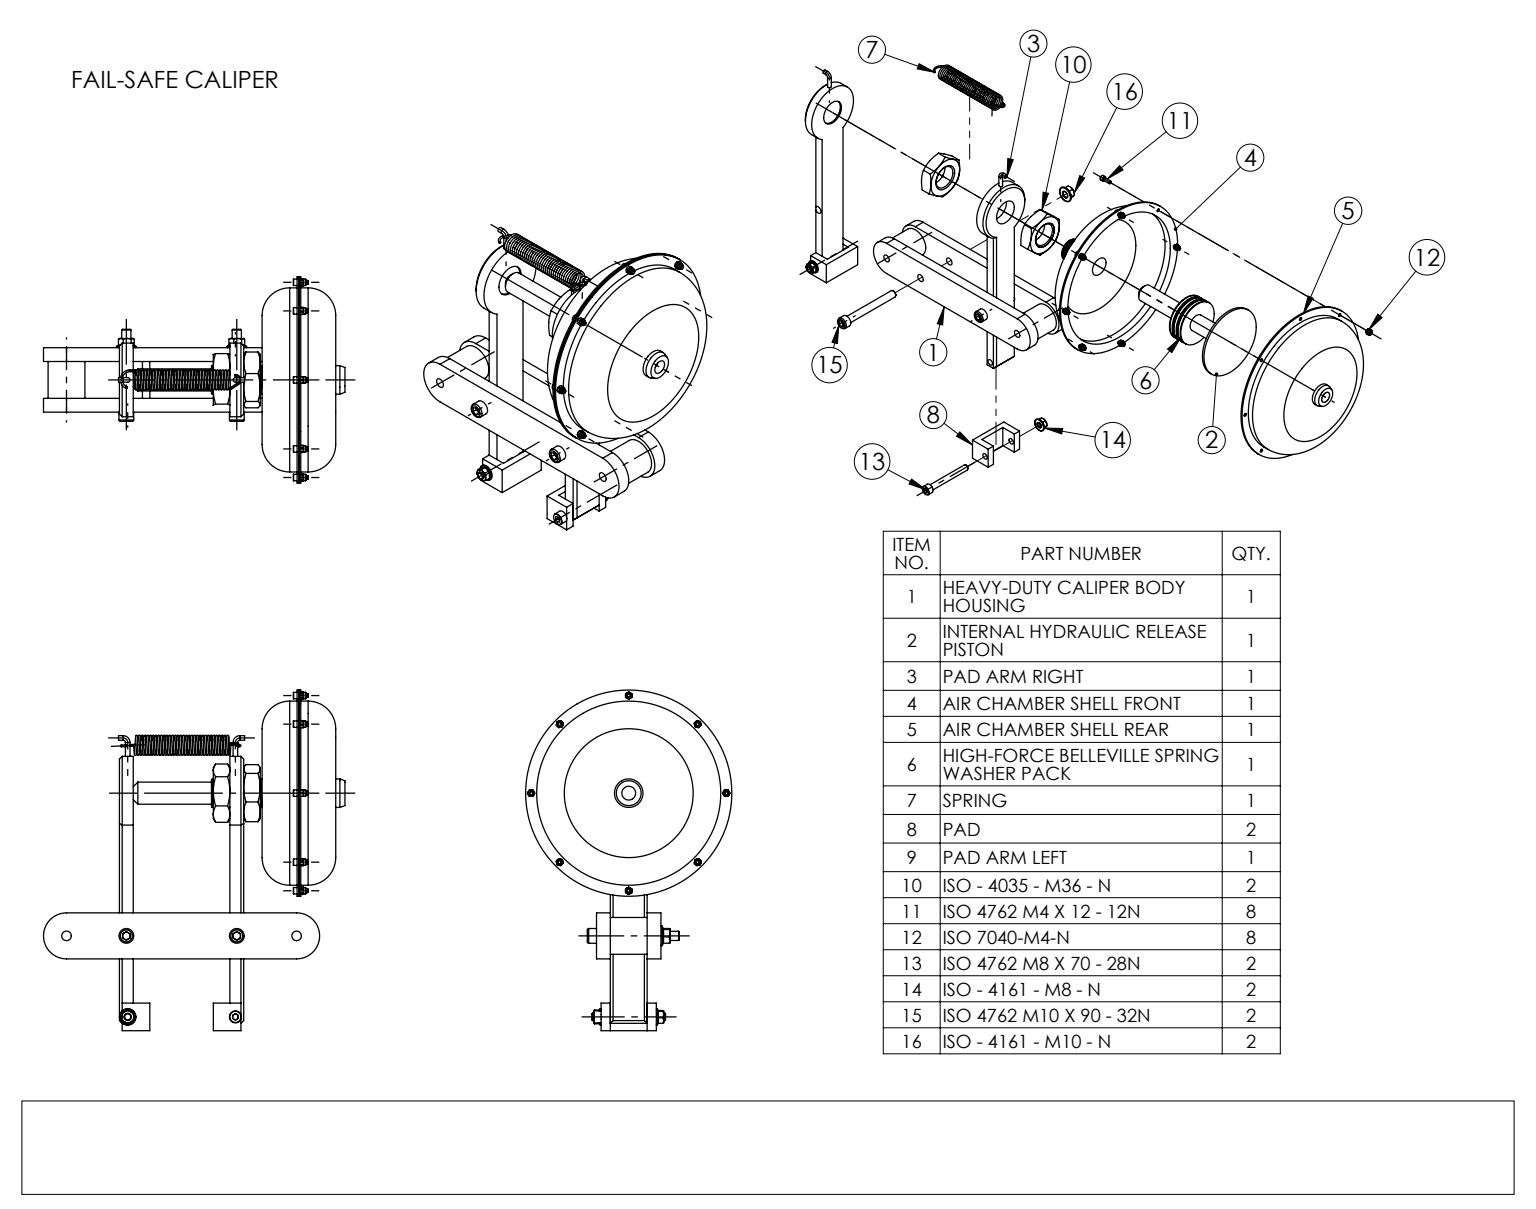
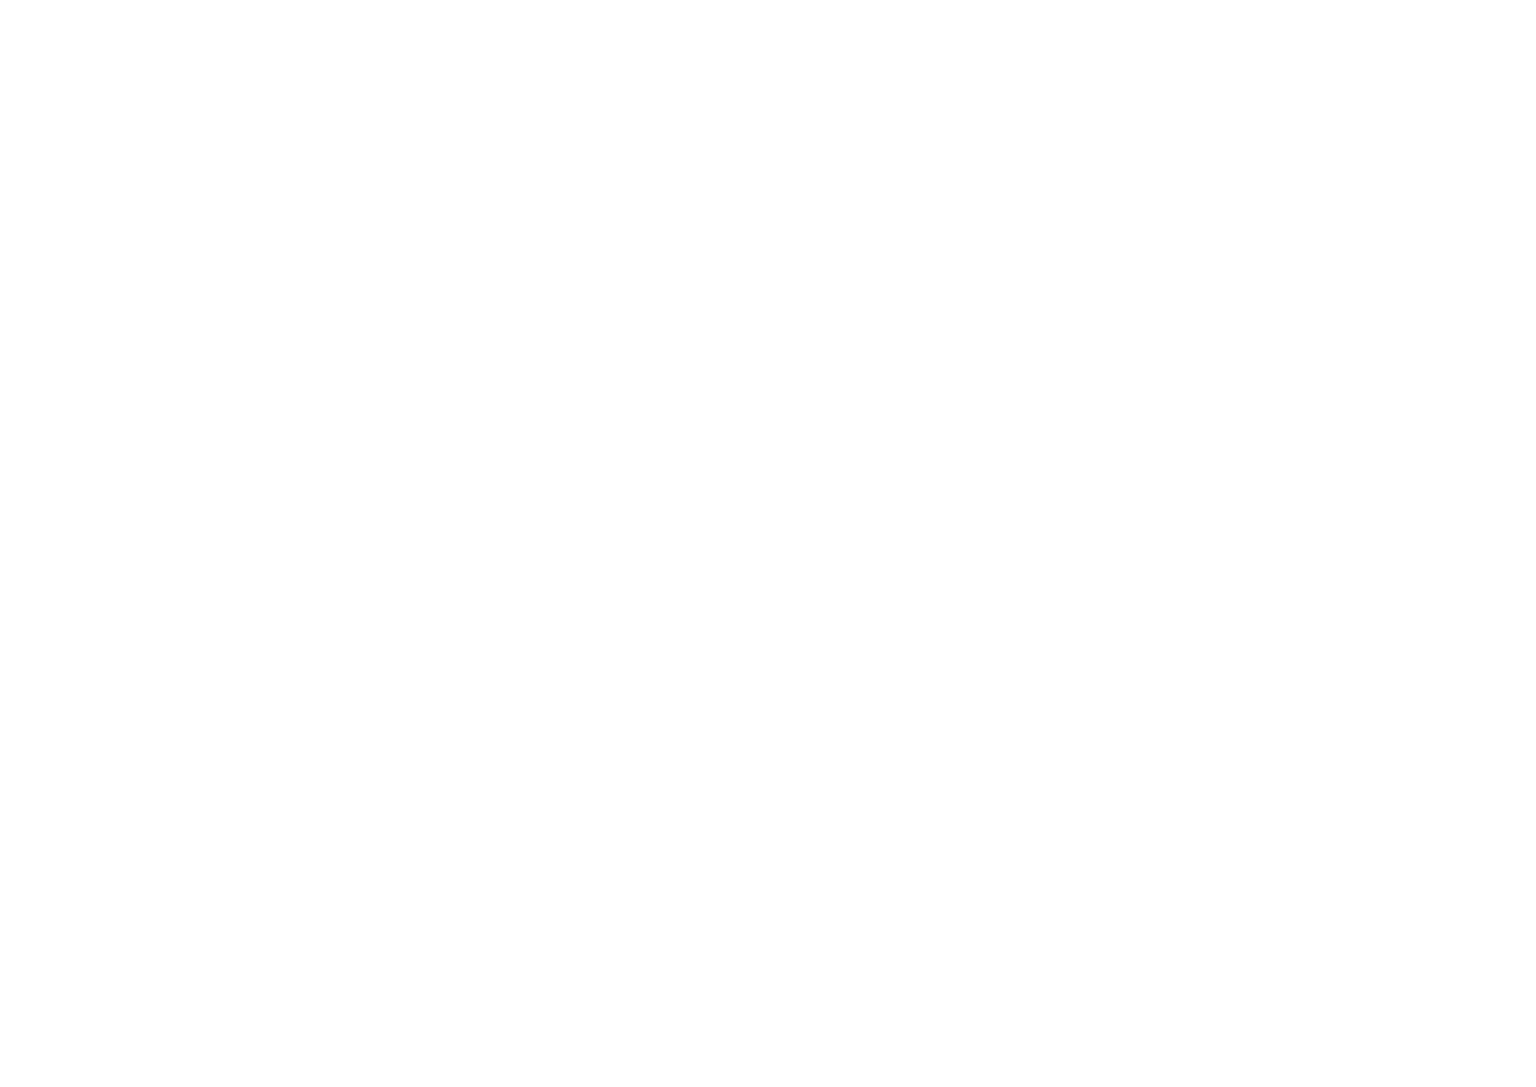
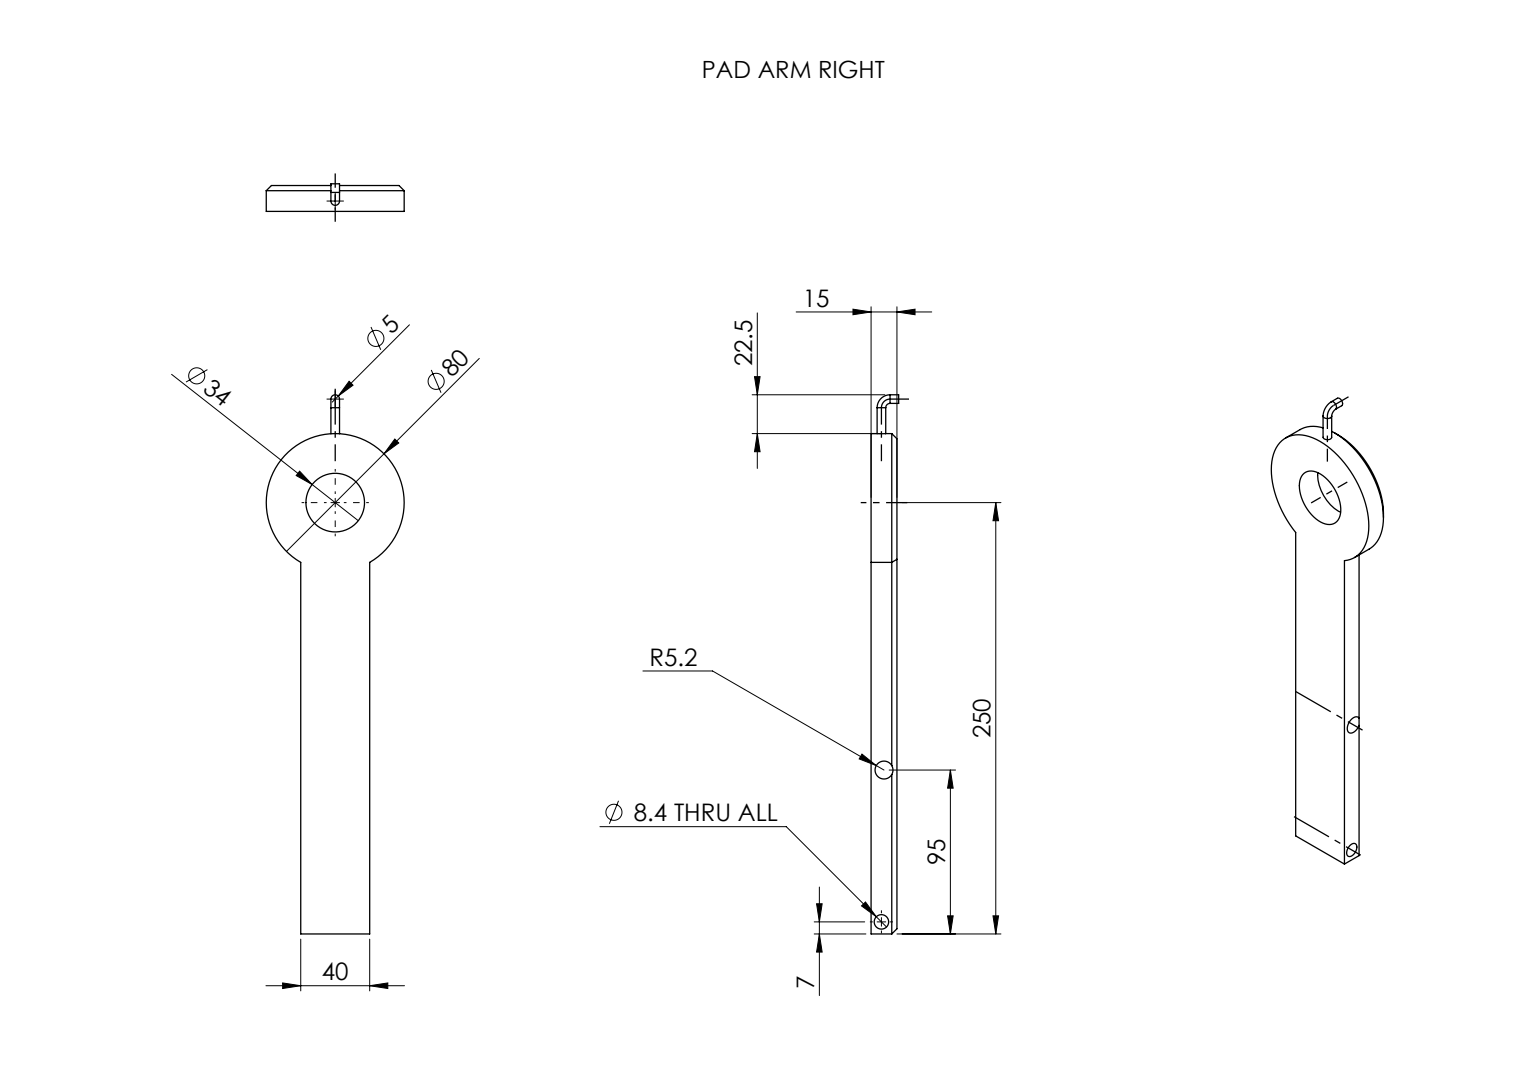
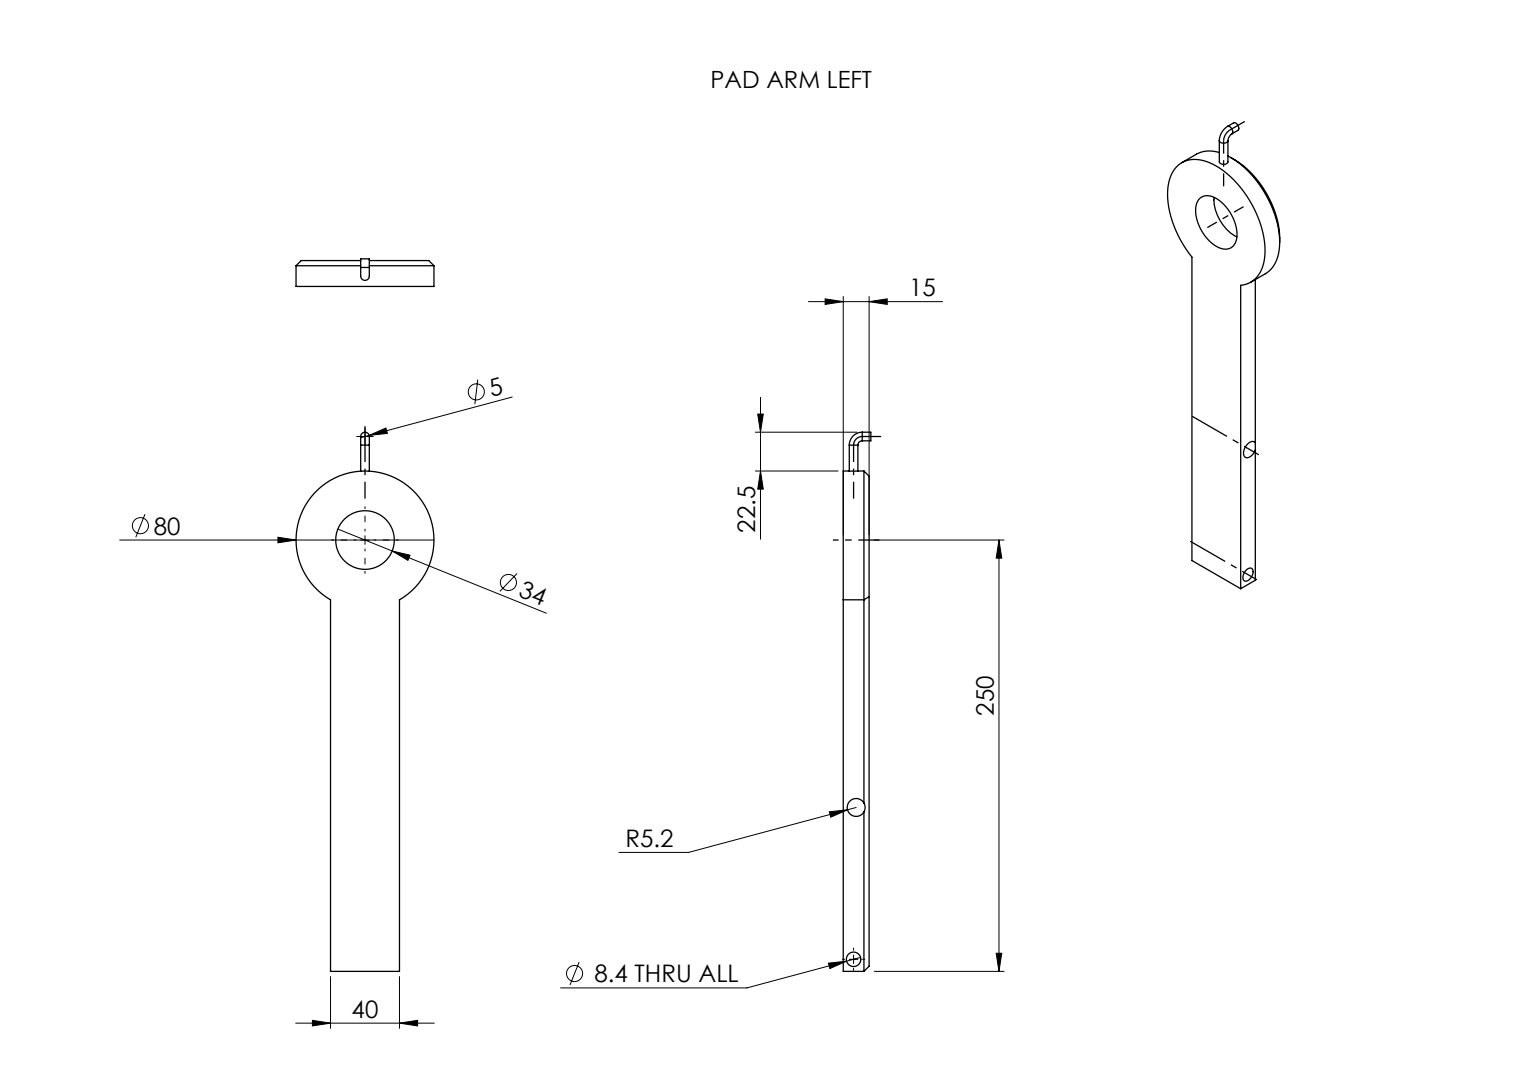
ISO-10303-21;
HEADER;
FILE_DESCRIPTION (('STEP AP214'),
    '1' );
FILE_NAME ('BR-600',
    '2026-10-08T07:58:12',
    ( '' ),
    ( '' ),
    'SwSTEP 2.0',
    'SolidWorks 2026',
    '' );
FILE_SCHEMA (( 'AUTOMOTIVE_DESIGN' ));
ENDSEC;

DATA;
#1 = EDGE_CURVE ( 'NONE', #21367, #4979, #7430, .T. ) ;
#2 = ORIENTED_EDGE ( 'NONE', *, *, #29028, .T. ) ;
#3 = CARTESIAN_POINT ( 'NONE',  ( 112.4999999999999858, 155.0000000000000000, -6.938893903907228378E-15 ) ) ;
#4 = DIRECTION ( 'NONE',  ( 0.000000000000000000, 0.000000000000000000, -1.000000000000000000 ) ) ;
#5 = ORIENTED_EDGE ( 'NONE', *, *, #16046, .F. ) ;
#6 = CARTESIAN_POINT ( 'NONE',  ( 2.517493886308900919, 214.5937144450984420, 40.40113791807857524 ) ) ;
#7 = DIRECTION ( 'NONE',  ( 0.000000000000000000, 0.000000000000000000, -1.000000000000000000 ) ) ;
#8 = CARTESIAN_POINT ( 'NONE',  ( -10.00000000000000711, 206.9523078486584495, 26.49886208192143755 ) ) ;
#9 = CARTESIAN_POINT ( 'NONE',  ( 60.97499999726881015, 140.1801316387863778, -4.815267126137194431 ) ) ;
#10 = ORIENTED_EDGE ( 'NONE', *, *, #1282, .F. ) ;
#11 = CARTESIAN_POINT ( 'NONE',  ( 68.68867513459484542, 150.1262045565065364, -15.00000000000012434 ) ) ;
#12 = SURFACE_SIDE_STYLE ('',( #18233 ) ) ;
#13 = DIRECTION ( 'NONE',  ( 0.000000000000000000, 0.000000000000000000, 1.000000000000000000 ) ) ;
#14 = CARTESIAN_POINT ( 'NONE',  ( 6.500168698208244500, 202.3363017425938324, 1.298862081921434930 ) ) ;
#15 = CARTESIAN_POINT ( 'NONE',  ( -8.118202686958039038, 201.1607312380087080, 39.20113791807857240 ) ) ;
#16 = DIRECTION ( 'NONE',  ( 1.000000000000000000, 0.000000000000000000, 0.000000000000000000 ) ) ;
#17 = CARTESIAN_POINT ( 'NONE',  ( -8.118202686958039038, 201.1607312380087080, 30.20113791807856884 ) ) ;
#18 = CARTESIAN_POINT ( 'NONE',  ( 6.220909254589680693, 198.5229672870052582, 103.4488620819214333 ) ) ;
#19 = APPLICATION_PROTOCOL_DEFINITION ( 'draft international standard', 'automotive_design', 1998, #29882 ) ;
#20 = CARTESIAN_POINT ( 'NONE',  ( 4.903702542908435547, 213.8346818373419751, 96.54886208192142760 ) ) ;
#21 = CARTESIAN_POINT ( 'NONE',  ( 33.32499999726881157, 164.1591823560292198, -12.60653300113719766 ) ) ;
#22 = SURFACE_SIDE_STYLE ('',( #2407 ) ) ;
#23 = LINE ( 'NONE', #2905, #21261 ) ;
#24 = CARTESIAN_POINT ( 'NONE',  ( -12.00000000000000711, 207.0476921513413515, 12.50113791807856600 ) ) ;
#25 = DIRECTION ( 'NONE',  ( -1.000000000000000000, 0.000000000000000000, 0.000000000000000000 ) ) ;
#26 = CARTESIAN_POINT ( 'NONE',  ( 57.37499999726880873, 155.0000000000000000, -15.58253175000000823 ) ) ;
#27 = ADVANCED_FACE ( 'NONE', ( #25458 ), #22740, .T. ) ;
#28 = CARTESIAN_POINT ( 'NONE',  ( 0.05014649552810505201, 217.5146222423826714, 58.25113791807856245 ) ) ;
#29 = EDGE_CURVE ( 'NONE', #11107, #14777, #31364, .T. ) ;
#30 = CARTESIAN_POINT ( 'NONE',  ( 87.72499999726882436, 169.8198683612136222, 4.815267126137181997 ) ) ;
#31 = CARTESIAN_POINT ( 'NONE',  ( 41.91132485994280188, 163.8167787843871110, -12.13525491562423397 ) ) ;
#32 = DIRECTION ( 'NONE',  ( -0.000000000000000000, -0.000000000000000000, -1.000000000000000000 ) ) ;
#33 = CARTESIAN_POINT ( 'NONE',  ( 51.79999999453762882, 146.4771138417591203, -11.73074641843674470 ) ) ;
#34 = EDGE_LOOP ( 'NONE', ( #21556, #29225, #7331, #33094 ) ) ;
#35 = CARTESIAN_POINT ( 'NONE',  ( -7.456977232089304408, 196.8216656703010301, 42.05113791807857382 ) ) ;
#36 = EDGE_CURVE ( 'NONE', #1409, #6493, #16652, .T. ) ;
#37 = PLANE ( 'NONE',  #25790 ) ;
#38 = CARTESIAN_POINT ( 'NONE',  ( -10.00000000000000711, 206.9523078486584495, 8.498862081921433997 ) ) ;
#39 = CARTESIAN_POINT ( 'NONE',  ( 60.11132485994280472, 169.2658477444273331, -4.635254915624224203 ) ) ;
#40 = ORIENTED_EDGE ( 'NONE', *, *, #21984, .F. ) ;
#41 = CARTESIAN_POINT ( 'NONE',  ( -10.00000000000000711, 207.0476921513413515, 6.501137918078566003 ) ) ;
#42 = CARTESIAN_POINT ( 'NONE',  ( -3.044812012440131443, 216.5253028482142952, 70.10113791807857808 ) ) ;
#43 = EDGE_CURVE ( 'NONE', #14229, #27576, #23397, .T. ) ;
#44 = ORIENTED_EDGE ( 'NONE', *, *, #27793, .F. ) ;
#45 = CARTESIAN_POINT ( 'NONE',  ( -2.517493886309087880, 214.5937144450984135, 36.09886208192144608 ) ) ;
#46 = CARTESIAN_POINT ( 'NONE',  ( 43.71132485994280614, 155.0000000000000000, -15.00000000000002487 ) ) ;
#47 = EDGE_LOOP ( 'NONE', ( #1882, #26577, #33467, #1949, #7115, #1431 ) ) ;
#48 = CARTESIAN_POINT ( 'NONE',  ( 2.517493886308900919, 214.5937144450984420, 16.40113791807856458 ) ) ;
#49 = CARTESIAN_POINT ( 'NONE',  ( -9.736236675708031640, 214.0148392665760753, 95.79886208192144181 ) ) ;
#50 = CARTESIAN_POINT ( 'NONE',  ( 42.47499999726881015, 149.9369285172503510, 15.58253174999999580 ) ) ;
#51 = ORIENTED_EDGE ( 'NONE', *, *, #2660, .T. ) ;
#52 = CARTESIAN_POINT ( 'NONE',  ( 47.92499999726881299, 164.1591823560292198, 12.60653300113718167 ) ) ;
#53 = CARTESIAN_POINT ( 'NONE',  ( 124.3127766070272315, 5.250000000000032863, 35.00001199999999812 ) ) ;
#54 = CARTESIAN_POINT ( 'NONE',  ( 3.044812012440130555, 197.4746971517856764, 5.601137918078566535 ) ) ;
#55 = CARTESIAN_POINT ( 'NONE',  ( 6.220909254589681581, 198.5229672870052582, 76.44886208192143329 ) ) ;
#56 = CARTESIAN_POINT ( 'NONE',  ( 50.77499999726880731, 140.1801316387863778, 4.815267126137185549 ) ) ;
#57 = DIRECTION ( 'NONE',  ( 0.000000000000000000, -1.000000000000000000, 0.000000000000000000 ) ) ;
#58 = CARTESIAN_POINT ( 'NONE',  ( 10.00000000000000711, 206.9523078486586201, 11.00113791807856600 ) ) ;
#59 = DIRECTION ( 'NONE',  ( -0.000000000000000000, -0.000000000000000000, -1.000000000000000000 ) ) ;
#60 = CARTESIAN_POINT ( 'NONE',  ( 65.20000000000001705, 167.3344367211045096, 8.961492836873468093 ) ) ;
#61 = CARTESIAN_POINT ( 'NONE',  ( -8.118202686958039038, 201.1607312380087080, 99.20113791807858661 ) ) ;
#62 = CARTESIAN_POINT ( 'NONE',  ( -27.49999999999999645, -5.348566131067992835, -0.2306174136865311308 ) ) ;
#63 = CARTESIAN_POINT ( 'NONE',  ( 9.984503880673470277, 203.7031108863295401, 86.15113791807857524 ) ) ;
#64 = CARTESIAN_POINT ( 'NONE',  ( -6.500000000000000000, -3.752776749732572803, -8.000000000000000000 ) ) ;
#65 = DIRECTION ( 'NONE',  ( 0.000000000000000000, 0.000000000000000000, 1.000000000000000000 ) ) ;
#66 = CARTESIAN_POINT ( 'NONE',  ( -3.662846001189865142, 195.5725841191952838, 94.89886208192145034 ) ) ;
#67 = CARTESIAN_POINT ( 'NONE',  ( 67.92499999726881299, 164.1591823560292198, 12.60653300113718167 ) ) ;
#68 = ORIENTED_EDGE ( 'NONE', *, *, #26579, .F. ) ;
#69 = CARTESIAN_POINT ( 'NONE',  ( -59.30520453566667527, 194.9296309105606326, -2.372451168785852715 ) ) ;
#70 = CARTESIAN_POINT ( 'NONE',  ( 37.59999999453762598, 141.2096805137202580, -4.480746418436742040 ) ) ;
#71 = CARTESIAN_POINT ( 'NONE',  ( -9.680171189290831535, 214.0920067884431148, 99.80113791807858092 ) ) ;
#72 = DIRECTION ( 'NONE',  ( -1.000000000000000000, -0.000000000000000000, -0.000000000000000000 ) ) ;
#73 = VERTEX_POINT ( 'NONE', #11840 ) ;
#74 = CARTESIAN_POINT ( 'NONE',  ( -6.139770520408224463, 198.4640165459539105, 89.04886208192141339 ) ) ;
#75 = AXIS2_PLACEMENT_3D ( 'NONE', #16121, #13402, #469 ) ;
#76 = CARTESIAN_POINT ( 'NONE',  ( 12.00000000000000711, 207.0476921513415220, 24.99886208192143400 ) ) ;
#77 = DIRECTION ( 'NONE',  ( -1.000000000000000000, -0.000000000000000000, -0.000000000000000000 ) ) ;
#78 = CARTESIAN_POINT ( 'NONE',  ( 6.220909254589536808, 215.4770327129947702, 40.55113791807855250 ) ) ;
#79 = ORIENTED_EDGE ( 'NONE', *, *, #5370, .F. ) ;
#80 = CARTESIAN_POINT ( 'NONE',  ( -2.426778023690076225, 199.3768101843759553, 7.898862081921436129 ) ) ;
#81 = CARTESIAN_POINT ( 'NONE',  ( -0.2855619784720687115, 3.876582599186216616, -0.2174200650117638633 ) ) ;
#82 = VERTEX_POINT ( 'NONE', #32615 ) ;
#83 = CARTESIAN_POINT ( 'NONE',  ( 2.517493886309087436, 199.4062855549015865, 91.59886208192145318 ) ) ;
#84 = EDGE_LOOP ( 'NONE', ( #4042, #16247, #32529, #21714 ) ) ;
#85 =( REPRESENTATION_RELATIONSHIP ('NONE','NONE', #25663, #30243 ) REPRESENTATION_RELATIONSHIP_WITH_TRANSFORMATION ( #16669 )SHAPE_REPRESENTATION_RELATIONSHIP( ) );
#86 = CARTESIAN_POINT ( 'NONE',  ( 8.015496119326531499, 209.5516654185219636, 31.85113791807857453 ) ) ;
#87 = DIRECTION ( 'NONE',  ( 0.000000000000000000, -1.000000000000000000, 0.000000000000000000 ) ) ;
#88 = ORIENTED_EDGE ( 'NONE', *, *, #21349, .T. ) ;
#89 = CARTESIAN_POINT ( 'NONE',  ( 5.147825380264231754, 5.688155668806028409, -7.450218641347809090 ) ) ;
#90 = CARTESIAN_POINT ( 'NONE',  ( 80.92499999726882720, 145.8408176439707802, -12.60653300113719588 ) ) ;
#91 = CARTESIAN_POINT ( 'NONE',  ( 87.50000000000001421, 155.0000000000000000, -6.938893903907228378E-15 ) ) ;
#92 = CARTESIAN_POINT ( 'NONE',  ( 8.015496119326531499, 209.5516654185219636, 88.85113791807857808 ) ) ;
#93 = PLANE ( 'NONE',  #4285 ) ;
#94 = PRESENTATION_STYLE_ASSIGNMENT (( #8103 ) ) ;
#95 = CARTESIAN_POINT ( 'NONE',  ( 50.79999999999999716, 167.3344367211045096, -8.961492836873482304 ) ) ;
#96 = CARTESIAN_POINT ( 'NONE',  ( 4.984841277089891776, 200.2242689037093726, 67.44886208192143329 ) ) ;
#97 = CARTESIAN_POINT ( 'NONE',  ( 27.50000000000001066, -2.682974265912531742, -6.098637220230963674E-17 ) ) ;
#98 = CARTESIAN_POINT ( 'NONE',  ( 53.82499999726881157, 168.2552932293087906, 9.630534252274372875 ) ) ;
#99 = CARTESIAN_POINT ( 'NONE',  ( 6.220909254589536808, 215.4770327129947987, 4.551137918078565825 ) ) ;
#100 = CARTESIAN_POINT ( 'NONE',  ( -7.500000000000000000, 4.330127018922191873, -7.422398894150032511 ) ) ;
#101 = CIRCLE ( 'NONE', #26212, 13.50000000000001066 ) ;
#102 = CARTESIAN_POINT ( 'NONE',  ( 55.42499999726880588, 168.2552932293087906, -9.630534252274387086 ) ) ;
#103 = CARTESIAN_POINT ( 'NONE',  ( 67.97499999726881015, 169.8198683612136222, 4.815267126137181997 ) ) ;
#104 = CARTESIAN_POINT ( 'NONE',  ( -7.375838497908182134, 217.2372850707499765, 63.95113791807857240 ) ) ;
#105 = CARTESIAN_POINT ( 'NONE',  ( 46.01132485994281041, 167.7597621252805880, -9.270509831248443078 ) ) ;
#106 = CARTESIAN_POINT ( 'NONE',  ( -3.753561863808691168, 195.6020594897209435, 5.901137918078566358 ) ) ;
#107 = CARTESIAN_POINT ( 'NONE',  ( 0.05014649552810506589, 217.5146222423826714, 88.25113791807858377 ) ) ;
#108 = CARTESIAN_POINT ( 'NONE',  ( 35.38867513459481273, 169.2658477444273331, 4.635254915624208216 ) ) ;
#109 = CARTESIAN_POINT ( 'NONE',  ( 12.00000000000000711, 207.0476921513415220, 48.99886208192143044 ) ) ;
#110 = CARTESIAN_POINT ( 'NONE',  ( 3.135527875058981895, 197.5041725223112792, 61.59886208192143897 ) ) ;
#111 = CARTESIAN_POINT ( 'NONE',  ( -0.05014649552807705357, 194.3824533091408000, 98.75113791807856956 ) ) ;
#112 = CARTESIAN_POINT ( 'NONE',  ( -67.50001199999999812, 168.5168296348864203, 10.36982646209945891 ) ) ;
#113 = CARTESIAN_POINT ( 'NONE',  ( -6.220909254589537696, 198.5229672870051161, 15.05113791807856671 ) ) ;
#114 = CARTESIAN_POINT ( 'NONE',  ( 6.139770520408223575, 215.5359834540460611, 75.54886208192139918 ) ) ;
#115 = EDGE_CURVE ( 'NONE', #13221, #23693, #5798, .T. ) ;
#116 = ORIENTED_EDGE ( 'NONE', *, *, #1238, .F. ) ;
#117 = CARTESIAN_POINT ( 'NONE',  ( -3.753561863808878130, 218.3979405102790281, 78.09886208192142476 ) ) ;
#118 = AXIS2_PLACEMENT_3D ( 'NONE', #27781, #9730, #4445 ) ;
#119 = CARTESIAN_POINT ( 'NONE',  ( -6.220909254589537696, 198.5229672870051161, 102.0511379180785383 ) ) ;
#120 = ORIENTED_EDGE ( 'NONE', *, *, #31535, .T. ) ;
#121 = CYLINDRICAL_SURFACE ( 'NONE', #25443, 15.00000000000001776 ) ;
#122 = CARTESIAN_POINT ( 'NONE',  ( 2.426778023690075337, 214.6231898156240447, 60.39886208192144323 ) ) ;
#123 = ORIENTED_EDGE ( 'NONE', *, *, #8294, .T. ) ;
#124 = CARTESIAN_POINT ( 'NONE',  ( 70.92499999726881299, 145.8408176439707802, -12.60653300113719588 ) ) ;
#125 = CARTESIAN_POINT ( 'NONE',  ( -56.25402757683428234, 194.9848779240976171, -1.110136720165091129 ) ) ;
#126 = CONICAL_SURFACE ( 'NONE', #19149, 32.00000000000005684, 0.1047197551196217685 ) ;
#127 = UNCERTAINTY_MEASURE_WITH_UNIT (LENGTH_MEASURE( 1.000000000000000082E-05 ), #13064, 'distance_accuracy_value', 'NONE');
#128 = CARTESIAN_POINT ( 'NONE',  ( 63.72499999726881015, 169.8198683612136222, 4.815267126137181997 ) ) ;
#129 = FACE_OUTER_BOUND ( 'NONE', #16222, .T. ) ;
#130 = CARTESIAN_POINT ( 'NONE',  ( 8.118202686958138514, 201.1607312380088501, 55.29886208192144181 ) ) ;
#131 = ORIENTED_EDGE ( 'NONE', *, *, #28510, .T. ) ;
#132 = DIRECTION ( 'NONE',  ( 1.000000000000000000, 0.000000000000000000, 0.000000000000000000 ) ) ;
#133 =( LENGTH_UNIT ( ) NAMED_UNIT ( * ) SI_UNIT ( .MILLI., .METRE. ) );
#134 = CARTESIAN_POINT ( 'NONE',  ( 108.1100194822685836, 155.0000000000000000, 0.000000000000000000 ) ) ;
#135 = CARTESIAN_POINT ( 'NONE',  ( -4.903702542908436435, 200.1653181626580249, 38.04886208192144892 ) ) ;
#136 = CARTESIAN_POINT ( 'NONE',  ( 10.01549611932653860, 210.2015048109876716, 67.85113791807857808 ) ) ;
#137 = CARTESIAN_POINT ( 'NONE',  ( 44.78867513459481842, 155.0000000000000000, -15.00000000000002487 ) ) ;
#138 = CARTESIAN_POINT ( 'NONE',  ( 10.01549611932653860, 210.2015048109876716, 58.85113791807856387 ) ) ;
#139 = AXIS2_PLACEMENT_3D ( 'NONE', #22504, #24891, #17559 ) ;
#140 = CARTESIAN_POINT ( 'NONE',  ( -8.118202686958039038, 201.1607312380087080, 24.20113791807856884 ) ) ;
#141 = CARTESIAN_POINT ( 'NONE',  ( -8.000000000000008882, 207.0476921513413515, 18.50113791807856956 ) ) ;
#142 = CARTESIAN_POINT ( 'NONE',  ( -58.50000000000001421, -88.00000000000000000, -20.00000000000000000 ) ) ;
#143 = CARTESIAN_POINT ( 'NONE',  ( 0.000000000000000000, 0.000000000000000000, -20.00000000000000000 ) ) ;
#144 = CARTESIAN_POINT ( 'NONE',  ( 40.12499999726880873, 155.0000000000000000, 15.58253174999999402 ) ) ;
#145 = CARTESIAN_POINT ( 'NONE',  ( -7.375838497908182134, 217.2372850707499765, 39.95113791807856529 ) ) ;
#146 = CARTESIAN_POINT ( 'NONE',  ( 1.126429428730187032, -7.232124035235040438, -6.344710093416088270 ) ) ;
#147 = CARTESIAN_POINT ( 'NONE',  ( 9.984503880673470277, 203.7031108863295401, 83.15113791807853261 ) ) ;
#148 = CARTESIAN_POINT ( 'NONE',  ( -0.05014649552810635652, 196.4853777576173002, 56.75113791807856245 ) ) ;
#149 = CARTESIAN_POINT ( 'NONE',  ( -9.736236675708031640, 214.0148392665760753, 23.79886208192143826 ) ) ;
#150 = CARTESIAN_POINT ( 'NONE',  ( 0.05014649552828275014, 196.4853777576173002, 31.74886208192143044 ) ) ;
#151 = CARTESIAN_POINT ( 'NONE',  ( 77.49999999453761745, 139.7537977485451393, -4.138211985947621020E-15 ) ) ;
#152 = CIRCLE ( 'NONE', #30594, 3.999999999999999112 ) ;
#153 = CARTESIAN_POINT ( 'NONE',  ( -9.680171189290831535, 214.0920067884431148, 69.80113791807856671 ) ) ;
#154 = CARTESIAN_POINT ( 'NONE',  ( -8.000000000000008882, 207.0476921513413515, 87.50113791807856956 ) ) ;
#155 = VECTOR ( 'NONE', #28010, 1000.000000000000000 ) ;
#156 = CARTESIAN_POINT ( 'NONE',  ( 8.118202686958138514, 201.1607312380088501, 49.29886208192143471 ) ) ;
#157 = EDGE_CURVE ( 'NONE', #28109, #32153, #10692, .T. ) ;
#158 = CARTESIAN_POINT ( 'NONE',  ( 48.78867513459482552, 155.0000000000000000, -15.00000000000002487 ) ) ;
#159 = ORIENTED_EDGE ( 'NONE', *, *, #2470, .T. ) ;
#160 = CARTESIAN_POINT ( 'NONE',  ( -9.736236675708031640, 214.0148392665760753, 50.79886208192143471 ) ) ;
#161 = VERTEX_POINT ( 'NONE', #19672 ) ;
#162 = ORIENTED_EDGE ( 'NONE', *, *, #20206, .F. ) ;
#163 = CARTESIAN_POINT ( 'NONE',  ( 51.68867513459483831, 159.8737954434934920, 15.00000000000010836 ) ) ;
#164 = EDGE_CURVE ( 'NONE', #11179, #4391, #29721, .T. ) ;
#165 = VECTOR ( 'NONE', #3398, 1000.000000000000000 ) ;
#166 = CYLINDRICAL_SURFACE ( 'NONE', #13806, 5.249999999999991118 ) ;
#167 = CARTESIAN_POINT ( 'NONE',  ( -6.444103211791042618, 211.7408657792732356, 39.80113791807857382 ) ) ;
#168 = FILL_AREA_STYLE ('',( #5443 ) ) ;
#169 = CARTESIAN_POINT ( 'NONE',  ( -10.00000000000000711, 206.9523078486584495, 23.49886208192143755 ) ) ;
#170 = CARTESIAN_POINT ( 'NONE',  ( 62.97499999726881015, 140.1801316387863778, -4.815267126137194431 ) ) ;
#171 = VERTEX_POINT ( 'NONE', #1955 ) ;
#172 = DIRECTION ( 'NONE',  ( 0.000000000000000000, 0.000000000000000000, 1.000000000000000000 ) ) ;
#173 = AXIS2_PLACEMENT_3D ( 'NONE', #29896, #20170, #1948 ) ;
#174 =( NAMED_UNIT ( * ) SI_UNIT ( $, .STERADIAN. ) SOLID_ANGLE_UNIT ( ) );
#175 = LINE ( 'NONE', #28457, #23884 ) ;
#176 = CARTESIAN_POINT ( 'NONE',  ( -7.984503880673422316, 204.3529502787951628, 8.348862081921435419 ) ) ;
#177 = VECTOR ( 'NONE', #7747, 1000.000000000000000 ) ;
#178 = CARTESIAN_POINT ( 'NONE',  ( -8.118202686958039038, 201.1607312380087080, 42.20113791807857240 ) ) ;
#179 = EDGE_CURVE ( 'NONE', #29148, #5220, #18847, .T. ) ;
#180 = CARTESIAN_POINT ( 'NONE',  ( -9.984503880673473830, 210.2968891136704315, 30.65113791807856813 ) ) ;
#181 = CARTESIAN_POINT ( 'NONE',  ( -6.139770520408224463, 198.4640165459539105, 104.0488620819214276 ) ) ;
#182 = AXIS2_PLACEMENT_3D ( 'NONE', #23295, #23628, #33351 ) ;
#183 = APPLICATION_PROTOCOL_DEFINITION ( 'draft international standard', 'automotive_design', 1998, #11815 ) ;
#184 = CARTESIAN_POINT ( 'NONE',  ( -6.444103211790928043, 202.2591342207265939, 92.19886208192143329 ) ) ;
#185 = CARTESIAN_POINT ( 'NONE',  ( 86.00000000000001421, 139.7537977485451393, -4.138211985947621020E-15 ) ) ;
#186 = CARTESIAN_POINT ( 'NONE',  ( 81.68867513459483121, 159.8737954434934920, 15.00000000000010836 ) ) ;
#187 = CARTESIAN_POINT ( 'NONE',  ( 107.5000000000000000, 155.0000000000000000, -6.938893903907228378E-15 ) ) ;
#188 = CARTESIAN_POINT ( 'NONE',  ( 3.662846001190051659, 195.5725841191953691, 5.601137918078566535 ) ) ;
#189 = CARTESIAN_POINT ( 'NONE',  ( 90.49452189536829394, 155.0000000000000000, 0.000000000000000000 ) ) ;
#190 = CARTESIAN_POINT ( 'NONE',  ( 59.07499999726880446, 141.7447067706911810, -9.630534252274385310 ) ) ;
#191 = EDGE_CURVE ( 'NONE', #26009, #2264, #14724, .T. ) ;
#192 = CARTESIAN_POINT ( 'NONE',  ( 6.139770520408368348, 198.4640165459539674, 56.45113791807857950 ) ) ;
#193 = CARTESIAN_POINT ( 'NONE',  ( -10.01549611932653860, 203.7984951890123000, 27.35113791807856742 ) ) ;
#194 = CARTESIAN_POINT ( 'NONE',  ( 87.92499999726881299, 164.1591823560292198, 12.60653300113718167 ) ) ;
#195 = CIRCLE ( 'NONE', #24668, 12.10452846326762177 ) ;
#196 = CARTESIAN_POINT ( 'NONE',  ( 93.60208470531338776, 155.0000000000000000, 12.00000000000001066 ) ) ;
#197 = DIRECTION ( 'NONE',  ( 0.000000000000000000, 0.000000000000000000, -1.000000000000000000 ) ) ;
#198 = CARTESIAN_POINT ( 'NONE',  ( 58.39999999453763024, 168.7903194862797420, -4.480746418436745593 ) ) ;
#199 = EDGE_LOOP ( 'NONE', ( #6046, #19847, #15492, #25201, #18551, #25086 ) ) ;
#200 = CARTESIAN_POINT ( 'NONE',  ( 3.662846001190051659, 195.5725841191953691, 41.60113791807857098 ) ) ;
#201 = CARTESIAN_POINT ( 'NONE',  ( 0.000000000000000000, 0.000000000000000000, 2.066666666667000385 ) ) ;
#202 = CARTESIAN_POINT ( 'NONE',  ( -8.118202686958138514, 212.8392687619910930, 11.79886208192143471 ) ) ;
#203 = DIRECTION ( 'NONE',  ( 0.000000000000000000, 0.000000000000000000, 1.000000000000000000 ) ) ;
#204 = ORIENTED_EDGE ( 'NONE', *, *, #10925, .T. ) ;
#205 = CARTESIAN_POINT ( 'NONE',  ( 10.00000000000000711, 206.9523078486586201, 71.00113791807858377 ) ) ;
#206 = CIRCLE ( 'NONE', #7281, 100.0000000000000284 ) ;
#207 = ORIENTED_EDGE ( 'NONE', *, *, #12087, .F. ) ;
#208 = CARTESIAN_POINT ( 'NONE',  ( 4.984841277089891776, 200.2242689037093726, 31.44886208192143684 ) ) ;
#209 = CARTESIAN_POINT ( 'NONE',  ( 11.41286821541921803, -25.16504226903143149, -17.92845254598169902 ) ) ;
#210 = VERTEX_POINT ( 'NONE', #17453 ) ;
#211 = CARTESIAN_POINT ( 'NONE',  ( -8.015496119326531499, 204.4483345814780364, 9.351137918078563871 ) ) ;
#212 = EDGE_CURVE ( 'NONE', #5261, #24452, #30622, .T. ) ;
#213 = EDGE_CURVE ( 'NONE', #19514, #25076, #28012, .T. ) ;
#214 = CARTESIAN_POINT ( 'NONE',  ( 11.98450388067341876, 210.9467285061363953, 93.84886208192143897 ) ) ;
#215 = CARTESIAN_POINT ( 'NONE',  ( 43.97499999726881015, 169.8198683612136222, 4.815267126137181997 ) ) ;
#216 = ORIENTED_EDGE ( 'NONE', *, *, #22229, .T. ) ;
#217 = CARTESIAN_POINT ( 'NONE',  ( 53.12499999726881583, 155.0000000000000000, -15.58253175000000823 ) ) ;
#218 = CARTESIAN_POINT ( 'NONE',  ( 127.6439996469472220, 4.587378538859885779, 35.00001200000000523 ) ) ;
#219 = CARTESIAN_POINT ( 'NONE',  ( -6.139770520408369237, 215.5359834540460042, 6.951137918078566180 ) ) ;
#220 = AXIS2_PLACEMENT_3D ( 'NONE', #21698, #13527, #16251 ) ;
#221 = CARTESIAN_POINT ( 'NONE',  ( 8.062137200540822946, 212.9164362838583315, 81.69886208192143329 ) ) ;
#223 = CARTESIAN_POINT ( 'NONE',  ( 53.77499999726881441, 169.8198683612136222, -4.815267126137197984 ) ) ;
#222 = PRODUCT_RELATED_PRODUCT_CATEGORY ( 'part', '', ( #29822 ) ) ;
#224 = DIRECTION ( 'NONE',  ( -2.312964634635740985E-16, 1.000000000000000000, 0.000000000000000000 ) ) ;
#225 = CARTESIAN_POINT ( 'NONE',  ( 8.062137200540920645, 201.0835637161417822, 17.30113791807856671 ) ) ;
#226 = DIRECTION ( 'NONE',  ( 1.000000000000000000, 0.000000000000000000, 0.000000000000000000 ) ) ;
#227 = EDGE_CURVE ( 'NONE', #17881, #23868, #23670, .T. ) ;
#228 = CIRCLE ( 'NONE', #27934, 13.00000000000001066 ) ;
#229 = CARTESIAN_POINT ( 'NONE',  ( 67.70000000000001705, 146.4771138417591203, 11.73074641843673227 ) ) ;
#230 = DIRECTION ( 'NONE',  ( 1.000000000000000000, 0.000000000000000000, 0.000000000000000000 ) ) ;
#231 = DIRECTION ( 'NONE',  ( -1.000000000000000000, 0.000000000000000000, -0.000000000000000000 ) ) ;
#232 = CARTESIAN_POINT ( 'NONE',  ( -10.01549611932653860, 203.7984951890123284, 81.35113791807857808 ) ) ;
#233 = AXIS2_PLACEMENT_3D ( 'NONE', #28448, #5105, #25888 ) ;
#234 = CARTESIAN_POINT ( 'NONE',  ( 37.97499999726881015, 169.8198683612136222, 4.815267126137181997 ) ) ;
#235 = EDGE_CURVE ( 'NONE', #32873, #16396, #27571, .T. ) ;
#236 = CARTESIAN_POINT ( 'NONE',  ( 3.753561863808876797, 195.6020594897209719, 94.59886208192145318 ) ) ;
#237 = B_SPLINE_CURVE_WITH_KNOTS ( 'NONE', 3,
 ( #14921, #6748, #30598, #12365, #7263, #16962 ),
 .UNSPECIFIED., .F., .F.,
 ( 4, 2, 4 ),
 ( 0.005511122051665409173, 0.007432374760074394321, 0.009353627468483380336 ),
 .UNSPECIFIED. ) ;
#238 = CARTESIAN_POINT ( 'NONE',  ( 69.42499999726881299, 168.2552932293087906, -9.630534252274385310 ) ) ;
#239 = EDGE_LOOP ( 'NONE', ( #2645, #22396, #19117, #16780 ) ) ;
#240 = CARTESIAN_POINT ( 'NONE',  ( -60.15146012614710003, 194.9557722165940845, -1.884122726181822971 ) ) ;
#241 = CARTESIAN_POINT ( 'NONE',  ( 39.59999999453763309, 141.2096805137202580, -4.480746418436742040 ) ) ;
#242 = CARTESIAN_POINT ( 'NONE',  ( -12.01549611932652972, 203.1486557965464499, 96.35113791807857808 ) ) ;
#243 = CARTESIAN_POINT ( 'NONE',  ( 3.469446951953614189E-15, -4.041451884327432076, -2.899999999999999911 ) ) ;
#244 = ORIENTED_EDGE ( 'NONE', *, *, #9158, .T. ) ;
#245 = STYLED_ITEM ( 'NONE', ( #10197 ), #10045 ) ;
#246 = CARTESIAN_POINT ( 'NONE',  ( -6.220909254589682469, 215.4770327129947134, 95.94886208192143329 ) ) ;
#247 = CARTESIAN_POINT ( 'NONE',  ( -9.736236675708031640, 214.0148392665760753, 26.79886208192143826 ) ) ;
#248 = CARTESIAN_POINT ( 'NONE',  ( -64.50000000000000000, -95.00000000000000000, 270.4495957273638282 ) ) ;
#249 = CARTESIAN_POINT ( 'NONE',  ( 10.00000000000000711, 206.9523078486586201, 47.00113791807856956 ) ) ;
#250 = VERTEX_POINT ( 'NONE', #3251 ) ;
#251 = CARTESIAN_POINT ( 'NONE',  ( -3.044812012439970683, 197.4746971517856196, 103.8988620819214361 ) ) ;
#252 = CIRCLE ( 'NONE', #19276, 6.500000000000000888 ) ;
#253 = VERTEX_POINT ( 'NONE', #11433 ) ;
#254 = CARTESIAN_POINT ( 'NONE',  ( -6.444103211790928043, 202.2591342207265939, 92.19886208192143329 ) ) ;
#255 = ADVANCED_FACE ( 'NONE', ( #21810 ), #32041, .T. ) ;
#256 = CARTESIAN_POINT ( 'NONE',  ( 4.903702542908601636, 200.1653181626581102, 32.45113791807857240 ) ) ;
#257 = CARTESIAN_POINT ( 'NONE',  ( 55.81132485994281467, 159.8737954434936057, -15.00000000000002665 ) ) ;
#258 = VERTEX_POINT ( 'NONE', #32202 ) ;
#259 = CARTESIAN_POINT ( 'NONE',  ( 4.000000000000000000, 3.518949890710768802, -4.770489558936219510E-15 ) ) ;
#260 = CARTESIAN_POINT ( 'NONE',  ( 86.72499999726882436, 140.1801316387863778, -4.815267126137194431 ) ) ;
#261 = FACE_OUTER_BOUND ( 'NONE', #4301, .T. ) ;
#262 = CARTESIAN_POINT ( 'NONE',  ( 7.984503880673485376, 204.3529502787953902, 86.15113791807856103 ) ) ;
#263 = COLOUR_RGB ( '', 0.31764706, 0.68627451, 0.89019608) ;
#264 =( NAMED_UNIT ( * ) PLANE_ANGLE_UNIT ( ) SI_UNIT ( $, .RADIAN. ) );
#265 = CARTESIAN_POINT ( 'NONE',  ( 49.50000000000000000, 155.0000000000000000, 14.49999999999999467 ) ) ;
#266 = CARTESIAN_POINT ( 'NONE',  ( 8.015496119326595448, 204.4483345814782638, 61.14886208192145034 ) ) ;
#267 = CARTESIAN_POINT ( 'NONE',  ( 125.5000000000000000, 229.9533188057749555, 74.95331880577313655 ) ) ;
#268 = CARTESIAN_POINT ( 'NONE',  ( 50.62499999726880162, 138.6155565068815463, -3.929120461958505118E-15 ) ) ;
#269 = CARTESIAN_POINT ( 'NONE',  ( 3.044812012440130555, 197.4746971517856764, -0.3988620819214342972 ) ) ;
#270 = CARTESIAN_POINT ( 'NONE',  ( 61.02499999726880020, 149.9369285172503510, -15.58253175000000823 ) ) ;
#271 = CARTESIAN_POINT ( 'NONE',  ( 72.47499999726878173, 149.9369285172503510, 15.58253174999999580 ) ) ;
#272 = CARTESIAN_POINT ( 'NONE',  ( -7.375838497908182134, 217.2372850707499765, 66.95113791807857240 ) ) ;
#273 = DIRECTION ( 'NONE',  ( 0.000000000000000000, 0.000000000000000000, -1.000000000000000000 ) ) ;
#274 = CARTESIAN_POINT ( 'NONE',  ( -8.062137200540920645, 212.9164362838581894, 87.80113791807856671 ) ) ;
#275 = CARTESIAN_POINT ( 'NONE',  ( 125.5000000000000000, 48.99999999999998579, 2.149999999999971489 ) ) ;
#276 = CARTESIAN_POINT ( 'NONE',  ( -9.680171189290716072, 199.9079932115567146, 50.19886208192144039 ) ) ;
#277 = CARTESIAN_POINT ( 'NONE',  ( 3.044812012439969795, 216.5253028482143520, 57.39886208192143613 ) ) ;
#278 = CARTESIAN_POINT ( 'NONE',  ( -12.01549611932652972, 203.1486557965464499, 93.35113791807857808 ) ) ;
#279 = CARTESIAN_POINT ( 'NONE',  ( -67.50001199999999812, 171.4562830276601630, 4.407803664655115305 ) ) ;
#280 = CARTESIAN_POINT ( 'NONE',  ( -10.00000000000000711, 207.0476921513413515, 12.50113791807856778 ) ) ;
#281 = CARTESIAN_POINT ( 'NONE',  ( -3.044812012439970683, 197.4746971517856196, 76.89886208192143613 ) ) ;
#282 = APPLICATION_CONTEXT ( 'automotive_design' ) ;
#283 = ORIENTED_EDGE ( 'NONE', *, *, #23034, .T. ) ;
#284 = CARTESIAN_POINT ( 'NONE',  ( 8.118202686958039038, 212.8392687619912635, 100.7011379180785866 ) ) ;
#285 = ORIENTED_EDGE ( 'NONE', *, *, #11593, .T. ) ;
#286 = CARTESIAN_POINT ( 'NONE',  ( -0.05014649552828365914, 215.4116977939061144, 66.24886208192143044 ) ) ;
#287 = ORIENTED_EDGE ( 'NONE', *, *, #8864, .T. ) ;
#288 = CARTESIAN_POINT ( 'NONE',  ( 75.92499999726881299, 164.1591823560292198, 12.60653300113718167 ) ) ;
#289 = DIRECTION ( 'NONE',  ( 0.000000000000000000, 0.9988620819214357738, 0.04769215134144196705 ) ) ;
#290 = DIRECTION ( 'NONE',  ( 1.000000000000000000, -0.000000000000000000, -0.000000000000000000 ) ) ;
#291 = CARTESIAN_POINT ( 'NONE',  ( 67.82499999726881867, 168.2552932293087906, 9.630534252274372875 ) ) ;
#292 = CARTESIAN_POINT ( 'NONE',  ( 6.444103211791042618, 202.2591342207267644, 59.30113791807857382 ) ) ;
#293 = CARTESIAN_POINT ( 'NONE',  ( 3.135527875058981895, 197.5041725223112792, 52.59886208192143897 ) ) ;
#294 = CARTESIAN_POINT ( 'NONE',  ( -9.945352646237287431, 205.9548993908332193, 104.4520571433695579 ) ) ;
#295 = DIRECTION ( 'NONE',  ( 1.000000000000000000, 0.000000000000000000, 0.000000000000000000 ) ) ;
#296 = CARTESIAN_POINT ( 'NONE',  ( 2.426778023690075337, 214.6231898156240447, 36.39886208192144323 ) ) ;
#297 = CARTESIAN_POINT ( 'NONE',  ( 9.984503880673470277, 203.7031108863295401, 83.15113791807853261 ) ) ;
#298 = FACE_BOUND ( 'NONE', #1357, .T. ) ;
#299 = EDGE_CURVE ( 'NONE', #17495, #22659, #1461, .T. ) ;
#300 = CARTESIAN_POINT ( 'NONE',  ( 9.984503880673470277, 203.7031108863295401, 56.15113791807856103 ) ) ;
#301 = CARTESIAN_POINT ( 'NONE',  ( 8.118202686958039038, 212.8392687619912635, 25.70113791807856529 ) ) ;
#302 = CARTESIAN_POINT ( 'NONE',  ( 4.984841277089725686, 213.7757310962907411, 13.55113791807856849 ) ) ;
#303 = CARTESIAN_POINT ( 'NONE',  ( 120.4126214611401195, -2.643999646947191362, 35.00001199999999812 ) ) ;
#304 = CARTESIAN_POINT ( 'NONE',  ( 115.4999999999999858, 207.9999999999998010, -91.79869280115066488 ) ) ;
#305 = CARTESIAN_POINT ( 'NONE',  ( 44.22499999726880304, 149.9369285172503510, 15.58253174999999580 ) ) ;
#306 = CARTESIAN_POINT ( 'NONE',  ( 7.375838497908181246, 196.7627149292499666, 35.45113791807855819 ) ) ;
#307 = FACE_BOUND ( 'NONE', #22866, .T. ) ;
#308 = CARTESIAN_POINT ( 'NONE',  ( -6.220909254589537696, 198.5229672870051161, 90.05113791807858092 ) ) ;
#309 = CARTESIAN_POINT ( 'NONE',  ( -10.00000000000000711, 207.0476921513413515, 60.50113791807857666 ) ) ;
#310 = CARTESIAN_POINT ( 'NONE',  ( 12.01549611932659367, 203.1486557965466773, 22.14886208192143613 ) ) ;
#311 = CARTESIAN_POINT ( 'NONE',  ( -0.05014649552828402690, 217.5146222423826714, 24.24886208192143044 ) ) ;
#312 = CARTESIAN_POINT ( 'NONE',  ( 80.39999999453763735, 168.7903194862797420, -4.480746418436745593 ) ) ;
#313 = CARTESIAN_POINT ( 'NONE',  ( 12.00000000000000711, 206.9523078486586485, 71.00113791807856956 ) ) ;
#314 = CARTESIAN_POINT ( 'NONE',  ( 7.984503880673485376, 204.3529502787953902, 92.15113791807856103 ) ) ;
#315 = CARTESIAN_POINT ( 'NONE',  ( -8.118202686958138514, 212.8392687619910930, 53.79886208192143471 ) ) ;
#316 = DIRECTION ( 'NONE',  ( 0.000000000000000000, 0.000000000000000000, -1.000000000000000000 ) ) ;
#317 = VERTEX_POINT ( 'NONE', #1197 ) ;
#318 = CARTESIAN_POINT ( 'NONE',  ( -7.456977232089471386, 217.1783343296987709, 50.94886208192143329 ) ) ;
#319 = ORIENTED_EDGE ( 'NONE', *, *, #6440, .F. ) ;
#320 = VERTEX_POINT ( 'NONE', #8379 ) ;
#321 = CARTESIAN_POINT ( 'NONE',  ( 0.000000000000000000, 0.000000000000000000, 3.299999999999999822 ) ) ;
#322 = DIRECTION ( 'NONE',  ( 0.000000000000000000, -0.5000000000000011102, -0.8660254037844379305 ) ) ;
#323 = CARTESIAN_POINT ( 'NONE',  ( 8.000000000000008882, 206.9523078486586485, 44.00113791807857666 ) ) ;
#324 = EDGE_CURVE ( 'NONE', #6936, #7786, #8863, .T. ) ;
#325 = FILL_AREA_STYLE ('',( #15500 ) ) ;
#326 = CARTESIAN_POINT ( 'NONE',  ( 10.01549611932659545, 203.7984951890123853, 19.14886208192142902 ) ) ;
#327 = CARTESIAN_POINT ( 'NONE',  ( 63.57499999726881867, 164.1591823560292198, -12.60653300113719766 ) ) ;
#328 = ORIENTED_EDGE ( 'NONE', *, *, #21858, .T. ) ;
#329 = DIRECTION ( 'NONE',  ( 0.000000000000000000, 1.000000000000000000, 0.000000000000000000 ) ) ;
#330 = FILL_AREA_STYLE ('',( #26891 ) ) ;
#331 = CARTESIAN_POINT ( 'NONE',  ( -7.922281120364393914, -4.573931137438277617, -8.047472243342932430 ) ) ;
#332 = CARTESIAN_POINT ( 'NONE',  ( 8.015496119326595448, 204.4483345814782638, 10.14886208192143435 ) ) ;
#333 = CARTESIAN_POINT ( 'NONE',  ( -6.220909254589537696, 198.5229672870051161, 48.05113791807858092 ) ) ;
#334 =( NAMED_UNIT ( * ) PLANE_ANGLE_UNIT ( ) SI_UNIT ( $, .RADIAN. ) );
#335 = EDGE_CURVE ( 'NONE', #14777, #31781, #18767, .T. ) ;
#336 = CARTESIAN_POINT ( 'NONE',  ( 10.00000000000000711, 206.9523078486586201, 23.00113791807856600 ) ) ;
#337 = CARTESIAN_POINT ( 'NONE',  ( 84.47499999726881015, 149.9369285172503510, 15.58253174999999580 ) ) ;
#338 = APPLICATION_PROTOCOL_DEFINITION ( 'draft international standard', 'automotive_design', 1998, #916 ) ;
#339 = CARTESIAN_POINT ( 'NONE',  ( 8.015496119326595448, 204.4483345814782638, 88.14886208192143613 ) ) ;
#340 = CARTESIAN_POINT ( 'NONE',  ( 38.12499999726880873, 155.0000000000000000, 15.58253174999999402 ) ) ;
#341 = CARTESIAN_POINT ( 'NONE',  ( -58.50000000000002132, 194.9217985566782829, 2.500000000000000000 ) ) ;
#342 = LINE ( 'NONE', #30862, #5985 ) ;
#343 = CARTESIAN_POINT ( 'NONE',  ( 0.05014649552807549926, 219.6175466908591716, 7.251137918078565114 ) ) ;
#344 = EDGE_CURVE ( 'NONE', #21593, #16276, #11595, .T. ) ;
#345 = DIRECTION ( 'NONE',  ( 0.000000000000000000, 0.000000000000000000, 1.000000000000000000 ) ) ;
#346 = CARTESIAN_POINT ( 'NONE',  ( 58.17499999726881299, 164.1591823560292198, 12.60653300113718167 ) ) ;
#347 = CARTESIAN_POINT ( 'NONE',  ( 6.139770520408368348, 198.4640165459539674, 59.45113791807855819 ) ) ;
#348 = CARTESIAN_POINT ( 'NONE',  ( 8.062137200540920645, 201.0835637161417822, 32.30113791807857382 ) ) ;
#349 = AXIS2_PLACEMENT_3D ( 'NONE', #10435, #20806, #13142 ) ;
#350 = CARTESIAN_POINT ( 'NONE',  ( -7.499999999999999112, -2.930060224340425901, -0.4701183149080249146 ) ) ;
#351 = EDGE_CURVE ( 'NONE', #31779, #31412, #28685, .T. ) ;
#352 = CARTESIAN_POINT ( 'NONE',  ( 78.61132485994281183, 159.8737954434936057, 15.00000000000001421 ) ) ;
#353 = CARTESIAN_POINT ( 'NONE',  ( 10.01549611932659367, 203.7984951890124421, 4.148862081921434353 ) ) ;
#354 = CARTESIAN_POINT ( 'NONE',  ( 62.09999999453761887, 159.7113355953771077, -14.50000000000000888 ) ) ;
#355 = VERTEX_POINT ( 'NONE', #16197 ) ;
#356 = CARTESIAN_POINT ( 'NONE',  ( 7.375838497908181246, 196.7627149292499666, 38.45113791807856529 ) ) ;
#357 = CARTESIAN_POINT ( 'NONE',  ( 77.31132485994280046, 140.7341522555726669, -4.635254915624220651 ) ) ;
#358 = CARTESIAN_POINT ( 'NONE',  ( -10.01549611932659722, 210.2015048109875011, 23.64886208192142902 ) ) ;
#359 = CARTESIAN_POINT ( 'NONE',  ( 71.28867513459483973, 170.7719333635740497, -7.904646289410545231E-15 ) ) ;
#360 = ORIENTED_EDGE ( 'NONE', *, *, #7714, .F. ) ;
#361 = ADVANCED_FACE ( 'NONE', ( #27937 ), #11271, .T. ) ;
#362 = CARTESIAN_POINT ( 'NONE',  ( -6.139770520408369237, 215.5359834540460042, 66.95113791807858661 ) ) ;
#363 = EDGE_LOOP ( 'NONE', ( #22893, #12184, #17028, #24574 ) ) ;
#364 = CARTESIAN_POINT ( 'NONE',  ( 44.11132485994280472, 169.2658477444273331, -4.635254915624224203 ) ) ;
#365 = ORIENTED_EDGE ( 'NONE', *, *, #11822, .F. ) ;
#366 = CARTESIAN_POINT ( 'NONE',  ( -2.517493886308901807, 199.4062855549015012, 17.90113791807856458 ) ) ;
#367 = EDGE_CURVE ( 'NONE', #11826, #6694, #28121, .T. ) ;
#368 = VECTOR ( 'NONE', #30488, 1000.000000000000000 ) ;
#369 = CARTESIAN_POINT ( 'NONE',  ( -12.00000000000000711, 206.9523078486584780, 101.4988620819214304 ) ) ;
#370 = CARTESIAN_POINT ( 'NONE',  ( 45.47499999726881015, 160.0630714827496206, -15.58253175000000823 ) ) ;
#371 = ORIENTED_EDGE ( 'NONE', *, *, #28490, .F. ) ;
#372 = CARTESIAN_POINT ( 'NONE',  ( 51.32499999726881157, 164.1591823560292198, -12.60653300113719766 ) ) ;
#373 = FACE_OUTER_BOUND ( 'NONE', #11507, .T. ) ;
#374 = CARTESIAN_POINT ( 'NONE',  ( -6.139770520408369237, 215.5359834540460042, 9.951137918078567068 ) ) ;
#375 = MECHANICAL_DESIGN_GEOMETRIC_PRESENTATION_REPRESENTATION (  '', ( #3643 ), #27015 ) ;
#376 = CARTESIAN_POINT ( 'NONE',  ( 6.220909254589681581, 198.5229672870052582, 82.44886208192141908 ) ) ;
#377 = CARTESIAN_POINT ( 'NONE',  ( 51.67499999726879878, 168.2552932293087906, -9.630534252274385310 ) ) ;
#378 = CARTESIAN_POINT ( 'NONE',  ( 32.50000000000000000, 155.0000000000000000, 15.00000000000001243 ) ) ;
#379 = CARTESIAN_POINT ( 'NONE',  ( -10.01549611932653860, 203.7984951890123284, 9.351137918078569200 ) ) ;
#380 = DIRECTION ( 'NONE',  ( -1.000000000000000000, 0.000000000000000000, 0.000000000000000000 ) ) ;
#381 = EDGE_CURVE ( 'NONE', #5932, #16641, #20514, .T. ) ;
#382 = CIRCLE ( 'NONE', #1466, 1.033333333332998372 ) ;
#383 = CARTESIAN_POINT ( 'NONE',  ( 75.40000000000000568, 159.7113355953771077, 14.49999999999999289 ) ) ;
#384 = CARTESIAN_POINT ( 'NONE',  ( -6.220909254589537696, 198.5229672870051161, 99.05113791807858092 ) ) ;
#385 = DIRECTION ( 'NONE',  ( -1.000000000000000000, -0.000000000000000000, -0.000000000000000000 ) ) ;
#386 = CARTESIAN_POINT ( 'NONE',  ( -8.118202686958039038, 201.1607312380087080, 81.20113791807857240 ) ) ;
#387 = CARTESIAN_POINT ( 'NONE',  ( 86.48867513459484258, 142.2402378747194405, -9.270509831248439525 ) ) ;
#388 = CARTESIAN_POINT ( 'NONE',  ( 37.37499999726881583, 155.0000000000000000, -15.58253175000000823 ) ) ;
#389 = CARTESIAN_POINT ( 'NONE',  ( -7.456977232089471386, 217.1783343296987709, 92.94886208192144750 ) ) ;
#390 = CARTESIAN_POINT ( 'NONE',  ( 71.72499999726881015, 169.8198683612136222, 4.815267126137181997 ) ) ;
#391 = ORIENTED_EDGE ( 'NONE', *, *, #25603, .F. ) ;
#392 = DIRECTION ( 'NONE',  ( 0.000000000000000000, 0.000000000000000000, 1.000000000000000000 ) ) ;
#393 = CARTESIAN_POINT ( 'NONE',  ( 38.49999999453763166, 170.2462022514548323, -7.872454543227099337E-15 ) ) ;
#394 = VECTOR ( 'NONE', #33049, 1000.000000000000114 ) ;
#395 = EDGE_CURVE ( 'NONE', #7505, #355, #22318, .T. ) ;
#396 = CARTESIAN_POINT ( 'NONE',  ( 60.63708498984762940, 120.3589838486224579, -20.00000000000000000 ) ) ;
#397 = CIRCLE ( 'NONE', #9630, 3.499999999999999556 ) ;
#398 = ORIENTED_EDGE ( 'NONE', *, *, #15560, .F. ) ;
#399 = PRESENTATION_LAYER_ASSIGNMENT (  '', '', ( #30884 ) ) ;
#400 = CARTESIAN_POINT ( 'NONE',  ( -8.062137200540822946, 201.0835637161416400, 95.19886208192143329 ) ) ;
#401 = CARTESIAN_POINT ( 'NONE',  ( -3.753561863808878130, 218.3979405102790281, 33.09886208192143187 ) ) ;
#402 = CARTESIAN_POINT ( 'NONE',  ( -52.50000000000002132, 155.0000000000000000, 6.938893903907228378E-15 ) ) ;
#403 = CARTESIAN_POINT ( 'NONE',  ( -8.118202686958039038, 201.1607312380087080, 39.20113791807857240 ) ) ;
#404 = ORIENTED_EDGE ( 'NONE', *, *, #3314, .F. ) ;
#405 = EDGE_CURVE ( 'NONE', #7596, #17895, #14227, .T. ) ;
#406 = CARTESIAN_POINT ( 'NONE',  ( 4.984841277089891776, 200.2242689037093726, 1.448862081921434841 ) ) ;
#407 = AXIS2_PLACEMENT_3D ( 'NONE', #13866, #6364, #3304 ) ;
#408 = DIRECTION ( 'NONE',  ( 0.000000000000000000, 0.000000000000000000, 1.000000000000000000 ) ) ;
#409 = EDGE_LOOP ( 'NONE', ( #12808, #6354, #120, #4248 ) ) ;
#410 = CARTESIAN_POINT ( 'NONE',  ( -2.517493886309087880, 214.5937144450984135, 90.09886208192143897 ) ) ;
#411 = ADVANCED_FACE ( 'NONE', ( #12099 ), #20103, .F. ) ;
#412 = CARTESIAN_POINT ( 'NONE',  ( -8.000000000000008882, 207.0476921513413515, 27.50113791807856956 ) ) ;
#413 = FACE_OUTER_BOUND ( 'NONE', #6804, .T. ) ;
#414 = ORIENTED_EDGE ( 'NONE', *, *, #20724, .T. ) ;
#415 = CARTESIAN_POINT ( 'NONE',  ( 34.42499999726880588, 141.7447067706911810, 9.630534252274376428 ) ) ;
#416 = CIRCLE ( 'NONE', #9651, 5.000000000000000888 ) ;
#417 = CARTESIAN_POINT ( 'NONE',  ( 33.67499999726881299, 168.2552932293087906, -9.630534252274385310 ) ) ;
#418 = PLANE ( 'NONE',  #220 ) ;
#419 = CARTESIAN_POINT ( 'NONE',  ( 7.984503880673485376, 204.3529502787953902, 89.15113791807856103 ) ) ;
#420 = VECTOR ( 'NONE', #14402, 1000.000000000000000 ) ;
#421 = CONICAL_SURFACE ( 'NONE', #2627, 6.500000000000000888, 0.8987552595851582282 ) ;
#422 = CARTESIAN_POINT ( 'NONE',  ( 45.70000000000000284, 146.4771138417591203, 11.73074641843673227 ) ) ;
#423 = CARTESIAN_POINT ( 'NONE',  ( -8.015496119326597224, 209.5516654185217362, 77.64886208192143613 ) ) ;
#424 = DIRECTION ( 'NONE',  ( 0.000000000000000000, 0.000000000000000000, -1.000000000000000000 ) ) ;
#425 = VECTOR ( 'NONE', #6795, 1000.000000000000227 ) ;
#426 = CARTESIAN_POINT ( 'NONE',  ( 51.12499999726881583, 155.0000000000000000, -15.58253175000000823 ) ) ;
#428 = ORIENTED_EDGE ( 'NONE', *, *, #4153, .F. ) ;
#427 = CARTESIAN_POINT ( 'NONE',  ( -9.984503880673475606, 210.2968891136704315, 15.65113791807856636 ) ) ;
#429 = DIRECTION ( 'NONE',  ( -1.000000000000000000, 0.000000000000000000, 0.000000000000000000 ) ) ;
#430 = CARTESIAN_POINT ( 'NONE',  ( 66.72499999726881015, 140.1801316387863778, -4.815267126137194431 ) ) ;
#431 = CARTESIAN_POINT ( 'NONE',  ( 78.67499999726879878, 141.7447067706911810, 9.630534252274376428 ) ) ;
#432 = CARTESIAN_POINT ( 'NONE',  ( 12.01549611932652972, 210.8513442034534933, 76.85113791807856387 ) ) ;
#433 = CARTESIAN_POINT ( 'NONE',  ( -6.500000000000000000, -3.752776749732572803, -6.177802698399433190 ) ) ;
#434 = EDGE_CURVE ( 'NONE', #32282, #27762, #17038, .T. ) ;
#435 = ADVANCED_FACE ( 'NONE', ( #11935 ), #14477, .T. ) ;
#436 = CARTESIAN_POINT ( 'NONE',  ( 10.01549611932653860, 210.2015048109876716, 97.85113791807857808 ) ) ;
#437 = CARTESIAN_POINT ( 'NONE',  ( 58.50000000000001421, -88.00000000000000000, -30.00000000000000000 ) ) ;
#438 = ORIENTED_EDGE ( 'NONE', *, *, #191, .T. ) ;
#439 = CARTESIAN_POINT ( 'NONE',  ( 7.375838497908012492, 217.2372850707501186, 51.54886208192144181 ) ) ;
#440 = CARTESIAN_POINT ( 'NONE',  ( 6.139770520408223575, 215.5359834540460611, 69.54886208192142760 ) ) ;
#441 = CARTESIAN_POINT ( 'NONE',  ( -3.753561863808878130, 218.3979405102790281, 6.098862081921433642 ) ) ;
#442 = CARTESIAN_POINT ( 'NONE',  ( -5.000000000000000888, 6.123233995736767268E-16, -25.03750572909317285 ) ) ;
#443 = AXIS2_PLACEMENT_3D ( 'NONE', #26403, #3062, #13451 ) ;
#444 = CARTESIAN_POINT ( 'NONE',  ( 3.135527875058820690, 216.4958274776887492, 10.40113791807856636 ) ) ;
#445 = ADVANCED_FACE ( 'NONE', ( #32704 ), #17380, .F. ) ;
#446 = ADVANCED_FACE ( 'NONE', ( #17719 ), #1879, .F. ) ;
#447 = CARTESIAN_POINT ( 'NONE',  ( -3.044812012439970683, 197.4746971517856196, 79.89886208192143613 ) ) ;
#448 = VECTOR ( 'NONE', #1366, 1000.000000000000000 ) ;
#449 = EDGE_LOOP ( 'NONE', ( #2882, #4117, #25704, #19508 ) ) ;
#450 = CARTESIAN_POINT ( 'NONE',  ( -6.139770520408369237, 215.5359834540460042, 99.95113791807855819 ) ) ;
#451 = ORIENTED_EDGE ( 'NONE', *, *, #3089, .T. ) ;
#452 = SURFACE_SIDE_STYLE ('',( #29228 ) ) ;
#453 = CARTESIAN_POINT ( 'NONE',  ( 6.444103211790928043, 211.7408657792734061, 60.69886208192144750 ) ) ;
#454 = ORIENTED_EDGE ( 'NONE', *, *, #17916, .T. ) ;
#455 =( BOUNDED_CURVE ( )  B_SPLINE_CURVE ( 2, ( #7550, #25926, #18262, #23205, #4981, #21145, #13149, #539, #28652, #5312, #17936 ),
 .UNSPECIFIED., .F., .F. ) 
 B_SPLINE_CURVE_WITH_KNOTS ( ( 3, 2, 2, 2, 2, 3 ),
 ( 0.1249999999999998473, 0.1285714285714284200, 0.1321428571428569787, 0.1357142857142855652, 0.1392857142857141239, 0.1428571428571427104 ),
 .UNSPECIFIED. ) 
 CURVE ( )  GEOMETRIC_REPRESENTATION_ITEM ( )  RATIONAL_B_SPLINE_CURVE ( ( 1.000000000000002220, 0.9510565162951514218, 1.000000000000000000, 0.9510565162951534202, 1.000000000000000000, 0.9510565162951534202, 1.000000000000000000, 0.9510565162951534202, 1.000000000000000000, 0.9510565162951545304, 0.9999999999999988898 ) ) 
 REPRESENTATION_ITEM ( '' )  );
#456 = VECTOR ( 'NONE', #17521, 1000.000000000000227 ) ;
#457 = CARTESIAN_POINT ( 'NONE',  ( 80.42499999726881299, 141.7447067706911810, 9.630534252274376428 ) ) ;
#458 = DIRECTION ( 'NONE',  ( 0.000000000000000000, 0.000000000000000000, 1.000000000000000000 ) ) ;
#459 = DIRECTION ( 'NONE',  ( 0.000000000000000000, -0.000000000000000000, 1.000000000000000000 ) ) ;
#460 = CARTESIAN_POINT ( 'NONE',  ( 69.02499999726880731, 149.9369285172503510, -15.58253175000000823 ) ) ;
#461 = CARTESIAN_POINT ( 'NONE',  ( 8.015496119326531499, 209.5516654185219636, 58.85113791807857098 ) ) ;
#462 = SURFACE_STYLE_USAGE ( .BOTH. , #25511 ) ;
#463 = CYLINDRICAL_SURFACE ( 'NONE', #17578, 15.00000000000001776 ) ;
#464 = SHAPE_REPRESENTATION_RELATIONSHIP ( 'NONE' , 'NONE' ,  #22175, #21775 ) ;
#465 = DIRECTION ( 'NONE',  ( 0.000000000000000000, 0.000000000000000000, -1.000000000000000000 ) ) ;
#466 = CARTESIAN_POINT ( 'NONE',  ( 7.984503880673422316, 209.6470497212048372, 36.84886208192142476 ) ) ;
#467 = AXIS2_PLACEMENT_3D ( 'NONE', #16628, #11526, #21908 ) ;
#468 = CARTESIAN_POINT ( 'NONE',  ( -10.00000000000000711, 207.0476921513413515, 84.50113791807856956 ) ) ;
#469 = DIRECTION ( 'NONE',  ( 0.000000000000000000, 0.000000000000000000, -1.000000000000000000 ) ) ;
#470 = CARTESIAN_POINT ( 'NONE',  ( 8.118202686958039038, 212.8392687619912635, 70.70113791807857240 ) ) ;
#471 = CIRCLE ( 'NONE', #10841, 12.10452846326762177 ) ;
#472 = CARTESIAN_POINT ( 'NONE',  ( -67.50000000000000000, 122.1366465496900418, -17.00000000000001421 ) ) ;
#473 = CARTESIAN_POINT ( 'NONE',  ( -2.426778023690262742, 214.6231898156240163, 19.10113791807856742 ) ) ;
#474 = CARTESIAN_POINT ( 'NONE',  ( 122.3560003530528064, -4.587378538859826271, 35.00001200000000523 ) ) ;
#475 = CARTESIAN_POINT ( 'NONE',  ( 60.48867513459483547, 142.2402378747194405, -9.270509831248439525 ) ) ;
#476 = CARTESIAN_POINT ( 'NONE',  ( 42.52499999726880731, 140.1801316387863778, 4.815267126137185549 ) ) ;
#477 = CARTESIAN_POINT ( 'NONE',  ( -12.01549611932652972, 203.1486557965464499, 39.35113791807856387 ) ) ;
#478 = CARTESIAN_POINT ( 'NONE',  ( 7.908217798048221781, 3.084840533507044125, -7.795645399445156443 ) ) ;
#479 = CARTESIAN_POINT ( 'NONE',  ( 3.044812012440130555, 197.4746971517856764, 98.60113791807857808 ) ) ;
#480 = CARTESIAN_POINT ( 'NONE',  ( 10.01549611932653860, 210.2015048109876716, 61.85113791807857098 ) ) ;
#481 = VECTOR ( 'NONE', #17231, 1000.000000000000000 ) ;
#482 = CARTESIAN_POINT ( 'NONE',  ( 9.736236675708031640, 199.9851607334238963, 22.29886208192143826 ) ) ;
#483 = CARTESIAN_POINT ( 'NONE',  ( 10.00000000000000711, 207.0476921513415220, 36.99886208192143755 ) ) ;
#484 = CARTESIAN_POINT ( 'NONE',  ( 79.79999999453762882, 146.4771138417591203, -11.73074641843674470 ) ) ;
#485 = CARTESIAN_POINT ( 'NONE',  ( -11.98450388067348804, 210.9467285061362247, 69.65113791807856103 ) ) ;
#486 = CARTESIAN_POINT ( 'NONE',  ( 8.015496119326531499, 209.5516654185219636, 85.85113791807857808 ) ) ;
#487 = CARTESIAN_POINT ( 'NONE',  ( 6.139770520408223575, 215.5359834540460611, 48.54886208192143471 ) ) ;
#488 = CARTESIAN_POINT ( 'NONE',  ( -52.50000000000002132, 155.0000000000000000, 6.938893903907228378E-15 ) ) ;
#489 = ORIENTED_EDGE ( 'NONE', *, *, #23335, .T. ) ;
#490 = CARTESIAN_POINT ( 'NONE',  ( -3.662846001189865142, 195.5725841191952838, 52.89886208192143613 ) ) ;
#491 = ORIENTED_EDGE ( 'NONE', *, *, #10155, .T. ) ;
#492 = CONICAL_SURFACE ( 'NONE', #30975, 15.50000000000001066, 0.3490658503988691153 ) ;
#493 = ORIENTED_EDGE ( 'NONE', *, *, #9737, .T. ) ;
#494 = CARTESIAN_POINT ( 'NONE',  ( 77.47499999726879594, 160.0630714827496206, -15.58253175000000823 ) ) ;
#495 = CARTESIAN_POINT ( 'NONE',  ( -3.755786496842903988E-16, -7.505553499465146494, -8.000000000000000000 ) ) ;
#496 = VECTOR ( 'NONE', #27599, 1000.000000000000000 ) ;
#497 = CARTESIAN_POINT ( 'NONE',  ( 11.98450388067341876, 210.9467285061363953, 54.84886208192143187 ) ) ;
#498 = CARTESIAN_POINT ( 'NONE',  ( -105.0000000000000142, 2.449293598294705330E-15, 35.00200000000000244 ) ) ;
#499 = CARTESIAN_POINT ( 'NONE',  ( 6.500168698208129925, 211.6636982574063381, 37.70113791807857240 ) ) ;
#500 = FILL_AREA_STYLE_COLOUR ( '', #2004 ) ;
#501 = CARTESIAN_POINT ( 'NONE',  ( -3.044812012439970683, 197.4746971517856196, 22.89886208192143613 ) ) ;
#502 = CARTESIAN_POINT ( 'NONE',  ( 63.27499999726880731, 149.9369285172503510, -15.58253175000000823 ) ) ;
#504 = ORIENTED_EDGE ( 'NONE', *, *, #9364, .F. ) ;
#503 = AXIS2_PLACEMENT_3D ( 'NONE', #32929, #27646, #1421 ) ;
#505 = UNCERTAINTY_MEASURE_WITH_UNIT (LENGTH_MEASURE( 1.000000000000000082E-05 ), #16997, 'distance_accuracy_value', 'NONE');
#506 =( LENGTH_UNIT ( ) NAMED_UNIT ( * ) SI_UNIT ( .MILLI., .METRE. ) );
#507 =( BOUNDED_CURVE ( )  B_SPLINE_CURVE ( 2, ( #4951, #13282, #18065, #5118, #18402, #10250, #10735, #28626, #5613 ),
 .UNSPECIFIED., .F., .T. ) 
 B_SPLINE_CURVE_WITH_KNOTS ( ( 3, 2, 2, 2, 3 ),
 ( 0.9464285714285716189, 0.9500000000000000666, 0.9535714285714287364, 0.9571428571428571841, 0.9605034456745119575 ),
 .UNSPECIFIED. ) 
 CURVE ( )  GEOMETRIC_REPRESENTATION_ITEM ( )  RATIONAL_B_SPLINE_CURVE ( ( 0.9999999999999970024, 0.9510565162951564178, 1.000000000000000000, 0.9510565162951534202, 1.000000000000000000, 0.9510565162951534202, 1.000000000000000000, 0.9539459051894326747, 0.9945623735783009067 ) ) 
 REPRESENTATION_ITEM ( '' )  );
#508 = CARTESIAN_POINT ( 'NONE',  ( -63.50000000000004263, 215.0000000000000000, 0.000000000000000000 ) ) ;
#509 = CARTESIAN_POINT ( 'NONE',  ( -4.984841277089891776, 213.7757310962905990, 2.948862081921435063 ) ) ;
#510 = CARTESIAN_POINT ( 'NONE',  ( -9.984503880673473830, 210.2968891136704315, 54.65113791807858235 ) ) ;
#511 = CARTESIAN_POINT ( 'NONE',  ( 5.276765049035074817, -6.073111908730307817, -7.634085501268428331 ) ) ;
#512 = CARTESIAN_POINT ( 'NONE',  ( 0.05014649552810505201, 217.5146222423826714, 34.25113791807856956 ) ) ;
#513 = CARTESIAN_POINT ( 'NONE',  ( 83.97499999726882436, 169.8198683612136222, 4.815267126137181997 ) ) ;
#514 = PRODUCT_CONTEXT ( 'NONE', #30526, 'mechanical' ) ;
#515 = CARTESIAN_POINT ( 'NONE',  ( -8.015496119326597224, 209.5516654185217362, 95.64886208192143613 ) ) ;
#516 = CARTESIAN_POINT ( 'NONE',  ( 41.42499999726881299, 168.2552932293087906, -9.630534252274385310 ) ) ;
#517 = DIRECTION ( 'NONE',  ( -0.000000000000000000, -0.000000000000000000, -1.000000000000000000 ) ) ;
#518 = CYLINDRICAL_SURFACE ( 'NONE', #15739, 17.00000000000000355 ) ;
#519 = CARTESIAN_POINT ( 'NONE',  ( 9.680171189290831535, 199.9079932115568852, 11.30113791807856671 ) ) ;
#520 = AXIS2_PLACEMENT_3D ( 'NONE', #21332, #31728, #8401 ) ;
#521 = CARTESIAN_POINT ( 'NONE',  ( -1.860380241283027480, -6.431462466365327479, -0.1499059597315341996 ) ) ;
#522 = CARTESIAN_POINT ( 'NONE',  ( 57.07499999726879736, 141.7447067706911810, -9.630534252274385310 ) ) ;
#523 = CARTESIAN_POINT ( 'NONE',  ( -6.220909254589537696, 198.5229672870051161, 54.05113791807856671 ) ) ;
#524 = CARTESIAN_POINT ( 'NONE',  ( -8.118202686958039038, 201.1607312380087080, 27.20113791807856884 ) ) ;
#525 = CARTESIAN_POINT ( 'NONE',  ( 4.000000000000000000, 1.759474945355380404, -3.047500000000001652 ) ) ;
#526 = CARTESIAN_POINT ( 'NONE',  ( 55.78867513459481842, 155.0000000000000000, 15.00000000000001243 ) ) ;
#527 = DIRECTION ( 'NONE',  ( 0.000000000000000000, -1.000000000000000000, 0.000000000000000000 ) ) ;
#528 = CARTESIAN_POINT ( 'NONE',  ( 60.59999999453763309, 168.7903194862797420, 4.480746418436729606 ) ) ;
#529 = ORIENTED_EDGE ( 'NONE', *, *, #7683, .F. ) ;
#530 = CARTESIAN_POINT ( 'NONE',  ( -7.375838497908182134, 217.2372850707499765, 36.95113791807856529 ) ) ;
#531 = DIRECTION ( 'NONE',  ( 0.8191520442889917986, 1.003171929053524747E-16, -0.5735764363510460484 ) ) ;
#532 = CARTESIAN_POINT ( 'NONE',  ( 0.05014649552828275708, 196.4853777576173002, 25.74886208192143400 ) ) ;
#533 = CARTESIAN_POINT ( 'NONE',  ( 71.58867513459482268, 163.8167787843871110, 12.13525491562421621 ) ) ;
#534 = VERTEX_POINT ( 'NONE', #12264 ) ;
#535 = CARTESIAN_POINT ( 'NONE',  ( 3.135527875058820690, 216.4958274776887492, 82.40113791807857524 ) ) ;
#536 = VERTEX_POINT ( 'NONE', #28106 ) ;
#537 = EDGE_CURVE ( 'NONE', #27429, #2840, #9457, .T. ) ;
#538 = CARTESIAN_POINT ( 'NONE',  ( 125.5000000000000000, 229.9533188057739039, -74.95331880577418815 ) ) ;
#539 = CARTESIAN_POINT ( 'NONE',  ( 80.08867513459485110, 142.2402378747194405, 9.270509831248432420 ) ) ;
#540 = ORIENTED_EDGE ( 'NONE', *, *, #17503, .F. ) ;
#541 = CARTESIAN_POINT ( 'NONE',  ( -6.444103211791042618, 211.7408657792732356, 9.801137918078564937 ) ) ;
#542 = AXIS2_PLACEMENT_3D ( 'NONE', #1520, #30308, #26911 ) ;
#543 = DIRECTION ( 'NONE',  ( -1.000000000000000000, 0.000000000000000000, 0.000000000000000000 ) ) ;
#544 = CARTESIAN_POINT ( 'NONE',  ( -9.680171189290716072, 199.9079932115567146, 98.19886208192144750 ) ) ;
#545 = CARTESIAN_POINT ( 'NONE',  ( 45.07499999726879736, 141.7447067706911810, -9.630534252274387086 ) ) ;
#546 = VERTEX_POINT ( 'NONE', #19601 ) ;
#547 = CARTESIAN_POINT ( 'NONE',  ( 48.62499999726880873, 138.6155565068815463, -3.929120461958505118E-15 ) ) ;
#548 = CARTESIAN_POINT ( 'NONE',  ( -58.50000000000001421, -88.00000000000000000, 20.00000000000000000 ) ) ;
#549 = CARTESIAN_POINT ( 'NONE',  ( 61.68867513459483121, 159.8737954434936057, 15.00000000000001421 ) ) ;
#550 = CARTESIAN_POINT ( 'NONE',  ( 6.139770520408223575, 215.5359834540460611, 81.54886208192144181 ) ) ;
#551 = CARTESIAN_POINT ( 'NONE',  ( 56.27499999726880020, 160.0630714827496206, 15.58253174999999402 ) ) ;
#552 = CARTESIAN_POINT ( 'NONE',  ( -8.118202686958039038, 201.1607312380087080, 18.20113791807856884 ) ) ;
#553 = CARTESIAN_POINT ( 'NONE',  ( -65.24999999999998579, -6.704941225331758039E-15, -20.00000000000000355 ) ) ;
#554 = CARTESIAN_POINT ( 'NONE',  ( 74.30000000000001137, 146.4771138417591203, -11.73074641843674470 ) ) ;
#555 = LINE ( 'NONE', #10948, #13247 ) ;
#556 = CARTESIAN_POINT ( 'NONE',  ( 127.5000000000000000, 155.0000000000000000, -6.938893903907228378E-15 ) ) ;
#557 = CARTESIAN_POINT ( 'NONE',  ( -6.220909254589537696, 198.5229672870051161, 87.05113791807856671 ) ) ;
#558 = CARTESIAN_POINT ( 'NONE',  ( 33.28867513459482552, 170.7719333635740497, -7.904646289410545231E-15 ) ) ;
#559 = CARTESIAN_POINT ( 'NONE',  ( 36.17499999726880588, 164.1591823560292198, 12.60653300113718167 ) ) ;
#560 = CARTESIAN_POINT ( 'NONE',  ( -9.736236675708031640, 214.0148392665760753, 95.79886208192144181 ) ) ;
#561 = CARTESIAN_POINT ( 'NONE',  ( 75.12499999726881583, 155.0000000000000000, -15.58253175000000823 ) ) ;
#562 = VERTEX_POINT ( 'NONE', #4088 ) ;
#563 = CARTESIAN_POINT ( 'NONE',  ( 102.4138169258850581, 155.0000000000000000, 0.000000000000000000 ) ) ;
#564 = CARTESIAN_POINT ( 'NONE',  ( 42.69999999453762030, 167.3344367211045096, 8.961492836873468093 ) ) ;
#565 = CARTESIAN_POINT ( 'NONE',  ( 39.81132485994280756, 159.8737954434936057, -15.00000000000005151 ) ) ;
#566 = CARTESIAN_POINT ( 'NONE',  ( -2.411464220262952818, -7.267994521134228059, -7.491772860715828486 ) ) ;
#567 = ORIENTED_EDGE ( 'NONE', *, *, #11593, .F. ) ;
#568 = CARTESIAN_POINT ( 'NONE',  ( -8.062137200540822946, 201.0835637161416400, 92.19886208192143329 ) ) ;
#569 = CARTESIAN_POINT ( 'NONE',  ( -7.375838497908014268, 196.7627149292498530, 35.04886208192143471 ) ) ;
#570 = FACE_OUTER_BOUND ( 'NONE', #15244, .T. ) ;
#571 = CARTESIAN_POINT ( 'NONE',  ( 3.044812012440130555, 197.4746971517856764, 56.60113791807857098 ) ) ;
#572 = ORIENTED_EDGE ( 'NONE', *, *, #18867, .F. ) ;
#573 = CARTESIAN_POINT ( 'NONE',  ( 8.015496119326595448, 204.4483345814782638, 7.148862081921435241 ) ) ;
#574 = EDGE_CURVE ( 'NONE', #21522, #10366, #23665, .T. ) ;
#575 = CARTESIAN_POINT ( 'NONE',  ( 73.78867513459483973, 155.0000000000000000, 15.00000000000001243 ) ) ;
#576 = VERTEX_POINT ( 'NONE', #31507 ) ;
#577 = CARTESIAN_POINT ( 'NONE',  ( -4.903702542908436435, 200.1653181626580249, 95.04886208192144181 ) ) ;
#578 = CARTESIAN_POINT ( 'NONE',  ( -4.984841277089726574, 200.2242689037092305, 33.05113791807857382 ) ) ;
#579 = DIRECTION ( 'NONE',  ( 1.000000000000000000, 1.776356839400250465E-15, 0.000000000000000000 ) ) ;
#580 = ORIENTED_EDGE ( 'NONE', *, *, #33085, .F. ) ;
#581 = FACE_OUTER_BOUND ( 'NONE', #26390, .T. ) ;
#582 = ADVANCED_FACE ( 'NONE', ( #13110, #10068 ), #33561, .T. ) ;
#583 = CARTESIAN_POINT ( 'NONE',  ( 87.12499999726880162, 155.0000000000000000, -15.58253175000000823 ) ) ;
#584 = DIRECTION ( 'NONE',  ( -1.000000000000000000, 0.000000000000000000, 0.000000000000000000 ) ) ;
#585 = CARTESIAN_POINT ( 'NONE',  ( -4.984841277089726574, 200.2242689037092305, 96.05113791807858092 ) ) ;
#586 = CARTESIAN_POINT ( 'NONE',  ( 0.000000000000000000, 0.000000000000000000, 0.000000000000000000 ) ) ;
#587 = CARTESIAN_POINT ( 'NONE',  ( 55.79999999999999716, 142.6655632788954620, 8.961492836873471646 ) ) ;
#588 = CARTESIAN_POINT ( 'NONE',  ( 7.984503880673422316, 209.6470497212048372, 69.84886208192143897 ) ) ;
#589 = DIRECTION ( 'NONE',  ( 1.000000000000000000, 0.000000000000000000, 0.000000000000000000 ) ) ;
#590 = EDGE_CURVE ( 'NONE', #31987, #31739, #18056, .T. ) ;
#591 = CARTESIAN_POINT ( 'NONE',  ( 60.22499999726881725, 149.9369285172503510, 15.58253174999999580 ) ) ;
#592 = CARTESIAN_POINT ( 'NONE',  ( 10.01549611932653860, 210.2015048109876716, 10.85113791807856565 ) ) ;
#593 = CARTESIAN_POINT ( 'NONE',  ( -6.500000000000000888, -4.077972562205394169, -6.122137109124704324 ) ) ;
#594 = CARTESIAN_POINT ( 'NONE',  ( 61.92499999726882010, 164.1591823560292198, 12.60653300113718167 ) ) ;
#595 = CARTESIAN_POINT ( 'NONE',  ( 73.97499999726881015, 169.8198683612136222, 4.815267126137181997 ) ) ;
#596 = CARTESIAN_POINT ( 'NONE',  ( 0.05014649552807549926, 219.6175466908591716, 73.25113791807858377 ) ) ;
#597 = CARTESIAN_POINT ( 'NONE',  ( 32.50000000000000000, 155.0000000000000000, -6.938893903907228378E-15 ) ) ;
#598 = EDGE_CURVE ( 'NONE', #2264, #27762, #4180, .T. ) ;
#599 = CARTESIAN_POINT ( 'NONE',  ( 3.044812012440130555, 197.4746971517856764, 98.60113791807857808 ) ) ;
#600 = CARTESIAN_POINT ( 'NONE',  ( 115.4999999999999858, 155.0000000000000000, -6.938893903907228378E-15 ) ) ;
#601 = ORIENTED_EDGE ( 'NONE', *, *, #25333, .F. ) ;
#602 = CARTESIAN_POINT ( 'NONE',  ( -12.01549611932659722, 210.8513442034533227, 62.64886208192143613 ) ) ;
#603 = CARTESIAN_POINT ( 'NONE',  ( -9.984503880673420539, 203.7031108863293980, 71.34886208192141055 ) ) ;
#604 = CARTESIAN_POINT ( 'NONE',  ( -12.00000000000000711, 206.9523078486584780, 8.498862081921435774 ) ) ;
#605 = DIRECTION ( 'NONE',  ( -0.000000000000000000, -0.000000000000000000, 1.000000000000000000 ) ) ;
#606 = CARTESIAN_POINT ( 'NONE',  ( -3.135527875058821579, 197.5041725223112223, 14.90113791807856636 ) ) ;
#607 = CARTESIAN_POINT ( 'NONE',  ( -6.220909254589682469, 215.4770327129946850, 77.94886208192140487 ) ) ;
#608 = VERTEX_POINT ( 'NONE', #7674 ) ;
#609 = CARTESIAN_POINT ( 'NONE',  ( 3.044812012440130555, 197.4746971517856764, 101.6011379180785781 ) ) ;
#610 = VERTEX_POINT ( 'NONE', #8008 ) ;
#611 = FACE_OUTER_BOUND ( 'NONE', #24311, .T. ) ;
#612 = CARTESIAN_POINT ( 'NONE',  ( -2.517493886309087880, 214.5937144450984135, 60.09886208192145318 ) ) ;
#613 = VERTEX_POINT ( 'NONE', #8175 ) ;
#614 = CARTESIAN_POINT ( 'NONE',  ( 79.42499999726881299, 168.2552932293087906, -9.630534252274387086 ) ) ;
#615 = VERTEX_POINT ( 'NONE', #21107 ) ;
#616 = CARTESIAN_POINT ( 'NONE',  ( 69.78867513459482552, 155.0000000000000000, 15.00000000000001243 ) ) ;
#617 = FACE_OUTER_BOUND ( 'NONE', #6434, .T. ) ;
#618 = AXIS2_PLACEMENT_3D ( 'NONE', #25395, #27609, #7178 ) ;
#619 = MANIFOLD_SOLID_BREP ( 'Boss-Extrude3', #29190 ) ;
#620 = CARTESIAN_POINT ( 'NONE',  ( 71.82499999726883289, 168.2552932293087906, 9.630534252274372875 ) ) ;
#621 = CARTESIAN_POINT ( 'NONE',  ( -2.517493886308901807, 199.4062855549015012, 62.90113791807858945 ) ) ;
#622 = EDGE_CURVE ( 'NONE', #30802, #33225, #4723, .T. ) ;
#623 = CARTESIAN_POINT ( 'NONE',  ( -125.0000000000000000, 0.000000000000000000, 20.00000000000000000 ) ) ;
#624 = EDGE_CURVE ( 'NONE', #17270, #23382, #19967, .T. ) ;
#625 = DIRECTION ( 'NONE',  ( 0.000000000000000000, 0.000000000000000000, -1.000000000000000000 ) ) ;
#626 = CARTESIAN_POINT ( 'NONE',  ( 34.20000000000000284, 142.6655632788954620, -8.961492836873480528 ) ) ;
#627 = CARTESIAN_POINT ( 'NONE',  ( 7.984503880673422316, 209.6470497212048372, 45.84886208192143897 ) ) ;
#628 = CARTESIAN_POINT ( 'NONE',  ( -10.01549611932653860, 203.7984951890123284, 78.35113791807857808 ) ) ;
#629 = EDGE_CURVE ( 'NONE', #11212, #17245, #20101, .T. ) ;
#630 = CARTESIAN_POINT ( 'NONE',  ( -8.118202686958039038, 201.1607312380087080, 63.20113791807857240 ) ) ;
#631 = CARTESIAN_POINT ( 'NONE',  ( 100.2066581602377653, 155.0000000000000000, -13.00000000000001066 ) ) ;
#632 = CARTESIAN_POINT ( 'NONE',  ( 2.517493886308900919, 214.5937144450984420, 25.40113791807857169 ) ) ;
#633 = CARTESIAN_POINT ( 'NONE',  ( -6.781345014477444977, 3.590342129888853151, -6.122077150241850951 ) ) ;
#634 = CARTESIAN_POINT ( 'NONE',  ( 45.42499999726880588, 168.2552932293087906, -9.630534252274387086 ) ) ;
#635 = CARTESIAN_POINT ( 'NONE',  ( -11.98450388067348804, 210.9467285061362247, 45.65113791807856813 ) ) ;
#636 = CARTESIAN_POINT ( 'NONE',  ( 127.5000000000000000, 155.0000000000000000, -112.0000000000000711 ) ) ;
#637 = EDGE_CURVE ( 'NONE', #6050, #31294, #20445, .T. ) ;
#638 = CARTESIAN_POINT ( 'NONE',  ( 3.044812012440130555, 197.4746971517856764, 95.60113791807857808 ) ) ;
#639 = CARTESIAN_POINT ( 'NONE',  ( 10.01549611932653860, 210.2015048109876716, 67.85113791807857808 ) ) ;
#640 = CARTESIAN_POINT ( 'NONE',  ( -9.736236675708031640, 214.0148392665760753, 35.79886208192143471 ) ) ;
#641 = CARTESIAN_POINT ( 'NONE',  ( 10.00000000000000711, 207.0476921513415220, 39.99886208192143755 ) ) ;
#642 = AXIS2_PLACEMENT_3D ( 'NONE', #23360, #10744, #31522 ) ;
#643 = CARTESIAN_POINT ( 'NONE',  ( 79.89999999453763735, 150.2886644046228639, -14.50000000000000888 ) ) ;
#644 = CARTESIAN_POINT ( 'NONE',  ( -3.662846001190052991, 218.4274158808045740, 79.10113791807857808 ) ) ;
#645 = CARTESIAN_POINT ( 'NONE',  ( -8.015496119326531499, 204.4483345814780364, 84.35113791807857808 ) ) ;
#646 =( BOUNDED_CURVE ( )  B_SPLINE_CURVE ( 3, ( #7649, #10206, #20750, #10043 ),
 .UNSPECIFIED., .F., .T. ) 
 B_SPLINE_CURVE_WITH_KNOTS ( ( 4, 4 ),
 ( 0.000000000000000000, 0.5248789335016748048 ),
 .UNSPECIFIED. ) 
 CURVE ( )  GEOMETRIC_REPRESENTATION_ITEM ( )  RATIONAL_B_SPLINE_CURVE ( ( 1.000000000000000000, 0.9771733092046011038, 0.9771733092046011038, 1.000000000000000000 ) ) 
 REPRESENTATION_ITEM ( '' )  );
#647 = CARTESIAN_POINT ( 'NONE',  ( 0.05014649552828275708, 196.4853777576173002, 46.74886208192143755 ) ) ;
#648 = DIRECTION ( 'NONE',  ( 0.000000000000000000, -0.4999999999999990563, 0.8660254037844391517 ) ) ;
#649 = ORIENTED_EDGE ( 'NONE', *, *, #18552, .F. ) ;
#650 = CARTESIAN_POINT ( 'NONE',  ( -3.662846001189865142, 195.5725841191952838, 64.89886208192143613 ) ) ;
#651 = AXIS2_PLACEMENT_3D ( 'NONE', #1417, #30036, #33096 ) ;
#652 = ORIENTED_EDGE ( 'NONE', *, *, #19298, .T. ) ;
#653 = ORIENTED_EDGE ( 'NONE', *, *, #32062, .T. ) ;
#654 = CARTESIAN_POINT ( 'NONE',  ( 74.47499999726881015, 149.9369285172503510, 15.58253174999999580 ) ) ;
#655 = CARTESIAN_POINT ( 'NONE',  ( 53.11132485994280472, 140.7341522555726669, 4.635254915624211769 ) ) ;
#656 = CARTESIAN_POINT ( 'NONE',  ( 59.58867513459482979, 163.8167787843871110, 12.13525491562421621 ) ) ;
#657 = CARTESIAN_POINT ( 'NONE',  ( 4.903702542908601636, 200.1653181626581102, 47.45113791807857950 ) ) ;
#658 = PRESENTATION_STYLE_ASSIGNMENT (( #994 ) ) ;
#659 = CARTESIAN_POINT ( 'NONE',  ( -10.00000000000000711, 206.9523078486584495, 35.49886208192143044 ) ) ;
#660 = CARTESIAN_POINT ( 'NONE',  ( 68.17499999726881299, 164.1591823560292198, 12.60653300113718167 ) ) ;
#661 = ORIENTED_EDGE ( 'NONE', *, *, #43, .F. ) ;
#662 = FACE_OUTER_BOUND ( 'NONE', #15822, .T. ) ;
#663 = STYLED_ITEM ( 'NONE', ( #5034 ), #1878 ) ;
#664 = CARTESIAN_POINT ( 'NONE',  ( 43.58867513459482979, 163.8167787843871110, 12.13525491562421621 ) ) ;
#665 = CARTESIAN_POINT ( 'NONE',  ( 4.984841277089891776, 200.2242689037093726, 19.44886208192143329 ) ) ;
#666 = CARTESIAN_POINT ( 'NONE',  ( 6.139770520408368348, 198.4640165459539674, 47.45113791807857950 ) ) ;
#667 = CARTESIAN_POINT ( 'NONE',  ( 4.613983237546155358, -6.452243898629820507, -7.591546097228409451 ) ) ;
#668 = CARTESIAN_POINT ( 'NONE',  ( -6.220909254589537696, 198.5229672870051161, 39.05113791807856671 ) ) ;
#669 = CARTESIAN_POINT ( 'NONE',  ( 87.57499999726880446, 164.1591823560292198, -12.60653300113719766 ) ) ;
#670 = PRODUCT_CONTEXT ( 'NONE', #3757, 'mechanical' ) ;
#671 = CARTESIAN_POINT ( 'NONE',  ( -2.517493886309087880, 214.5937144450984135, 96.09886208192143897 ) ) ;
#672 = MANIFOLD_SOLID_BREP ( 'Boss-Extrude2', #22647 ) ;
#673 = CONICAL_SURFACE ( 'NONE', #14801, 15.50000000000001066, 0.3490658503988691153 ) ;
#674 = CARTESIAN_POINT ( 'NONE',  ( 40.02499999726881441, 160.0630714827496206, 15.58253174999999402 ) ) ;
#675 = CARTESIAN_POINT ( 'NONE',  ( 67.78867513459482552, 155.0000000000000000, 15.00000000000001243 ) ) ;
#676 = DIRECTION ( 'NONE',  ( -0.000000000000000000, -0.000000000000000000, -1.000000000000000000 ) ) ;
#677 = CARTESIAN_POINT ( 'NONE',  ( -3.662846001190052991, 218.4274158808045740, 22.10113791807856742 ) ) ;
#678 = CARTESIAN_POINT ( 'NONE',  ( -1.604619215278546562E-14, -7.505553499465138501, -0.8000000000000003775 ) ) ;
#679 = CARTESIAN_POINT ( 'NONE',  ( 55.77499999726881441, 169.8198683612136222, -4.815267126137197984 ) ) ;
#680 = CARTESIAN_POINT ( 'NONE',  ( 3.135527875058820690, 216.4958274776887492, 64.40113791807857524 ) ) ;
#681 = CARTESIAN_POINT ( 'NONE',  ( 8.062137200540920645, 201.0835637161417822, 41.30113791807857382 ) ) ;
#682 = DIRECTION ( 'NONE',  ( 0.000000000000000000, -1.000000000000000000, 0.000000000000000000 ) ) ;
#683 = LINE ( 'NONE', #11086, #20111 ) ;
#684 = CARTESIAN_POINT ( 'NONE',  ( -10.01549611932659545, 210.2015048109875011, 8.648862081921434353 ) ) ;
#685 = CARTESIAN_POINT ( 'NONE',  ( 62.29999999453762172, 167.3344367211045096, -8.961492836873482304 ) ) ;
#686 = ORIENTED_EDGE ( 'NONE', *, *, #637, .T. ) ;
#687 = CARTESIAN_POINT ( 'NONE',  ( -0.05014649552807705357, 194.3824533091408000, 44.75113791807856956 ) ) ;
#688 = DIRECTION ( 'NONE',  ( -0.000000000000000000, -0.000000000000000000, -1.000000000000000000 ) ) ;
#689 = CARTESIAN_POINT ( 'NONE',  ( 8.118202686958138514, 201.1607312380088501, 22.29886208192143826 ) ) ;
#690 = FACE_BOUND ( 'NONE', #27435, .T. ) ;
#691 = ORIENTED_EDGE ( 'NONE', *, *, #18686, .T. ) ;
#692 = AXIS2_PLACEMENT_3D ( 'NONE', #23356, #15003, #10082 ) ;
#693 = CARTESIAN_POINT ( 'NONE',  ( -0.05014649552810635652, 196.4853777576173002, 83.75113791807856956 ) ) ;
#694 = EDGE_LOOP ( 'NONE', ( #19337, #26108, #32446, #26781 ) ) ;
#695 = CARTESIAN_POINT ( 'NONE',  ( 117.5000000000000142, 155.0000000000000000, 100.0000000000000284 ) ) ;
#696 = CARTESIAN_POINT ( 'NONE',  ( -6.725979247667767780, -3.622307570260316911, -6.470294263593358686 ) ) ;
#697 = VERTEX_POINT ( 'NONE', #18883 ) ;
#698 = CIRCLE ( 'NONE', #9954, 4.057500000000000107 ) ;
#699 = CARTESIAN_POINT ( 'NONE',  ( -6.500168698208129925, 202.3363017425936050, 21.20113791807856529 ) ) ;
#700 = B_SPLINE_CURVE_WITH_KNOTS ( 'NONE', 3,
 ( #29050, #23768, #21044, #6513, #433, #21210 ),
 .UNSPECIFIED., .F., .F.,
 ( 4, 2, 4 ),
 ( -4.604908129293502741E-06, 0.0003318387708545218599, 0.0006682824498383372301 ),
 .UNSPECIFIED. ) ;
#701 = AXIS2_PLACEMENT_3D ( 'NONE', #11341, #16437, #6045 ) ;
#702 = CARTESIAN_POINT ( 'NONE',  ( -60.87270596256635713, 194.9921970430798979, -0.8044259506661830539 ) ) ;
#703 = CARTESIAN_POINT ( 'NONE',  ( 3.135527875058981895, 197.5041725223112792, 7.598862081921435419 ) ) ;
#704 = CARTESIAN_POINT ( 'NONE',  ( 44.67499999726881299, 141.7447067706911810, 9.630534252274376428 ) ) ;
#705 = ORIENTED_EDGE ( 'NONE', *, *, #23746, .F. ) ;
#706 = CARTESIAN_POINT ( 'NONE',  ( 49.02499999726880731, 149.9369285172503510, -15.58253175000000823 ) ) ;
#707 = CARTESIAN_POINT ( 'NONE',  ( 94.70964751525852421, 155.0000000000000000, 32.10452846326766974 ) ) ;
#708 = CARTESIAN_POINT ( 'NONE',  ( 61.58867513459482979, 163.8167787843871110, 12.13525491562421621 ) ) ;
#709 = CARTESIAN_POINT ( 'NONE',  ( -125.0000000000000000, 0.000000000000000000, 35.00000000000000000 ) ) ;
#710 = CARTESIAN_POINT ( 'NONE',  ( 10.01549611932659545, 203.7984951890123853, 85.14886208192143613 ) ) ;
#711 = CARTESIAN_POINT ( 'NONE',  ( 55.67499999726879878, 168.2552932293087906, -9.630534252274385310 ) ) ;
#712 = CARTESIAN_POINT ( 'NONE',  ( 10.01549611932653860, 210.2015048109876716, 25.85113791807856742 ) ) ;
#713 = FACE_OUTER_BOUND ( 'NONE', #1487, .T. ) ;
#714 = CARTESIAN_POINT ( 'NONE',  ( 3.662846001189864698, 218.4274158808046593, 75.39886208192143613 ) ) ;
#715 = CIRCLE ( 'NONE', #5600, 13.00000000000003908 ) ;
#716 = CARTESIAN_POINT ( 'NONE',  ( 73.40000000000000568, 159.7113355953771077, 14.49999999999999289 ) ) ;
#717 = CARTESIAN_POINT ( 'NONE',  ( 64.98867513459482836, 163.8167787843871110, -12.13525491562423397 ) ) ;
#718 = DIRECTION ( 'NONE',  ( 0.000000000000000000, 0.000000000000000000, -1.000000000000000000 ) ) ;
#719 = CARTESIAN_POINT ( 'NONE',  ( 10.00000000000000711, 206.9523078486586201, 86.00113791807858377 ) ) ;
#720 = DIRECTION ( 'NONE',  ( 0.000000000000000000, -0.7071067811865506814, -0.7071067811865442421 ) ) ;
#721 = CARTESIAN_POINT ( 'NONE',  ( 35.77499999726881441, 169.8198683612136222, -4.815267126137197984 ) ) ;
#722 = CARTESIAN_POINT ( 'NONE',  ( -8.062137200540920645, 212.9164362838581894, 39.80113791807857382 ) ) ;
#723 = EDGE_CURVE ( 'NONE', #697, #15536, #20846, .T. ) ;
#724 =( REPRESENTATION_RELATIONSHIP ('NONE','NONE', #25663, #17605 ) REPRESENTATION_RELATIONSHIP_WITH_TRANSFORMATION ( #19234 )SHAPE_REPRESENTATION_RELATIONSHIP( ) );
#725 = CARTESIAN_POINT ( 'NONE',  ( 79.92499999726881299, 164.1591823560292198, 12.60653300113718167 ) ) ;
#726 = EDGE_LOOP ( 'NONE', ( #4770, #12905, #31541, #10132, #32533 ) ) ;
#727 = DIRECTION ( 'NONE',  ( 1.000000000000000000, -0.000000000000000000, -0.000000000000000000 ) ) ;
#728 = CIRCLE ( 'NONE', #9429, 2.000000000000000888 ) ;
#729 = CARTESIAN_POINT ( 'NONE',  ( 42.29999999453763593, 167.3344367211045096, -8.961492836873482304 ) ) ;
#730 = CARTESIAN_POINT ( 'NONE',  ( 7.456977232089302632, 217.1783343296989131, 7.551137918078564049 ) ) ;
#731 = AXIS2_PLACEMENT_3D ( 'NONE', #2930, #31053, #13311 ) ;
#732 = DIRECTION ( 'NONE',  ( 0.000000000000000000, 0.000000000000000000, 1.000000000000000000 ) ) ;
#733 = CARTESIAN_POINT ( 'NONE',  ( 3.500000000000004441, -0.6807265984995718444, -0.02935130719647200889 ) ) ;
#734 = VERTEX_POINT ( 'NONE', #15326 ) ;
#735 = CARTESIAN_POINT ( 'NONE',  ( -6.139770520408224463, 198.4640165459539105, 98.04886208192142760 ) ) ;
#736 = CARTESIAN_POINT ( 'NONE',  ( 12.01549611932659367, 203.1486557965466773, 37.14886208192143613 ) ) ;
#737 = CARTESIAN_POINT ( 'NONE',  ( -58.50000000000002132, 209.9999999999999716, 0.000000000000000000 ) ) ;
#738 = CARTESIAN_POINT ( 'NONE',  ( 10.01549611932653860, 210.2015048109876716, 55.85113791807857808 ) ) ;
#739 = VERTEX_POINT ( 'NONE', #3543 ) ;
#740 = CARTESIAN_POINT ( 'NONE',  ( -4.984841277089891776, 213.7757310962905990, 14.94886208192143506 ) ) ;
#741 = AXIS2_PLACEMENT_3D ( 'NONE', #7083, #30078, #6742 ) ;
#742 = EDGE_LOOP ( 'NONE', ( #22101, #21274, #7659, #32959, #16898 ) ) ;
#743 = CARTESIAN_POINT ( 'NONE',  ( -6.444103211790928043, 202.2591342207265939, 86.19886208192144750 ) ) ;
#744 = EDGE_CURVE ( 'NONE', #14095, #15702, #8660, .T. ) ;
#745 = CARTESIAN_POINT ( 'NONE',  ( -2.426778023690262742, 214.6231898156240163, 34.10113791807857098 ) ) ;
#746 = CARTESIAN_POINT ( 'NONE',  ( 7.500000000000000000, -1.486698507076798847, -0.09861472150523931113 ) ) ;
#747 = VERTEX_POINT ( 'NONE', #26712 ) ;
#748 = CARTESIAN_POINT ( 'NONE',  ( 100.4058500716420781, 155.0000000000000000, 0.000000000000000000 ) ) ;
#749 = AXIS2_PLACEMENT_3D ( 'NONE', #5267, #20944, #26062 ) ;
#750 = CARTESIAN_POINT ( 'NONE',  ( 36.87499999726881583, 138.6155565068815463, -3.929120461958505118E-15 ) ) ;
#751 = DIRECTION ( 'NONE',  ( 0.000000000000000000, 0.000000000000000000, 1.000000000000000000 ) ) ;
#752 = CARTESIAN_POINT ( 'NONE',  ( 4.903702542908601636, 200.1653181626581102, 95.45113791807858661 ) ) ;
#753 = DIRECTION ( 'NONE',  ( 0.000000000000000000, -0.7071067811865487940, -0.7071067811865463515 ) ) ;
#754 = CARTESIAN_POINT ( 'NONE',  ( 53.19999999999998863, 167.3344367211045096, 8.961492836873468093 ) ) ;
#755 = CARTESIAN_POINT ( 'NONE',  ( 8.000000000000008882, 207.0476921513415220, 75.99886208192144466 ) ) ;
#756 = DIRECTION ( 'NONE',  ( -1.000000000000000000, -0.000000000000000000, -0.000000000000000000 ) ) ;
#757 = EDGE_CURVE ( 'NONE', #31949, #12310, #32158, .T. ) ;
#758 = CARTESIAN_POINT ( 'NONE',  ( 55.22499999726880304, 160.0630714827496206, -15.58253175000000823 ) ) ;
#759 = CARTESIAN_POINT ( 'NONE',  ( -9.984503880673475606, 210.2968891136704315, 6.651137918078565470 ) ) ;
#760 = CARTESIAN_POINT ( 'NONE',  ( 37.51132485994280330, 146.1832212156128890, -12.13525491562423042 ) ) ;
#761 = CARTESIAN_POINT ( 'NONE',  ( 62.72499999726881015, 140.1801316387863778, -4.815267126137194431 ) ) ;
#762 = CARTESIAN_POINT ( 'NONE',  ( 76.87499999726881583, 138.6155565068815463, -3.929120461958505118E-15 ) ) ;
#763 = CARTESIAN_POINT ( 'NONE',  ( 7.456977232089302632, 217.1783343296989131, 73.55113791807856671 ) ) ;
#764 = ADVANCED_FACE ( 'NONE', ( #27053 ), #13424, .T. ) ;
#765 = CARTESIAN_POINT ( 'NONE',  ( 10.01549611932653860, 210.2015048109876716, 100.8511379180785639 ) ) ;
#766 = PLANE ( 'NONE',  #3114 ) ;
#767 = EDGE_CURVE ( 'NONE', #31501, #25247, #11551, .T. ) ;
#768 = ORIENTED_EDGE ( 'NONE', *, *, #31535, .F. ) ;
#769 = CARTESIAN_POINT ( 'NONE',  ( 10.00000000000000711, 207.0476921513415220, 0.9988620819214343305 ) ) ;
#770 = CARTESIAN_POINT ( 'NONE',  ( 12.00000000000000711, 207.0476921513415220, 60.99886208192143044 ) ) ;
#771 = CARTESIAN_POINT ( 'NONE',  ( -0.05014649552828402690, 217.5146222423826714, 66.24886208192143044 ) ) ;
#772 = CIRCLE ( 'NONE', #14370, 2.149999999999994138 ) ;
#773 = CARTESIAN_POINT ( 'NONE',  ( 7.456977232089471386, 196.8216656703012006, 4.448862081921434175 ) ) ;
#774 = CARTESIAN_POINT ( 'NONE',  ( -67.50000599999999906, 155.0000000000000000, -17.00000000000000711 ) ) ;
#775 = CARTESIAN_POINT ( 'NONE',  ( -8.118202686958039038, 201.1607312380087080, 21.20113791807856529 ) ) ;
#776 = CIRCLE ( 'NONE', #1871, 69.99999999999998579 ) ;
#777 = CARTESIAN_POINT ( 'NONE',  ( 8.118202686958138514, 201.1607312380088501, 82.29886208192144181 ) ) ;
#778 = ORIENTED_EDGE ( 'NONE', *, *, #23557, .F. ) ;
#779 = DIRECTION ( 'NONE',  ( -0.1461455375466716444, 0.9854922318508084755, -0.08629335326029916042 ) ) ;
#780 = VERTEX_POINT ( 'NONE', #29440 ) ;
#781 = DIRECTION ( 'NONE',  ( 0.000000000000000000, 0.000000000000000000, -1.000000000000000000 ) ) ;
#782 = CARTESIAN_POINT ( 'NONE',  ( -7.984503880673422316, 204.3529502787951628, 62.34886208192144608 ) ) ;
#783 = EDGE_LOOP ( 'NONE', ( #26414, #22482, #29062, #10811 ) ) ;
#784 = ADVANCED_FACE ( 'NONE', ( #16487 ), #3096, .F. ) ;
#785 = CARTESIAN_POINT ( 'NONE',  ( 76.12499999726881583, 155.0000000000000000, 15.58253174999999402 ) ) ;
#786 = ORIENTED_EDGE ( 'NONE', *, *, #16132, .F. ) ;
#787 = FACE_OUTER_BOUND ( 'NONE', #21644, .T. ) ;
#788 = MECHANICAL_DESIGN_GEOMETRIC_PRESENTATION_REPRESENTATION (  '', ( #15484 ), #5146 ) ;
#789 = MANIFOLD_SOLID_BREP ( 'CirPattern1', #11241 ) ;
#790 = UNCERTAINTY_MEASURE_WITH_UNIT (LENGTH_MEASURE( 1.000000000000000082E-05 ), #19917, 'distance_accuracy_value', 'NONE');
#791 = ADVANCED_FACE ( 'NONE', ( #31825 ), #29110, .T. ) ;
#792 = CARTESIAN_POINT ( 'NONE',  ( 70.02499999726879309, 160.0630714827496206, 15.58253174999999402 ) ) ;
#793 = CARTESIAN_POINT ( 'NONE',  ( 4.984841277089725686, 213.7757310962907411, 67.55113791807856671 ) ) ;
#794 = CARTESIAN_POINT ( 'NONE',  ( 101.3062541159399075, 155.0000000000000000, -12.00000000000001066 ) ) ;
#795 = SURFACE_STYLE_FILL_AREA ( #10535 ) ;
#796 = CARTESIAN_POINT ( 'NONE',  ( 33.59999999999998721, 150.2886644046228639, 14.49999999999999645 ) ) ;
#797 = CARTESIAN_POINT ( 'NONE',  ( 8.015496119326595448, 204.4483345814782638, 40.14886208192143613 ) ) ;
#798 = CARTESIAN_POINT ( 'NONE',  ( 0.05014649552810505201, 217.5146222423826714, 76.25113791807855534 ) ) ;
#799 = CARTESIAN_POINT ( 'NONE',  ( -3.135527875058821579, 197.5041725223112223, 68.90113791807857524 ) ) ;
#800 = DIRECTION ( 'NONE',  ( 0.9366133782696114407, 0.000000000000000000, 0.3503646381220365535 ) ) ;
#801 = CARTESIAN_POINT ( 'NONE',  ( -2.517493886308901807, 199.4062855549015012, 23.90113791807857169 ) ) ;
#802 = CARTESIAN_POINT ( 'NONE',  ( 125.5000000000000000, 228.4330392262228600, -76.47359838532526055 ) ) ;
#803 = CARTESIAN_POINT ( 'NONE',  ( 6.500000000000000000, 3.752776749732573247, -0.8000000000000003775 ) ) ;
#804 = CARTESIAN_POINT ( 'NONE',  ( 45.02499999726881441, 149.9369285172503510, -15.58253175000000823 ) ) ;
#805 = CARTESIAN_POINT ( 'NONE',  ( -11.98450388067348804, 210.9467285061362247, 51.65113791807857524 ) ) ;
#806 = CARTESIAN_POINT ( 'NONE',  ( -130.2500000000000000, 6.429395695523609083E-16, 35.00000599999999906 ) ) ;
#807 = CARTESIAN_POINT ( 'NONE',  ( 6.220909254589536808, 215.4770327129947702, 94.55113791807858092 ) ) ;
#808 = CARTESIAN_POINT ( 'NONE',  ( 6.220909254589536808, 215.4770327129947987, 64.55113791807858092 ) ) ;
#809 = CARTESIAN_POINT ( 'NONE',  ( -12.01549611932659722, 210.8513442034533227, 29.64886208192143968 ) ) ;
#810 = CARTESIAN_POINT ( 'NONE',  ( -8.062137200540822946, 201.0835637161416400, 38.19886208192143329 ) ) ;
#811 = CARTESIAN_POINT ( 'NONE',  ( 87.99999999453763166, 155.0000000000000000, -14.50000000000000711 ) ) ;
#812 = CARTESIAN_POINT ( 'NONE',  ( 3.662846001190051659, 195.5725841191953691, 77.60113791807854966 ) ) ;
#813 = CARTESIAN_POINT ( 'NONE',  ( 2.426778023690261410, 199.3768101843759837, 101.6011379180785781 ) ) ;
#814 = EDGE_CURVE ( 'NONE', #4673, #6298, #27597, .T. ) ;
#815 = CARTESIAN_POINT ( 'NONE',  ( -6.220909254589682469, 215.4770327129946850, 47.94886208192144039 ) ) ;
#816 = DIRECTION ( 'NONE',  ( -1.000000000000000000, -0.000000000000000000, 0.000000000000000000 ) ) ;
#817 = ORIENTED_EDGE ( 'NONE', *, *, #26586, .F. ) ;
#818 = CARTESIAN_POINT ( 'NONE',  ( 3.753561863808876797, 195.6020594897209719, 61.59886208192143897 ) ) ;
#819 = ORIENTED_EDGE ( 'NONE', *, *, #16423, .F. ) ;
#820 = CARTESIAN_POINT ( 'NONE',  ( -6.444103211790928043, 202.2591342207265939, 32.19886208192144039 ) ) ;
#821 = ORIENTED_EDGE ( 'NONE', *, *, #24714, .F. ) ;
#822 = EDGE_CURVE ( 'NONE', #562, #11454, #3119, .T. ) ;
#823 = CARTESIAN_POINT ( 'NONE',  ( 75.67499999726881299, 168.2552932293087906, -9.630534252274387086 ) ) ;
#824 = DIRECTION ( 'NONE',  ( 1.000000000000000000, -0.000000000000000000, -0.000000000000000000 ) ) ;
#825 = CARTESIAN_POINT ( 'NONE',  ( 58.78867513459481842, 155.0000000000000000, -15.00000000000002487 ) ) ;
#826 = CARTESIAN_POINT ( 'NONE',  ( 7.984503880673485376, 204.3529502787953902, 56.15113791807857524 ) ) ;
#827 = EDGE_CURVE ( 'NONE', #18269, #18960, #27386, .T. ) ;
#828 = CARTESIAN_POINT ( 'NONE',  ( 3.044812012439969795, 216.5253028482143520, 30.39886208192143613 ) ) ;
#829 = CARTESIAN_POINT ( 'NONE',  ( 70.97499999726881015, 140.1801316387863778, -4.815267126137194431 ) ) ;
#830 = EDGE_LOOP ( 'NONE', ( #26379, #19429, #20513, #9975 ) ) ;
#831 = DIRECTION ( 'NONE',  ( -1.000000000000000000, -0.000000000000000000, -0.000000000000000000 ) ) ;
#832 = SURFACE_STYLE_FILL_AREA ( #18565 ) ;
#833 = DIRECTION ( 'NONE',  ( 0.000000000000000000, 0.000000000000000000, -1.000000000000000000 ) ) ;
#834 = CARTESIAN_POINT ( 'NONE',  ( 2.517493886309087436, 199.4062855549015865, 16.59886208192143897 ) ) ;
#835 = CARTESIAN_POINT ( 'NONE',  ( -3.044812012440131443, 216.5253028482142952, 49.10113791807857808 ) ) ;
#836 = CARTESIAN_POINT ( 'NONE',  ( 83.78867513459482552, 155.0000000000000000, 15.00000000000001243 ) ) ;
#837 = CARTESIAN_POINT ( 'NONE',  ( 8.062137200540920645, 201.0835637161417822, 35.30113791807857382 ) ) ;
#838 = CARTESIAN_POINT ( 'NONE',  ( 85.07499999726880446, 141.7447067706911810, -9.630534252274385310 ) ) ;
#839 = CONTEXT_DEPENDENT_SHAPE_REPRESENTATION ( #15296, #20613 ) ;
#840 = CARTESIAN_POINT ( 'NONE',  ( -4.903702542908436435, 200.1653181626580249, 104.0488620819214560 ) ) ;
#841 = CARTESIAN_POINT ( 'NONE',  ( 39.42499999726881299, 168.2552932293087906, -9.630534252274385310 ) ) ;
#842 = CARTESIAN_POINT ( 'NONE',  ( 36.68867513459482410, 150.1262045565068206, -15.00000000000030909 ) ) ;
#843 = DIRECTION ( 'NONE',  ( 0.000000000000000000, 0.7071067811865442421, -0.7071067811865506814 ) ) ;
#844 = CARTESIAN_POINT ( 'NONE',  ( -7.456977232089304408, 196.8216656703010301, 21.05113791807857027 ) ) ;
#845 = CARTESIAN_POINT ( 'NONE',  ( 33.37499999726880873, 155.0000000000000000, -15.58253175000000823 ) ) ;
#846 = CARTESIAN_POINT ( 'NONE',  ( 63.07499999726881867, 141.7447067706911810, -9.630534252274385310 ) ) ;
#847 = CARTESIAN_POINT ( 'NONE',  ( -6.139770520408369237, 215.5359834540460042, 66.95113791807858661 ) ) ;
#848 = CARTESIAN_POINT ( 'NONE',  ( -10.01549611932653860, 203.7984951890123000, 39.35113791807857098 ) ) ;
#849 = LINE ( 'NONE', #23689, #23558 ) ;
#850 = CARTESIAN_POINT ( 'NONE',  ( -7.500000000000000888, 2.886751345948126435, -7.198902722707427593 ) ) ;
#851 = CARTESIAN_POINT ( 'NONE',  ( -3.662846001189865142, 195.5725841191952838, 4.898862081921434353 ) ) ;
#852 = CARTESIAN_POINT ( 'NONE',  ( -3.044812012439970683, 197.4746971517856196, 10.89886208192143613 ) ) ;
#853 = CARTESIAN_POINT ( 'NONE',  ( 63.29999999453762882, 142.6655632788954620, 8.961492836873471646 ) ) ;
#854 = VERTEX_POINT ( 'NONE', #11721 ) ;
#855 = CARTESIAN_POINT ( 'NONE',  ( 0.05014649552807549926, 219.6175466908591716, 49.25113791807856956 ) ) ;
#856 = CARTESIAN_POINT ( 'NONE',  ( 77.01132485994283172, 142.2402378747194405, 9.270509831248432420 ) ) ;
#857 = CARTESIAN_POINT ( 'NONE',  ( -8.062137200540822946, 201.0835637161416400, 17.19886208192143684 ) ) ;
#858 = EDGE_CURVE ( 'NONE', #11477, #33308, #3671, .T. ) ;
#859 = CARTESIAN_POINT ( 'NONE',  ( 72.01132485994281751, 167.7597621252805880, -9.270509831248443078 ) ) ;
#860 = VERTEX_POINT ( 'NONE', #29951 ) ;
#861 = CARTESIAN_POINT ( 'NONE',  ( -9.984503880673473830, 210.2968891136704315, 84.65113791807857524 ) ) ;
#862 = ORIENTED_EDGE ( 'NONE', *, *, #26257, .T. ) ;
#863 = EDGE_CURVE ( 'NONE', #32863, #21974, #12924, .T. ) ;
#864 = LINE ( 'NONE', #21144, #15127 ) ;
#865 = DIRECTION ( 'NONE',  ( 1.000000000000000000, 0.000000000000000000, 0.000000000000000000 ) ) ;
#866 = VERTEX_POINT ( 'NONE', #12225 ) ;
#867 = CARTESIAN_POINT ( 'NONE',  ( 4.903702542908601636, 200.1653181626581102, 23.45113791807856884 ) ) ;
#868 = CARTESIAN_POINT ( 'NONE',  ( -60.48814638060569848, 194.9711715815534205, -1.524404325634890700 ) ) ;
#869 = CARTESIAN_POINT ( 'NONE',  ( -9.984503880673420539, 203.7031108863293980, 2.348862081921433198 ) ) ;
#870 = CARTESIAN_POINT ( 'NONE',  ( 51.47499999726881725, 160.0630714827496206, -15.58253175000000823 ) ) ;
#871 = ORIENTED_EDGE ( 'NONE', *, *, #13443, .T. ) ;
#872 = CARTESIAN_POINT ( 'NONE',  ( 60.02499999726880020, 160.0630714827496206, 15.58253174999999402 ) ) ;
#873 = DIRECTION ( 'NONE',  ( 0.000000000000000000, -1.000000000000000000, 0.000000000000000000 ) ) ;
#874 = DIRECTION ( 'NONE',  ( 1.000000000000000000, 0.000000000000000000, 0.000000000000000000 ) ) ;
#875 = DIRECTION ( 'NONE',  ( 0.000000000000000000, 0.000000000000000000, -1.000000000000000000 ) ) ;
#876 = CARTESIAN_POINT ( 'NONE',  ( -8.062137200540822946, 201.0835637161416400, 86.19886208192144750 ) ) ;
#877 = CARTESIAN_POINT ( 'NONE',  ( 59.17499999726881299, 145.8408176439707802, -12.60653300113719588 ) ) ;
#878 = CARTESIAN_POINT ( 'NONE',  ( 6.139770520408368348, 198.4640165459539674, 26.45113791807856884 ) ) ;
#879 = CARTESIAN_POINT ( 'NONE',  ( 7.500000000000000888, 1.443375672974060109, -7.063244554130000630 ) ) ;
#880 = CARTESIAN_POINT ( 'NONE',  ( -7.456977232089471386, 217.1783343296987709, 77.94886208192143329 ) ) ;
#881 = CONICAL_SURFACE ( 'NONE', #18301, 31.00000000000000000, 1.466076571675255957 ) ;
#882 = CARTESIAN_POINT ( 'NONE',  ( 74.09999999999999432, 141.2096805137202580, -4.480746418436742040 ) ) ;
#883 = CARTESIAN_POINT ( 'NONE',  ( -3.249999999999996891, 5.629165124598855208, -5.592027715088710771 ) ) ;
#884 = CARTESIAN_POINT ( 'NONE',  ( 6.220909254589536808, 215.4770327129947702, 91.55113791807858092 ) ) ;
#885 = CARTESIAN_POINT ( 'NONE',  ( 92.70168066101555837, 155.0000000000000000, -13.00000000000003908 ) ) ;
#886 = CARTESIAN_POINT ( 'NONE',  ( 40.77499999726881441, 140.1801316387863778, 4.815267126137185549 ) ) ;
#887 = CARTESIAN_POINT ( 'NONE',  ( -3.135527875058821579, 197.5041725223112223, 32.90113791807857524 ) ) ;
#888 = CARTESIAN_POINT ( 'NONE',  ( 75.32499999726881867, 164.1591823560292198, -12.60653300113719766 ) ) ;
#889 = VERTEX_POINT ( 'NONE', #33000 ) ;
#890 = DIRECTION ( 'NONE',  ( -1.000000000000000000, -0.000000000000000000, -0.000000000000000000 ) ) ;
#891 = CARTESIAN_POINT ( 'NONE',  ( 41.99999999453763166, 155.0000000000000000, -14.50000000000000711 ) ) ;
#892 = CARTESIAN_POINT ( 'NONE',  ( -12.01549611932652972, 203.1486557965464499, 24.35113791807856742 ) ) ;
#893 = CARTESIAN_POINT ( 'NONE',  ( 40.71132485994280614, 155.0000000000000000, 15.00000000000001243 ) ) ;
#894 = CARTESIAN_POINT ( 'NONE',  ( -67.50000000000000000, -92.00000000000000000, 17.00000000000001421 ) ) ;
#895 = VERTEX_POINT ( 'NONE', #9668 ) ;
#896 = CARTESIAN_POINT ( 'NONE',  ( -12.01549611932659722, 210.8513442034533227, 29.64886208192143968 ) ) ;
#897 = DIRECTION ( 'NONE',  ( 0.000000000000000000, -1.000000000000000000, 0.000000000000000000 ) ) ;
#898 = CARTESIAN_POINT ( 'NONE',  ( -8.062137200540920645, 212.9164362838581894, 48.80113791807857382 ) ) ;
#899 = ORIENTED_EDGE ( 'NONE', *, *, #32978, .F. ) ;
#900 = CARTESIAN_POINT ( 'NONE',  ( 4.903702542908435547, 213.8346818373419751, 12.54886208192143826 ) ) ;
#901 = AXIS2_PLACEMENT_3D ( 'NONE', #15694, #7192, #17748 ) ;
#902 = AXIS2_PLACEMENT_3D ( 'NONE', #9614, #1446, #27504 ) ;
#903 = PRODUCT_DEFINITION_CONTEXT ( 'detailed design', #2680, 'design' ) ;
#904 = CARTESIAN_POINT ( 'NONE',  ( 127.5000000000000000, 155.0000000000000000, -6.938893903907228378E-15 ) ) ;
#905 = EDGE_LOOP ( 'NONE', ( #26424, #10889, #20231, #20681, #20609 ) ) ;
#906 = CARTESIAN_POINT ( 'NONE',  ( 0.05014649552828262524, 198.5883022060938572, 103.7488620819214304 ) ) ;
#907 = CARTESIAN_POINT ( 'NONE',  ( -0.05014649552807731031, 198.5883022060938572, 38.75113791807856956 ) ) ;
#908 = FACE_OUTER_BOUND ( 'NONE', #23376, .T. ) ;
#910 = ORIENTED_EDGE ( 'NONE', *, *, #16888, .T. ) ;
#909 = VECTOR ( 'NONE', #224, 1000.000000000000000 ) ;
#911 = CARTESIAN_POINT ( 'NONE',  ( 37.02499999726880020, 149.9369285172503510, -15.58253175000000823 ) ) ;
#912 = CARTESIAN_POINT ( 'NONE',  ( 9.984503880673420539, 210.2968891136705167, 63.84886208192142476 ) ) ;
#913 = CARTESIAN_POINT ( 'NONE',  ( 88.02499999726880731, 160.0630714827496206, 15.58253174999999402 ) ) ;
#914 = DIRECTION ( 'NONE',  ( 0.000000000000000000, 1.000000000000000000, -6.454785026890489601E-15 ) ) ;
#915 = CARTESIAN_POINT ( 'NONE',  ( -6.500168698208129925, 202.3363017425936050, 102.2011379180785866 ) ) ;
#916 = APPLICATION_CONTEXT ( 'automotive_design' ) ;
#917 = CARTESIAN_POINT ( 'NONE',  ( 55.10000000000000142, 168.7903194862797420, 4.480746418436729606 ) ) ;
#918 = CARTESIAN_POINT ( 'NONE',  ( 6.500168698208244500, 202.3363017425938324, 73.29886208192142760 ) ) ;
#919 = DIRECTION ( 'NONE',  ( 0.000000000000000000, 0.9949972439410068592, -0.09990237509589369735 ) ) ;
#920 = AXIS2_PLACEMENT_3D ( 'NONE', #13262, #15985, #26700 ) ;
#921 = CARTESIAN_POINT ( 'NONE',  ( 55.82499999726880446, 168.2552932293087906, 9.630534252274372875 ) ) ;
#922 = VECTOR ( 'NONE', #2392, 1000.000000000000114 ) ;
#924 = ORIENTED_EDGE ( 'NONE', *, *, #32237, .F. ) ;
#923 = CARTESIAN_POINT ( 'NONE',  ( 10.01549611932653860, 210.2015048109876716, 7.851137918078565647 ) ) ;
#925 = DIRECTION ( 'NONE',  ( 0.000000000000000000, 0.000000000000000000, -1.000000000000000000 ) ) ;
#926 = CARTESIAN_POINT ( 'NONE',  ( 65.12499999726881583, 155.0000000000000000, -15.58253175000000823 ) ) ;
#927 = CARTESIAN_POINT ( 'NONE',  ( 73.47499999726878173, 160.0630714827496206, -15.58253175000000823 ) ) ;
#928 = CARTESIAN_POINT ( 'NONE',  ( -12.00000000000000711, 207.0476921513413515, 75.50113791807856956 ) ) ;
#929 = CARTESIAN_POINT ( 'NONE',  ( 8.118202686958039038, 212.8392687619912635, 97.70113791807857240 ) ) ;
#930 = VECTOR ( 'NONE', #7597, 1000.000000000000114 ) ;
#931 = EDGE_LOOP ( 'NONE', ( #7883, #32623, #17410, #12258 ) ) ;
#932 = CARTESIAN_POINT ( 'NONE',  ( -6.220909254589682469, 215.4770327129946850, 2.948862081921434175 ) ) ;
#933 = CARTESIAN_POINT ( 'NONE',  ( -9.680171189290716072, 199.9079932115567146, 59.19886208192144750 ) ) ;
#934 = CARTESIAN_POINT ( 'NONE',  ( 0.05014649552828275014, 196.4853777576173002, 70.74886208192143044 ) ) ;
#935 = CARTESIAN_POINT ( 'NONE',  ( 9.680171189290716072, 214.0920067884432854, 6.698862081921434175 ) ) ;
#936 = CARTESIAN_POINT ( 'NONE',  ( -67.50001199999998391, 160.4776661921571588, -16.13174377802661752 ) ) ;
#937 = CARTESIAN_POINT ( 'NONE',  ( -6.220909254589537696, 198.5229672870051161, 27.05113791807856671 ) ) ;
#938 = CARTESIAN_POINT ( 'NONE',  ( 9.984503880673420539, 210.2968891136705167, 90.84886208192143897 ) ) ;
#939 = ORIENTED_EDGE ( 'NONE', *, *, #757, .F. ) ;
#940 = CARTESIAN_POINT ( 'NONE',  ( 63.21132485994281325, 139.2280666364260071, -4.041636747397287284E-15 ) ) ;
#941 = ORIENTED_EDGE ( 'NONE', *, *, #22042, .T. ) ;
#942 = LINE ( 'NONE', #11680, #28706 ) ;
#943 = CARTESIAN_POINT ( 'NONE',  ( -2.517493886309087880, 214.5937144450984135, 72.09886208192142476 ) ) ;
#944 = ORIENTED_EDGE ( 'NONE', *, *, #7946, .F. ) ;
#945 = EDGE_CURVE ( 'NONE', #28898, #31739, #6447, .T. ) ;
#946 = AXIS2_PLACEMENT_3D ( 'NONE', #5551, #781, #28896 ) ;
#947 = CARTESIAN_POINT ( 'NONE',  ( 74.82499999726881867, 141.7447067706911810, -9.630534252274387086 ) ) ;
#948 = VERTEX_POINT ( 'NONE', #16827 ) ;
#949 = CARTESIAN_POINT ( 'NONE',  ( -0.5219667817988843384, 7.204195837485507958, -0.5602453477493336553 ) ) ;
#950 = CIRCLE ( 'NONE', #16649, 27.99999999999999645 ) ;
#951 = MANIFOLD_SOLID_BREP ( 'EndChamfer', #26460 ) ;
#952 = CARTESIAN_POINT ( 'NONE',  ( 67.22499999726879594, 160.0630714827496206, -15.58253175000000823 ) ) ;
#953 = CARTESIAN_POINT ( 'NONE',  ( -8.015496119326531499, 204.4483345814780364, 69.35113791807857808 ) ) ;
#954 = CARTESIAN_POINT ( 'NONE',  ( 109.0104235265664272, 155.0000000000000000, -11.99999999999998224 ) ) ;
#955 = VECTOR ( 'NONE', #756, 1000.000000000000000 ) ;
#956 = DIRECTION ( 'NONE',  ( 1.000000000000000000, 2.912190848224676732E-17, -6.099278249758083281E-16 ) ) ;
#957 = CARTESIAN_POINT ( 'NONE',  ( 35.20000000000000284, 167.3344367211045096, 8.961492836873468093 ) ) ;
#958 = CARTESIAN_POINT ( 'NONE',  ( -6.500168698208244500, 211.6636982574061676, 41.79886208192144181 ) ) ;
#959 = CARTESIAN_POINT ( 'NONE',  ( 10.01549611932653860, 210.2015048109876716, 76.85113791807857808 ) ) ;
#960 = CARTESIAN_POINT ( 'NONE',  ( -8.118202686958039038, 201.1607312380087080, 69.20113791807858661 ) ) ;
#961 = CARTESIAN_POINT ( 'NONE',  ( 117.5000000000000000, 63.20130719884917170, -52.99999999999946709 ) ) ;
#962 = CARTESIAN_POINT ( 'NONE',  ( 2.426778023690261410, 199.3768101843759837, 20.60113791807856742 ) ) ;
#963 = CARTESIAN_POINT ( 'NONE',  ( 6.250000000000000888, 5.051814855409225480, -7.198902722707425816 ) ) ;
#964 = CARTESIAN_POINT ( 'NONE',  ( -3.499999999999999556, -0.6807265984995715113, -0.02935130719646900088 ) ) ;
#965 = CARTESIAN_POINT ( 'NONE',  ( 44.42499999726881299, 141.7447067706911810, 9.630534252274376428 ) ) ;
#966 = CARTESIAN_POINT ( 'NONE',  ( 11.98450388067348271, 203.0532714938637753, 47.15113791807857524 ) ) ;
#967 = CARTESIAN_POINT ( 'NONE',  ( 7.500000000000000000, 3.948247735265829395, -7.349893093595813554 ) ) ;
#968 = VECTOR ( 'NONE', #31908, 1000.000000000000000 ) ;
#969 = CARTESIAN_POINT ( 'NONE',  ( 3.044812012440130555, 197.4746971517856764, 92.60113791807857808 ) ) ;
#970 = CARTESIAN_POINT ( 'NONE',  ( -10.01549611932653860, 203.7984951890123000, 72.35113791807857808 ) ) ;
#971 = AXIS2_PLACEMENT_3D ( 'NONE', #10766, #21306, #3410 ) ;
#972 = CIRCLE ( 'NONE', #14031, 13.00000000000001776 ) ;
#973 = CARTESIAN_POINT ( 'NONE',  ( -3.662846001189865142, 195.5725841191952838, 31.89886208192143613 ) ) ;
#974 = CARTESIAN_POINT ( 'NONE',  ( 8.062137200540822946, 212.9164362838583315, 39.69886208192143329 ) ) ;
#975 = CARTESIAN_POINT ( 'NONE',  ( 85.69999999453762030, 142.6655632788954620, -8.961492836873480528 ) ) ;
#976 = CARTESIAN_POINT ( 'NONE',  ( -11.98450388067348804, 210.9467285061362247, 81.65113791807856103 ) ) ;
#977 = CARTESIAN_POINT ( 'NONE',  ( 7.984503880673485376, 204.3529502787953902, 101.1511379180785895 ) ) ;
#978 = EDGE_CURVE ( 'NONE', #23779, #33225, #14441, .T. ) ;
#979 = CARTESIAN_POINT ( 'NONE',  ( 9.984503880673420539, 210.2968891136705167, 57.84886208192143897 ) ) ;
#980 = FACE_OUTER_BOUND ( 'NONE', #1402, .T. ) ;
#981 = AXIS2_PLACEMENT_3D ( 'NONE', #30181, #6671, #17224 ) ;
#982 = VERTEX_POINT ( 'NONE', #25338 ) ;
#983 = CARTESIAN_POINT ( 'NONE',  ( 3.662846001189864698, 218.4274158808046593, 57.39886208192143613 ) ) ;
#984 = EDGE_LOOP ( 'NONE', ( #28690, #5687, #6551, #10597 ) ) ;
#985 = CARTESIAN_POINT ( 'NONE',  ( 70.47499999726881015, 149.9369285172503510, 15.58253174999999580 ) ) ;
#986 = CARTESIAN_POINT ( 'NONE',  ( 7.984503880673422316, 209.6470497212048372, 36.84886208192142476 ) ) ;
#987 = EDGE_LOOP ( 'NONE', ( #4854, #13147, #24836, #25299, #30659 ) ) ;
#988 = ADVANCED_FACE ( 'NONE', ( #4564 ), #7120, .F. ) ;
#989 = CARTESIAN_POINT ( 'NONE',  ( 80.17499999726881299, 164.1591823560292198, 12.60653300113718167 ) ) ;
#990 = DIRECTION ( 'NONE',  ( -1.000000000000000000, -0.000000000000000000, -0.000000000000000000 ) ) ;
#991 = CARTESIAN_POINT ( 'NONE',  ( 5.000000000000000000, -2.342598717236903383, 4.057500000000001883 ) ) ;
#992 = CARTESIAN_POINT ( 'NONE',  ( -2.517493886308901807, 199.4062855549015012, 50.90113791807858235 ) ) ;
#993 = AXIS2_PLACEMENT_3D ( 'NONE', #19471, #32747, #14366 ) ;
#994 = SURFACE_STYLE_USAGE ( .BOTH. , #19219 ) ;
#995 = AXIS2_PLACEMENT_3D ( 'NONE', #7458, #17673, #4722 ) ;
#996 = CARTESIAN_POINT ( 'NONE',  ( 10.01549611932659545, 203.7984951890123853, 37.14886208192142192 ) ) ;
#997 = CARTESIAN_POINT ( 'NONE',  ( 70.77499999726880731, 140.1801316387863778, 4.815267126137185549 ) ) ;
#998 = ORIENTED_EDGE ( 'NONE', *, *, #28348, .F. ) ;
#999 = DIRECTION ( 'NONE',  ( 0.000000000000000000, 0.000000000000000000, 1.000000000000000000 ) ) ;
#1000 = EDGE_CURVE ( 'NONE', #5337, #6298, #8048, .T. ) ;
#1001 =( NAMED_UNIT ( * ) PLANE_ANGLE_UNIT ( ) SI_UNIT ( $, .RADIAN. ) );
#1002 = CARTESIAN_POINT ( 'NONE',  ( 99.17200000000002547, 0.000000000000000000, 5.000000000000000888 ) ) ;
#1003 = CYLINDRICAL_SURFACE ( 'NONE', #10395, 5.250000000000004441 ) ;
#1004 = CARTESIAN_POINT ( 'NONE',  ( 7.984503880673422316, 209.6470497212048372, 18.84886208192143187 ) ) ;
#1005 = CARTESIAN_POINT ( 'NONE',  ( -6.139770520408369237, 215.5359834540460042, 54.95113791807856529 ) ) ;
#1006 = CARTESIAN_POINT ( 'NONE',  ( 3.044812012440130555, 197.4746971517856764, 41.60113791807857808 ) ) ;
#1007 = CARTESIAN_POINT ( 'NONE',  ( 84.67499999726881299, 141.7447067706911810, 9.630534252274376428 ) ) ;
#1008 = AXIS2_PLACEMENT_3D ( 'NONE', #4742, #5084, #30817 ) ;
#1009 = CARTESIAN_POINT ( 'NONE',  ( -4.984841277089891776, 213.7757310962905990, 98.94886208192143329 ) ) ;
#1010 = CARTESIAN_POINT ( 'NONE',  ( 35.52499999726880731, 169.8198683612136222, -4.815267126137197984 ) ) ;
#1011 = CARTESIAN_POINT ( 'NONE',  ( 81.18867513459481700, 169.2658477444273331, -4.635254915624224203 ) ) ;
#1012 = CARTESIAN_POINT ( 'NONE',  ( 4.000000000000000000, 0.000000000000000000, 0.000000000000000000 ) ) ;
#1013 = CARTESIAN_POINT ( 'NONE',  ( -11.98450388067348804, 210.9467285061362247, 21.65113791807856813 ) ) ;
#1014 = CARTESIAN_POINT ( 'NONE',  ( 99.17200000000002547, 0.000000000000000000, 0.000000000000000000 ) ) ;
#1015 = EDGE_CURVE ( 'NONE', #20912, #20942, #22442, .T. ) ;
#1016 = CARTESIAN_POINT ( 'NONE',  ( -3.135527875058821579, 197.5041725223112223, 68.90113791807857524 ) ) ;
#1017 = ADVANCED_FACE ( 'NONE', ( #30283 ), #6949, .T. ) ;
#1018 = CARTESIAN_POINT ( 'NONE',  ( 3.044812012440130555, 197.4746971517856764, 41.60113791807857808 ) ) ;
#1019 = FACE_OUTER_BOUND ( 'NONE', #22833, .T. ) ;
#1020 = CARTESIAN_POINT ( 'NONE',  ( 2.249320974685019792, 30.45561873520115270, -16.29357272760982411 ) ) ;
#1021 = CARTESIAN_POINT ( 'NONE',  ( -3.753561863808878130, 218.3979405102790281, 6.098862081921433642 ) ) ;
#1022 = CARTESIAN_POINT ( 'NONE',  ( -10.00000000000000711, 206.9523078486584495, 11.49886208192143577 ) ) ;
#1023 = CARTESIAN_POINT ( 'NONE',  ( 66.99999999453761745, 155.0000000000000000, 14.49999999999999467 ) ) ;
#1024 = ORIENTED_EDGE ( 'NONE', *, *, #32635, .F. ) ;
#1025 = CARTESIAN_POINT ( 'NONE',  ( -3.662846001190052991, 218.4274158808045740, 46.10113791807857098 ) ) ;
#1026 = VECTOR ( 'NONE', #8266, 1000.000000000000000 ) ;
#1027 = CARTESIAN_POINT ( 'NONE',  ( 8.015496119326531499, 209.5516654185219636, 67.85113791807857808 ) ) ;
#1028 = EDGE_CURVE ( 'NONE', #8086, #25683, #17164, .T. ) ;
#1029 = LINE ( 'NONE', #22776, #23544 ) ;
#1030 = CARTESIAN_POINT ( 'NONE',  ( 8.118202686958138514, 201.1607312380088501, 28.29886208192143471 ) ) ;
#1031 = CARTESIAN_POINT ( 'NONE',  ( 45.01132485994281751, 142.2402378747194405, 9.270509831248432420 ) ) ;
#1032 = VERTEX_POINT ( 'NONE', #28244 ) ;
#1033 = AXIS2_PLACEMENT_3D ( 'NONE', #1708, #30335, #2058 ) ;
#1034 = CARTESIAN_POINT ( 'NONE',  ( -10.01549611932653860, 203.7984951890123284, 78.35113791807857808 ) ) ;
#1035 = ORIENTED_EDGE ( 'NONE', *, *, #13146, .F. ) ;
#1036 = CIRCLE ( 'NONE', #9747, 10.12668159690567649 ) ;
#1037 = FACE_OUTER_BOUND ( 'NONE', #7836, .T. ) ;
#1038 = CARTESIAN_POINT ( 'NONE',  ( -1.098735407079250326, -7.248058225758884809, -6.326622577870279152 ) ) ;
#1039 = EDGE_LOOP ( 'NONE', ( #23668, #1919 ) ) ;
#1040 = CARTESIAN_POINT ( 'NONE',  ( 4.984841277089725686, 213.7757310962907411, 19.55113791807856671 ) ) ;
#1041 = CARTESIAN_POINT ( 'NONE',  ( -60.91993774119386984, 194.9950632347986641, -0.6485596632537811157 ) ) ;
#1042 = CARTESIAN_POINT ( 'NONE',  ( 8.118202686958138514, 201.1607312380088501, 4.298862081921434708 ) ) ;
#1043 = CARTESIAN_POINT ( 'NONE',  ( 48.77499999726880731, 140.1801316387863778, 4.815267126137185549 ) ) ;
#1044 = VERTEX_POINT ( 'NONE', #2517 ) ;
#1045 = CARTESIAN_POINT ( 'NONE',  ( 54.42499999726881299, 141.7447067706911810, 9.630534252274376428 ) ) ;
#1046 = CARTESIAN_POINT ( 'NONE',  ( 89.50000000000002842, 155.0000000000000000, 0.000000000000000000 ) ) ;
#1047 = FACE_OUTER_BOUND ( 'NONE', #1653, .T. ) ;
#1048 = DIRECTION ( 'NONE',  ( 0.000000000000000000, 0.000000000000000000, 1.000000000000000000 ) ) ;
#1049 = CIRCLE ( 'NONE', #20059, 2.500000000000000000 ) ;
#1050 = CARTESIAN_POINT ( 'NONE',  ( -6.220909254589682469, 215.4770327129946850, 92.94886208192143329 ) ) ;
#1051 = CARTESIAN_POINT ( 'NONE',  ( 59.27499999726882152, 149.9369285172503510, -15.58253175000000823 ) ) ;
#1052 = CARTESIAN_POINT ( 'NONE',  ( -3.044812012440131443, 216.5253028482142952, 19.10113791807856742 ) ) ;
#1053 = CARTESIAN_POINT ( 'NONE',  ( 7.500000000000000888, 3.608439182435154269, -7.298562697733103732 ) ) ;
#1054 = EDGE_CURVE ( 'NONE', #14849, #9110, #2180, .T. ) ;
#1055 = ADVANCED_FACE ( 'NONE', ( #7461 ), #15286, .F. ) ;
#1056 = CARTESIAN_POINT ( 'NONE',  ( -12.01549611932659722, 210.8513442034533227, 77.64886208192143613 ) ) ;
#1057 = CARTESIAN_POINT ( 'NONE',  ( 73.59999999999999432, 150.2886644046228639, 14.49999999999999645 ) ) ;
#1058 = CARTESIAN_POINT ( 'NONE',  ( 64.88867513459483405, 159.8737954434937478, -14.99999999999993072 ) ) ;
#1059 = DIRECTION ( 'NONE',  ( 0.000000000000000000, 0.000000000000000000, -1.000000000000000000 ) ) ;
#1060 = CARTESIAN_POINT ( 'NONE',  ( -8.062137200540920645, 212.9164362838581894, 96.80113791807858092 ) ) ;
#1061 = CARTESIAN_POINT ( 'NONE',  ( 125.5000000000000000, 261.0000000000000000, -2.149999999999985256 ) ) ;
#1062 = CARTESIAN_POINT ( 'NONE',  ( 45.27499999726880020, 149.9369285172503510, -15.58253175000000823 ) ) ;
#1063 = EDGE_CURVE ( 'NONE', #15562, #30489, #11824, .T. ) ;
#1064 = CARTESIAN_POINT ( 'NONE',  ( -8.118202686958039038, 201.1607312380087080, 39.20113791807857240 ) ) ;
#1065 = CARTESIAN_POINT ( 'NONE',  ( 75.22499999726879594, 160.0630714827496206, -15.58253175000000823 ) ) ;
#1066 = ORIENTED_EDGE ( 'NONE', *, *, #8262, .F. ) ;
#1067 = DIRECTION ( 'NONE',  ( 0.5773502691896268413, -0.5773502691896268413, -0.5773502691896235106 ) ) ;
#1068 = CARTESIAN_POINT ( 'NONE',  ( 46.69999999453762740, 167.3344367211045096, 8.961492836873468093 ) ) ;
#1069 = CARTESIAN_POINT ( 'NONE',  ( 0.05014649552807549926, 219.6175466908591716, 16.25113791807856600 ) ) ;
#1070 = EDGE_CURVE ( 'NONE', #10890, #31219, #20910, .T. ) ;
#1071 = DIRECTION ( 'NONE',  ( -0.000000000000000000, -0.000000000000000000, -1.000000000000000000 ) ) ;
#1072 = CARTESIAN_POINT ( 'NONE',  ( 3.499999999999993339, -2.020725942163723143, -0.3126073911696551910 ) ) ;
#1073 = EDGE_LOOP ( 'NONE', ( #10094, #23123, #12443, #529 ) ) ;
#1074 = CARTESIAN_POINT ( 'NONE',  ( 9.680171189290716072, 214.0920067884432854, 33.69886208192142618 ) ) ;
#1075 = CARTESIAN_POINT ( 'NONE',  ( 65.24999999999998579, 7.347880794884118356E-15, -35.00000000000000000 ) ) ;
#1076 = CIRCLE ( 'NONE', #10334, 2.500000000000000000 ) ;
#1077 = CARTESIAN_POINT ( 'NONE',  ( -8.118202686958039038, 201.1607312380087080, 54.20113791807857240 ) ) ;
#1078 = EDGE_LOOP ( 'NONE', ( #2639, #30744, #24589, #33121 ) ) ;
#1079 = CARTESIAN_POINT ( 'NONE',  ( 7.984503880673422316, 209.6470497212048372, 15.84886208192143719 ) ) ;
#1080 = CARTESIAN_POINT ( 'NONE',  ( -14.33345751131668955, -23.47883925285270834, -17.99999999999999645 ) ) ;
#1081 = VERTEX_POINT ( 'NONE', #33517 ) ;
#1082 = CARTESIAN_POINT ( 'NONE',  ( 8.000000000000008882, 207.0476921513415220, 102.9988620819214304 ) ) ;
#1083 = CARTESIAN_POINT ( 'NONE',  ( 0.05014649552807626948, 215.4116977939061144, 43.25113791807856956 ) ) ;
#1084 = DIRECTION ( 'NONE',  ( -1.000000000000000000, 0.000000000000000000, 0.000000000000000000 ) ) ;
#1085 = ORIENTED_EDGE ( 'NONE', *, *, #22443, .T. ) ;
#1086 = CARTESIAN_POINT ( 'NONE',  ( 37.12499999726881583, 155.0000000000000000, -15.58253175000000823 ) ) ;
#1087 =( BOUNDED_CURVE ( )  B_SPLINE_CURVE ( 2, ( #26892, #27390, #29787, #3549, #18445, #26273, #6096, #6453, #1339, #13942, #32335 ),
 .UNSPECIFIED., .F., .F. ) 
 B_SPLINE_CURVE_WITH_KNOTS ( ( 3, 2, 2, 2, 2, 3 ),
 ( 0.6249999999999996669, 0.6285714285714282257, 0.6321428571428568954, 0.6357142857142854542, 0.6392857142857141239, 0.6428571428571426827 ),
 .UNSPECIFIED. ) 
 CURVE ( )  GEOMETRIC_REPRESENTATION_ITEM ( )  RATIONAL_B_SPLINE_CURVE ( ( 1.000000000000004663, 0.9510565162951488682, 1.000000000000000000, 0.9510565162951534202, 1.000000000000000000, 0.9510565162951534202, 1.000000000000000000, 0.9510565162951534202, 1.000000000000000000, 0.9510565162951549745, 0.9999999999999984457 ) ) 
 REPRESENTATION_ITEM ( '' )  );
#1088 = CARTESIAN_POINT ( 'NONE',  ( -3.135527875058982783, 216.4958274776886924, 63.09886208192143187 ) ) ;
#1089 = CARTESIAN_POINT ( 'NONE',  ( 42.87499999726881583, 138.6155565068815463, -3.929120461958505118E-15 ) ) ;
#1090 = CARTESIAN_POINT ( 'NONE',  ( 0.000000000000000000, 0.000000000000000000, -2.899999999999999911 ) ) ;
#1091 = CARTESIAN_POINT ( 'NONE',  ( 2.426778023690261410, 199.3768101843759837, 98.60113791807857808 ) ) ;
#1092 = CARTESIAN_POINT ( 'NONE',  ( 56.59999999999999432, 159.7113355953771077, -14.50000000000000888 ) ) ;
#1093 = CARTESIAN_POINT ( 'NONE',  ( -5.357619327558936585E-16, 7.505553499465137612, -6.064240316920400886 ) ) ;
#1094 = ADVANCED_BREP_SHAPE_REPRESENTATION ( '', ( #23982, #2404 ), #31228 ) ;
#1095 = CARTESIAN_POINT ( 'NONE',  ( -8.000000000000008882, 206.9523078486584780, 74.49886208192144466 ) ) ;
#1096 = CARTESIAN_POINT ( 'NONE',  ( 54.71132485994280614, 155.0000000000000000, 15.00000000000001243 ) ) ;
#1097 = CARTESIAN_POINT ( 'NONE',  ( -0.3755270751584372513, 206.7692714347155629, 108.3323677711371573 ) ) ;
#1098 = CARTESIAN_POINT ( 'NONE',  ( 58.02499999726880731, 160.0630714827496206, 15.58253174999999402 ) ) ;
#1099 = CARTESIAN_POINT ( 'NONE',  ( -6.220909254589537696, 198.5229672870051445, 9.051137918078566713 ) ) ;
#1100 = LINE ( 'NONE', #11492, #1026 ) ;
#1101 = CARTESIAN_POINT ( 'NONE',  ( 67.62499999726881583, 171.3844434931184253, -7.942151717890134290E-15 ) ) ;
#1102 = CARTESIAN_POINT ( 'NONE',  ( 73.57499999726880446, 164.1591823560292198, -12.60653300113719766 ) ) ;
#1103 = CARTESIAN_POINT ( 'NONE',  ( 12.00000000000000711, 206.9523078486586485, 77.00113791807858377 ) ) ;
#1104 = CARTESIAN_POINT ( 'NONE',  ( 6.220909254589536808, 215.4770327129947987, 94.55113791807858092 ) ) ;
#1105 = CARTESIAN_POINT ( 'NONE',  ( 0.000000000000000000, 0.000000000000000000, -18.00000000000000000 ) ) ;
#1106 = EDGE_LOOP ( 'NONE', ( #29137, #28238, #18476, #24027 ) ) ;
#1107 = CARTESIAN_POINT ( 'NONE',  ( 9.680171189290716072, 214.0920067884432854, 102.6988620819214475 ) ) ;
#1108 = CARTESIAN_POINT ( 'NONE',  ( 0.05014649552828288198, 194.3824533091408000, 61.74886208192143755 ) ) ;
#1109 = CARTESIAN_POINT ( 'NONE',  ( -6.220909254589682469, 215.4770327129947134, 68.94886208192143329 ) ) ;
#1110 = CARTESIAN_POINT ( 'NONE',  ( 12.00000000000000711, 207.0476921513415220, 6.998862081921433997 ) ) ;
#1111 = CARTESIAN_POINT ( 'NONE',  ( -4.358513833876417998, -4.989164364209884184, -0.07763482564821273801 ) ) ;
#1112 = CARTESIAN_POINT ( 'NONE',  ( -8.062137200540920645, 212.9164362838581894, 27.80113791807856671 ) ) ;
#1113 = CARTESIAN_POINT ( 'NONE',  ( 8.062137200540822946, 212.9164362838583315, 87.69886208192144750 ) ) ;
#1114 = ORIENTED_EDGE ( 'NONE', *, *, #11237, .F. ) ;
#1115 = LINE ( 'NONE', #21550, #33373 ) ;
#1116 = ORIENTED_EDGE ( 'NONE', *, *, #8477, .T. ) ;
#1117 = CARTESIAN_POINT ( 'NONE',  ( 27.50000000000000355, 15.87713240271469317, -18.00000000000000000 ) ) ;
#1118 = CARTESIAN_POINT ( 'NONE',  ( -4.903702542908436435, 200.1653181626580249, 74.04886208192142760 ) ) ;
#1119 = ORIENTED_EDGE ( 'NONE', *, *, #227, .T. ) ;
#1120 = PRODUCT_DEFINITION_SHAPE ( 'NONE', 'NONE',  #33701 ) ;
#1121 = CARTESIAN_POINT ( 'NONE',  ( 86.82499999726879025, 141.7447067706911810, -9.630534252274387086 ) ) ;
#1122 = EDGE_LOOP ( 'NONE', ( #25752, #2521, #18480, #9209 ) ) ;
#1123 = CARTESIAN_POINT ( 'NONE',  ( 68.78867513459482552, 155.0000000000000000, -15.00000000000002487 ) ) ;
#1124 = CARTESIAN_POINT ( 'NONE',  ( 76.72499999726881015, 140.1801316387863778, -4.815267126137194431 ) ) ;
#1125 = CARTESIAN_POINT ( 'NONE',  ( -6.500168698208129925, 202.3363017425936050, 69.20113791807857240 ) ) ;
#1126 = CARTESIAN_POINT ( 'NONE',  ( 74.88867513459483405, 159.8737954434939184, -14.99999999999981704 ) ) ;
#1127 = FACE_OUTER_BOUND ( 'NONE', #9365, .T. ) ;
#1128 = CARTESIAN_POINT ( 'NONE',  ( 8.000000000000008882, 207.0476921513415220, 42.99886208192143755 ) ) ;
#1129 = CARTESIAN_POINT ( 'NONE',  ( 0.05014649552810505201, 217.5146222423826714, 91.25113791807858377 ) ) ;
#1130 = CARTESIAN_POINT ( 'NONE',  ( -10.01549611932653860, 203.7984951890123284, 69.35113791807857808 ) ) ;
#1131 = CARTESIAN_POINT ( 'NONE',  ( 7.922281120364393914, -4.573931137438282057, -8.047472243342932430 ) ) ;
#1132 = CARTESIAN_POINT ( 'NONE',  ( -8.015496119326531499, 204.4483345814780364, 24.35113791807856742 ) ) ;
#1133 = FACE_OUTER_BOUND ( 'NONE', #17035, .T. ) ;
#1134 = CARTESIAN_POINT ( 'NONE',  ( 117.5000000000000142, 155.0000000000000000, 98.00000000000000000 ) ) ;
#1135 = CARTESIAN_POINT ( 'NONE',  ( 50.22499999726881015, 149.9369285172503510, 15.58253174999999580 ) ) ;
#1136 = CARTESIAN_POINT ( 'NONE',  ( -3.662846001190052991, 218.4274158808045740, 49.10113791807857808 ) ) ;
#1137 = CARTESIAN_POINT ( 'NONE',  ( 125.0000000000000000, 3.061616997868383121E-14, -35.00000000000000000 ) ) ;
#1138 = CARTESIAN_POINT ( 'NONE',  ( 3.135527875058820690, 216.4958274776887492, 94.40113791807857524 ) ) ;
#1139 = EDGE_CURVE ( 'NONE', #15105, #26666, #12565, .T. ) ;
#1140 = CARTESIAN_POINT ( 'NONE',  ( 8.062137200540920645, 201.0835637161417822, 65.30113791807858092 ) ) ;
#1141 = CARTESIAN_POINT ( 'NONE',  ( 7.456977232089471386, 196.8216656703012006, 28.44886208192142973 ) ) ;
#1142 = CARTESIAN_POINT ( 'NONE',  ( 0.05014649552828275014, 196.4853777576173002, 37.74886208192144466 ) ) ;
#1143 = CARTESIAN_POINT ( 'NONE',  ( 83.79999999453762882, 146.4771138417591203, -11.73074641843674470 ) ) ;
#1144 = CARTESIAN_POINT ( 'NONE',  ( -3.662846001190052991, 218.4274158808045740, 82.10113791807857808 ) ) ;
#1145 = CARTESIAN_POINT ( 'NONE',  ( 6.444103211791042618, 202.2591342207267644, 98.30113791807858092 ) ) ;
#1146 = CARTESIAN_POINT ( 'NONE',  ( -8.062137200540822946, 201.0835637161416400, 62.19886208192143329 ) ) ;
#1147 = DIRECTION ( 'NONE',  ( 0.000000000000000000, -0.5000000000000014433, -0.8660254037844379305 ) ) ;
#1148 = VERTEX_POINT ( 'NONE', #15462 ) ;
#1149 = CARTESIAN_POINT ( 'NONE',  ( 9.736236675708031640, 199.9851607334238963, 64.29886208192144181 ) ) ;
#1150 = VECTOR ( 'NONE', #31313, 1000.000000000000000 ) ;
#1151 = EDGE_LOOP ( 'NONE', ( #25557, #15743, #24197, #1200, #10854, #1528 ) ) ;
#1152 = CARTESIAN_POINT ( 'NONE',  ( 73.67499999726878457, 168.2552932293087906, -9.630534252274385310 ) ) ;
#1153 = CARTESIAN_POINT ( 'NONE',  ( -7.984503880673422316, 204.3529502787951628, 41.34886208192143897 ) ) ;
#1154 = ORIENTED_EDGE ( 'NONE', *, *, #19289, .T. ) ;
#1155 = CARTESIAN_POINT ( 'NONE',  ( 85.87499999726881583, 171.3844434931184253, -7.942151717890134290E-15 ) ) ;
#1156 = DIRECTION ( 'NONE',  ( -1.000000000000000000, 0.000000000000000000, 0.000000000000000000 ) ) ;
#1157 = DIRECTION ( 'NONE',  ( 0.000000000000000000, 0.000000000000000000, -1.000000000000000000 ) ) ;
#1158 = CARTESIAN_POINT ( 'NONE',  ( -8.000000000000008882, 207.0476921513413515, 54.50113791807857666 ) ) ;
#1159 = CARTESIAN_POINT ( 'NONE',  ( 10.00000000000000711, 207.0476921513415220, 33.99886208192143044 ) ) ;
#1160 = CARTESIAN_POINT ( 'NONE',  ( 69.67499999726879878, 168.2552932293087906, -9.630534252274387086 ) ) ;
#1161 = ORIENTED_EDGE ( 'NONE', *, *, #624, .T. ) ;
#1162 = CARTESIAN_POINT ( 'NONE',  ( 41.28867513459482552, 170.7719333635740497, -7.904646289410545231E-15 ) ) ;
#1163 = DIRECTION ( 'NONE',  ( 0.000000000000000000, 1.000000000000000000, -1.222984857324291014E-15 ) ) ;
#1164 = DIRECTION ( 'NONE',  ( 0.000000000000000000, 0.000000000000000000, -1.000000000000000000 ) ) ;
#1165 = CARTESIAN_POINT ( 'NONE',  ( 8.015496119326595448, 204.4483345814782638, 16.14886208192143968 ) ) ;
#1166 = CARTESIAN_POINT ( 'NONE',  ( 8.062137200540920645, 201.0835637161417822, 59.30113791807857382 ) ) ;
#1167 = CARTESIAN_POINT ( 'NONE',  ( -9.984503880673473830, 210.2968891136704315, 39.65113791807857524 ) ) ;
#1168 = CARTESIAN_POINT ( 'NONE',  ( 88.17499999726881299, 164.1591823560292198, 12.60653300113718167 ) ) ;
#1169 = VECTOR ( 'NONE', #26440, 1000.000000000000000 ) ;
#1170 = CARTESIAN_POINT ( 'NONE',  ( 2.517493886309087436, 199.4062855549015865, 103.5988620819214532 ) ) ;
#1171 = CARTESIAN_POINT ( 'NONE',  ( 46.02499999726880731, 160.0630714827496206, 15.58253174999999402 ) ) ;
#1172 = FACE_OUTER_BOUND ( 'NONE', #23032, .T. ) ;
#1173 = CARTESIAN_POINT ( 'NONE',  ( 7.375838497908181246, 196.7627149292499666, 23.45113791807856884 ) ) ;
#1174 = CARTESIAN_POINT ( 'NONE',  ( -0.5204879950542059541, -7.205049615410630715, -0.5609245978742286587 ) ) ;
#1175 = CARTESIAN_POINT ( 'NONE',  ( 0.05014649552810505201, 217.5146222423826714, 67.25113791807856956 ) ) ;
#1176 = EDGE_CURVE ( 'NONE', #2927, #16155, #28150, .T. ) ;
#1177 = CARTESIAN_POINT ( 'NONE',  ( 9.984503880673473830, 203.7031108863295401, 44.15113791807856813 ) ) ;
#1178 = DIRECTION ( 'NONE',  ( -0.000000000000000000, -0.000000000000000000, 1.000000000000000000 ) ) ;
#1179 = CARTESIAN_POINT ( 'NONE',  ( -3.214438021527937117, -2.185595227304884425, -2.682579934988229997 ) ) ;
#1180 = CARTESIAN_POINT ( 'NONE',  ( 7.456977232089471386, 196.8216656703012006, 7.448862081921435951 ) ) ;
#1181 = CARTESIAN_POINT ( 'NONE',  ( -3.135527875058982783, 216.4958274776886924, 12.09886208192143542 ) ) ;
#1182 = CARTESIAN_POINT ( 'NONE',  ( 68.99999999453763166, 155.0000000000000000, 14.49999999999999467 ) ) ;
#1183 = EDGE_LOOP ( 'NONE', ( #6771, #131, #30193, #14259, #7403, #30165 ) ) ;
#1184 = CARTESIAN_POINT ( 'NONE',  ( -12.01549611932652972, 203.1486557965464499, 51.35113791807857098 ) ) ;
#1185 = CARTESIAN_POINT ( 'NONE',  ( -4.984841277089726574, 200.2242689037092305, 66.05113791807858092 ) ) ;
#1186 = DIRECTION ( 'NONE',  ( -0.1045284632676468234, 1.217938055844715641E-16, -0.9945218953682740670 ) ) ;
#1187 = CARTESIAN_POINT ( 'NONE',  ( 6.220909254589681581, 198.5229672870052582, 28.44886208192143684 ) ) ;
#1188 = ORIENTED_EDGE ( 'NONE', *, *, #27275, .F. ) ;
#1189 = ADVANCED_FACE ( 'NONE', ( #30983 ), #30977, .F. ) ;
#1190 = CARTESIAN_POINT ( 'NONE',  ( -10.01549611932653860, 203.7984951890123284, 81.35113791807857808 ) ) ;
#1191 = ORIENTED_EDGE ( 'NONE', *, *, #15216, .F. ) ;
#1192 = CARTESIAN_POINT ( 'NONE',  ( -64.50000000000000000, 2.605762844159070557, -20.00000000000000000 ) ) ;
#1193 = DIRECTION ( 'NONE',  ( 5.620504062164857944E-16, -0.9988620819214347746, 0.04769215134146256169 ) ) ;
#1194 = EDGE_LOOP ( 'NONE', ( #3412, #16477, #22110, #1374, #13596 ) ) ;
#1195 = CARTESIAN_POINT ( 'NONE',  ( 2.426778023690261410, 199.3768101843759837, 26.60113791807856742 ) ) ;
#1196 = ADVANCED_FACE ( 'NONE', ( #25855 ), #12953, .T. ) ;
#1197 = CARTESIAN_POINT ( 'NONE',  ( 127.5000000000000000, 78.52640161467446944, -73.43303922622258995 ) ) ;
#1198 = CARTESIAN_POINT ( 'NONE',  ( 10.01549611932659545, 203.7984951890123853, 4.148862081921434353 ) ) ;
#1199 = CARTESIAN_POINT ( 'NONE',  ( 50.07499999726881157, 168.2552932293087906, 9.630534252274372875 ) ) ;
#1200 = ORIENTED_EDGE ( 'NONE', *, *, #19971, .T. ) ;
#1201 = CARTESIAN_POINT ( 'NONE',  ( 54.52499999726881441, 140.1801316387863778, 4.815267126137185549 ) ) ;
#1202 = CARTESIAN_POINT ( 'NONE',  ( 6.444103211791042618, 202.2591342207267644, 47.30113791807858092 ) ) ;
#1203 = DIRECTION ( 'NONE',  ( 1.000000000000000000, 0.000000000000000000, 0.000000000000000000 ) ) ;
#1204 = CIRCLE ( 'NONE', #21871, 32.10452846326769816 ) ;
#1205 = PRESENTATION_STYLE_ASSIGNMENT (( #14154 ) ) ;
#1206 = DIRECTION ( 'NONE',  ( 0.000000000000000000, 0.4999999999999990563, -0.8660254037844391517 ) ) ;
#1207 = CARTESIAN_POINT ( 'NONE',  ( 8.062137200540822946, 212.9164362838583315, 90.69886208192143329 ) ) ;
#1208 = ADVANCED_FACE ( 'NONE', ( #129 ), #14425, .F. ) ;
#1209 = VECTOR ( 'NONE', #26616, 1000.000000000000000 ) ;
#1210 = CARTESIAN_POINT ( 'NONE',  ( 62.67499999726879878, 141.7447067706911810, 9.630534252274376428 ) ) ;
#1211 = CARTESIAN_POINT ( 'NONE',  ( 8.118202686958039038, 212.8392687619912635, 19.70113791807856884 ) ) ;
#1212 = CARTESIAN_POINT ( 'NONE',  ( 7.500000000000000000, -3.608439182435168036, -7.298562697733107285 ) ) ;
#1213 = CARTESIAN_POINT ( 'NONE',  ( 3.753561863808876797, 195.6020594897209719, 82.59886208192143897 ) ) ;
#1214 = CARTESIAN_POINT ( 'NONE',  ( 81.30000000000001137, 163.5228861582408797, 11.73074641843673049 ) ) ;
#1215 = CARTESIAN_POINT ( 'NONE',  ( 39.98867513459482126, 146.1832212156128890, 12.13525491562421976 ) ) ;
#1216 = DIRECTION ( 'NONE',  ( -0.1045284632676468234, 1.217938055844715641E-16, -0.9945218953682740670 ) ) ;
#1217 = CARTESIAN_POINT ( 'NONE',  ( 0.05014649552810505201, 217.5146222423826714, 97.25113791807854113 ) ) ;
#1218 = CARTESIAN_POINT ( 'NONE',  ( 27.50000000000001066, -2.682974265912535294, -18.00000000000000355 ) ) ;
#1219 = CARTESIAN_POINT ( 'NONE',  ( 47.57499999726881867, 164.1591823560292198, -12.60653300113719766 ) ) ;
#1220 = CARTESIAN_POINT ( 'NONE',  ( 9.984503880673470277, 203.7031108863295401, 35.15113791807856813 ) ) ;
#1221 = B_SPLINE_CURVE_WITH_KNOTS ( 'NONE', 3,
 ( #24822, #19875, #11540, #6432, #4039, #6078, #21925, #16476, #22095, #32146 ),
 .UNSPECIFIED., .F., .F.,
 ( 4, 2, 2, 2, 4 ),
 ( 1.572453990175171705E-19, 0.002305503304226491201, 0.004611006608452982401, 0.006916509912679473168, 0.009222013216905964803 ),
 .UNSPECIFIED. ) ;
#1222 = CARTESIAN_POINT ( 'NONE',  ( 79.32499999726881867, 164.1591823560292198, -12.60653300113719766 ) ) ;
#1223 = ORIENTED_EDGE ( 'NONE', *, *, #17026, .F. ) ;
#1224 = AXIS2_PLACEMENT_3D ( 'NONE', #13530, #23921, #21197 ) ;
#1225 = LINE ( 'NONE', #11455, #20091 ) ;
#1226 = LINE ( 'NONE', #11624, #13011 ) ;
#1227 = CARTESIAN_POINT ( 'NONE',  ( 48.59999999453763309, 168.7903194862797420, 4.480746418436729606 ) ) ;
#1228 = CARTESIAN_POINT ( 'NONE',  ( -9.736236675707914401, 199.9851607334237542, 21.20113791807856529 ) ) ;
#1229 = DIRECTION ( 'NONE',  ( 0.000000000000000000, 0.000000000000000000, 1.000000000000000000 ) ) ;
#1230 = CARTESIAN_POINT ( 'NONE',  ( 115.4999999999999858, 51.09158283380785548, 28.95509836041905771 ) ) ;
#1231 = ORIENTED_EDGE ( 'NONE', *, *, #33099, .T. ) ;
#1232 = MANIFOLD_SOLID_BREP ( 'CirPattern1', #28098 ) ;
#1233 = CARTESIAN_POINT ( 'NONE',  ( -7.375838497908014268, 196.7627149292498530, 47.04886208192144181 ) ) ;
#1234 = CARTESIAN_POINT ( 'NONE',  ( 6.500000000000000000, -0.6456425506958747285, 7.487771253728014997E-16 ) ) ;
#1235 = CARTESIAN_POINT ( 'NONE',  ( 9.984503880673470277, 203.7031108863295401, 50.15113791807855392 ) ) ;
#1236 = VECTOR ( 'NONE', #1186, 1000.000000000000000 ) ;
#1237 = CARTESIAN_POINT ( 'NONE',  ( -8.015496119326597224, 209.5516654185217362, 14.64886208192143258 ) ) ;
#1238 = EDGE_CURVE ( 'NONE', #29217, #23382, #10861, .T. ) ;
#1239 = EDGE_CURVE ( 'NONE', #23379, #18472, #26181, .T. ) ;
#1240 = UNCERTAINTY_MEASURE_WITH_UNIT (LENGTH_MEASURE( 1.000000000000000082E-05 ), #4525, 'distance_accuracy_value', 'NONE');
#1241 = CARTESIAN_POINT ( 'NONE',  ( 51.51132485994281041, 146.1832212156128890, -12.13525491562423042 ) ) ;
#1242 = ORIENTED_EDGE ( 'NONE', *, *, #12526, .T. ) ;
#1243 = CARTESIAN_POINT ( 'NONE',  ( 2.426778023690075337, 214.6231898156240447, 96.39886208192146455 ) ) ;
#1244 = ADVANCED_FACE ( 'NONE', ( #29075, #31630 ), #29240, .T. ) ;
#1245 = DIRECTION ( 'NONE',  ( 1.000000000000000000, 0.000000000000000000, 0.000000000000000000 ) ) ;
#1246 = CARTESIAN_POINT ( 'NONE',  ( 2.426778023690261410, 199.3768101843759837, 44.60113791807857098 ) ) ;
#1247 = CARTESIAN_POINT ( 'NONE',  ( 99.99999999999998579, 0.000000000000000000, 0.000000000000000000 ) ) ;
#1248 = ORIENTED_EDGE ( 'NONE', *, *, #24308, .T. ) ;
#1249 = CARTESIAN_POINT ( 'NONE',  ( 41.12499999726880873, 155.0000000000000000, -15.58253175000000823 ) ) ;
#1250 = DIRECTION ( 'NONE',  ( 1.000000000000000000, 0.000000000000000000, 0.000000000000000000 ) ) ;
#1251 = AXIS2_PLACEMENT_3D ( 'NONE', #4410, #33022, #24855 ) ;
#1252 = CARTESIAN_POINT ( 'NONE',  ( 10.01549611932659545, 203.7984951890123853, 61.14886208192144323 ) ) ;
#1253 = ADVANCED_FACE ( 'NONE', ( #13725 ), #13394, .T. ) ;
#1254 = CARTESIAN_POINT ( 'NONE',  ( 41.77499999726881441, 169.8198683612136222, -4.815267126137197984 ) ) ;
#1255 = CARTESIAN_POINT ( 'NONE',  ( 99.30625411593993590, 155.0000000000000000, 0.000000000000000000 ) ) ;
#1256 = CARTESIAN_POINT ( 'NONE',  ( -8.015496119326531499, 204.4483345814780364, 99.35113791807857808 ) ) ;
#1257 = PRODUCT ( 'Internal Hydraulic Release Piston', 'Internal Hydraulic Release Piston', '', ( #26899 ) ) ;
#1258 = CONICAL_SURFACE ( 'NONE', #22487, 27.50000000000000355, 1.047197551196595411 ) ;
#1259 = CARTESIAN_POINT ( 'NONE',  ( 53.10000000000000142, 168.7903194862797420, 4.480746418436729606 ) ) ;
#1260 = CARTESIAN_POINT ( 'NONE',  ( 63.38867513459482694, 169.2658477444273331, 4.635254915624208216 ) ) ;
#1261 = CARTESIAN_POINT ( 'NONE',  ( 8.000000000000008882, 207.0476921513415220, 81.99886208192144466 ) ) ;
#1262 = CARTESIAN_POINT ( 'NONE',  ( -4.555432764205793461, 5.242992371775927474, -6.208169345099788572 ) ) ;
#1263 = AXIS2_PLACEMENT_3D ( 'NONE', #30747, #23072, #15236 ) ;
#1264 = LINE ( 'NONE', #22553, #33601 ) ;
#1265 = AXIS2_PLACEMENT_3D ( 'NONE', #21852, #8910, #19303 ) ;
#1266 = CARTESIAN_POINT ( 'NONE',  ( 59.62499999726882294, 171.3844434931184253, -7.942151717890132712E-15 ) ) ;
#1268 = ORIENTED_EDGE ( 'NONE', *, *, #4948, .F. ) ;
#1267 = CARTESIAN_POINT ( 'NONE',  ( 10.00000000000000711, 206.9523078486586201, 20.00113791807856600 ) ) ;
#1269 = CARTESIAN_POINT ( 'NONE',  ( 43.21132485994281325, 139.2280666364260071, -4.041636747397287284E-15 ) ) ;
#1270 = CARTESIAN_POINT ( 'NONE',  ( 81.57499999726880446, 164.1591823560292198, -12.60653300113719766 ) ) ;
#1271 = CARTESIAN_POINT ( 'NONE',  ( -9.680171189290831535, 214.0920067884431148, 84.80113791807858092 ) ) ;
#1272 = CARTESIAN_POINT ( 'NONE',  ( 1.750000000000016209, -3.031088913245524985, -2.899999999999999911 ) ) ;
#1273 = FACE_OUTER_BOUND ( 'NONE', #22824, .T. ) ;
#1274 = ORIENTED_EDGE ( 'NONE', *, *, #15983, .F. ) ;
#1275 = CARTESIAN_POINT ( 'NONE',  ( 3.753561863808876797, 195.6020594897209719, 58.59886208192143897 ) ) ;
#1276 = CIRCLE ( 'NONE', #741, 2.149999999999985256 ) ;
#1277 = CARTESIAN_POINT ( 'NONE',  ( -6.220909254589682469, 215.4770327129947134, 71.94886208192144750 ) ) ;
#1278 = CARTESIAN_POINT ( 'NONE',  ( -12.01549611932659722, 210.8513442034533227, 11.64886208192143613 ) ) ;
#1279 = DIRECTION ( 'NONE',  ( -1.000000000000000000, -0.000000000000000000, -0.000000000000000000 ) ) ;
#1280 = CARTESIAN_POINT ( 'NONE',  ( -10.00000000000000711, 207.0476921513413515, 21.50113791807856956 ) ) ;
#1281 = CARTESIAN_POINT ( 'NONE',  ( 9.984503880673420539, 210.2968891136705167, 87.84886208192141055 ) ) ;
#1282 = EDGE_CURVE ( 'NONE', #22150, #13858, #18398, .T. ) ;
#1283 = ORIENTED_EDGE ( 'NONE', *, *, #598, .T. ) ;
#1284 = LINE ( 'NONE', #32113, #20847 ) ;
#1285 =( GEOMETRIC_REPRESENTATION_CONTEXT ( 3 ) GLOBAL_UNCERTAINTY_ASSIGNED_CONTEXT ( ( #28742 ) ) GLOBAL_UNIT_ASSIGNED_CONTEXT ( ( #21117, #12788, #28297 ) ) REPRESENTATION_CONTEXT ( 'NONE', 'WORKASPACE' ) );
#1286 = ORIENTED_EDGE ( 'NONE', *, *, #8935, .F. ) ;
#1287 = CARTESIAN_POINT ( 'NONE',  ( 4.000000000000000000, 0.000000000000000000, -8.000000000000000000 ) ) ;
#1288 = CARTESIAN_POINT ( 'NONE',  ( -8.000000000000008882, 206.9523078486584780, 71.49886208192144466 ) ) ;
#1289 = SHAPE_REPRESENTATION ( 'socket head cap screw_iso_ISO 4762 M10 x 90 - 32N', ( #2404 ), #25772 ) ;
#1290 = AXIS2_PLACEMENT_3D ( 'NONE', #17289, #33134, #30578 ) ;
#1291 = VERTEX_POINT ( 'NONE', #14067 ) ;
#1292 = EDGE_CURVE ( 'NONE', #9623, #30416, #28733, .T. ) ;
#1293 = CARTESIAN_POINT ( 'NONE',  ( 82.52499999726880731, 140.1801316387863778, 4.815267126137185549 ) ) ;
#1294 = ORIENTED_EDGE ( 'NONE', *, *, #3214, .F. ) ;
#1295 = CARTESIAN_POINT ( 'NONE',  ( 68.91132485994280898, 146.1832212156128890, 12.13525491562421976 ) ) ;
#1296 = MANIFOLD_SOLID_BREP ( 'Fillet2', #22105 ) ;
#1297 = CARTESIAN_POINT ( 'NONE',  ( 79.42499999726881299, 168.2552932293087906, -9.630534252274385310 ) ) ;
#1298 = CARTESIAN_POINT ( 'NONE',  ( 18.40606158072673537, -21.12752019707603779, -17.76591125084755163 ) ) ;
#1299 = CARTESIAN_POINT ( 'NONE',  ( -2.517493886308901807, 199.4062855549015012, 65.90113791807856103 ) ) ;
#1300 = LINE ( 'NONE', #25129, #6401 ) ;
#1301 = CIRCLE ( 'NONE', #14892, 2.000000000000000888 ) ;
#1302 = PRESENTATION_STYLE_ASSIGNMENT (( #24286 ) ) ;
#1303 = CARTESIAN_POINT ( 'NONE',  ( 33.80000000000000426, 142.6655632788954620, 8.961492836873471646 ) ) ;
#1304 = CARTESIAN_POINT ( 'NONE',  ( -7.984503880673422316, 204.3529502787951628, 44.34886208192144608 ) ) ;
#1305 = CARTESIAN_POINT ( 'NONE',  ( -0.05014649552810635652, 196.4853777576173002, 74.75113791807858377 ) ) ;
#1306 = DIRECTION ( 'NONE',  ( 0.000000000000000000, 0.000000000000000000, -1.000000000000000000 ) ) ;
#1307 = CARTESIAN_POINT ( 'NONE',  ( 73.61132485994279762, 150.1262045565062806, -14.99999999999993072 ) ) ;
#1308 = CIRCLE ( 'NONE', #24706, 2.000000000000000888 ) ;
#1309 = DIRECTION ( 'NONE',  ( 0.000000000000000000, 0.000000000000000000, -1.000000000000000000 ) ) ;
#1310 = CARTESIAN_POINT ( 'NONE',  ( 51.02499999726880731, 149.9369285172503510, -15.58253175000000823 ) ) ;
#1311 = CARTESIAN_POINT ( 'NONE',  ( 12.00000000000000711, 206.9523078486586485, 53.00113791807857666 ) ) ;
#1312 = CARTESIAN_POINT ( 'NONE',  ( -119.7500000000000000, -6.429395695523609083E-16, 35.00000599999999906 ) ) ;
#1313 = AXIS2_PLACEMENT_3D ( 'NONE', #10723, #17889, #4937 ) ;
#1314 = CARTESIAN_POINT ( 'NONE',  ( -6.139770520408369237, 215.5359834540460042, 99.95113791807855819 ) ) ;
#1315 = CARTESIAN_POINT ( 'NONE',  ( 9.984503880673473830, 203.7031108863295401, 65.15113791807856103 ) ) ;
#1316 = CARTESIAN_POINT ( 'NONE',  ( -12.00000000000000711, 206.9523078486584780, 32.49886208192143044 ) ) ;
#1317 = CARTESIAN_POINT ( 'NONE',  ( 3.044812012439969795, 216.5253028482143520, 51.39886208192143613 ) ) ;
#1318 = CARTESIAN_POINT ( 'NONE',  ( 83.29999999453764303, 142.6655632788954620, 8.961492836873471646 ) ) ;
#1319 = CARTESIAN_POINT ( 'NONE',  ( -0.05014649552807705357, 194.3824533091408000, 80.75113791807856956 ) ) ;
#1320 = CARTESIAN_POINT ( 'NONE',  ( -0.05014649552807731031, 198.5883022060938572, 95.75113791807856956 ) ) ;
#1321 = CARTESIAN_POINT ( 'NONE',  ( 8.118202686958138514, 201.1607312380088501, 61.29886208192143471 ) ) ;
#1322 = SURFACE_STYLE_FILL_AREA ( #6767 ) ;
#1323 = ORIENTED_EDGE ( 'NONE', *, *, #11989, .F. ) ;
#1324 = CARTESIAN_POINT ( 'NONE',  ( 7.456977232089471386, 196.8216656703012006, 61.44886208192143329 ) ) ;
#1325 = EDGE_LOOP ( 'NONE', ( #5593, #15241, #7416, #14552 ) ) ;
#1326 = CARTESIAN_POINT ( 'NONE',  ( 72.47499999726878173, 149.9369285172503510, 15.58253174999999580 ) ) ;
#1327 = CARTESIAN_POINT ( 'NONE',  ( 8.015496119326595448, 204.4483345814782638, 46.14886208192143613 ) ) ;
#1328 = VERTEX_POINT ( 'NONE', #26846 ) ;
#1329 = CARTESIAN_POINT ( 'NONE',  ( 82.47499999726879594, 149.9369285172503510, 15.58253174999999580 ) ) ;
#1330 = CARTESIAN_POINT ( 'NONE',  ( -1.750000000000014211, 3.031088913245526317, -2.899999999999999911 ) ) ;
#1331 = CARTESIAN_POINT ( 'NONE',  ( -0.5619217318086660029, -7.564468822943311466, -6.443866470201765395 ) ) ;
#1332 = CARTESIAN_POINT ( 'NONE',  ( -2.426778023690262742, 214.6231898156240163, 49.10113791807857808 ) ) ;
#1333 =( NAMED_UNIT ( * ) SI_UNIT ( $, .STERADIAN. ) SOLID_ANGLE_UNIT ( ) );
#1334 = EDGE_CURVE ( 'NONE', #258, #1780, #13570, .T. ) ;
#1335 = CARTESIAN_POINT ( 'NONE',  ( 9.984503880673420539, 210.2968891136705167, 30.84886208192142831 ) ) ;
#1336 = CARTESIAN_POINT ( 'NONE',  ( 71.27499999726882152, 149.9369285172503510, -15.58253175000000823 ) ) ;
#1337 = VERTEX_POINT ( 'NONE', #24281 ) ;
#1338 = FACE_OUTER_BOUND ( 'NONE', #3579, .T. ) ;
#1339 = CARTESIAN_POINT ( 'NONE',  ( 51.98867513459482126, 146.1832212156128890, 12.13525491562421976 ) ) ;
#1340 = DIRECTION ( 'NONE',  ( 1.000000000000000000, 0.000000000000000000, 0.000000000000000000 ) ) ;
#1341 = CARTESIAN_POINT ( 'NONE',  ( 6.500168698208244500, 202.3363017425938324, 16.29886208192143471 ) ) ;
#1342 = CARTESIAN_POINT ( 'NONE',  ( 9.984503880673470277, 203.7031108863295401, 62.15113791807856813 ) ) ;
#1343 = CARTESIAN_POINT ( 'NONE',  ( -6.220909254589537696, 198.5229672870051161, 51.05113791807856671 ) ) ;
#1344 = CARTESIAN_POINT ( 'NONE',  ( 37.91132485994280898, 163.8167787843871110, -12.13525491562423397 ) ) ;
#1345 = CARTESIAN_POINT ( 'NONE',  ( -0.05014649552828365914, 215.4116977939061144, 99.24886208192143044 ) ) ;
#1346 = CARTESIAN_POINT ( 'NONE',  ( 42.82499999726879736, 141.7447067706911810, -9.630534252274385310 ) ) ;
#1347 = DIRECTION ( 'NONE',  ( 0.000000000000000000, 0.000000000000000000, -1.000000000000000000 ) ) ;
#1348 = CARTESIAN_POINT ( 'NONE',  ( 34.02499999726880731, 160.0630714827496206, 15.58253174999999224 ) ) ;
#1349 = CARTESIAN_POINT ( 'NONE',  ( -0.05014649552807705357, 194.3824533091408000, 20.75113791807856600 ) ) ;
#1350 = CARTESIAN_POINT ( 'NONE',  ( 99.99999999999998579, 4.171999999999999709, 0.000000000000000000 ) ) ;
#1351 = CARTESIAN_POINT ( 'NONE',  ( 3.044812012440130555, 197.4746971517856764, 62.60113791807857098 ) ) ;
#1352 = CARTESIAN_POINT ( 'NONE',  ( -8.118202686958039038, 201.1607312380087080, 39.20113791807857240 ) ) ;
#1353 = CARTESIAN_POINT ( 'NONE',  ( -1.750000000000016209, -3.031088913245524985, -2.899999999999999911 ) ) ;
#1354 = CARTESIAN_POINT ( 'NONE',  ( -12.00000000000000711, 206.9523078486584780, 8.498862081921435774 ) ) ;
#1355 = CARTESIAN_POINT ( 'NONE',  ( 8.118202686958138514, 201.1607312380088501, 13.29886208192143648 ) ) ;
#1356 = CARTESIAN_POINT ( 'NONE',  ( 69.99999999453763166, 155.0000000000000000, -14.50000000000000711 ) ) ;
#1357 = EDGE_LOOP ( 'NONE', ( #5317, #13106 ) ) ;
#1358 = CARTESIAN_POINT ( 'NONE',  ( 3.662846001190051659, 195.5725841191953691, 50.60113791807857808 ) ) ;
#1359 = CARTESIAN_POINT ( 'NONE',  ( -2.426778023690262742, 214.6231898156240163, 73.10113791807857808 ) ) ;
#1360 = B_SPLINE_CURVE_WITH_KNOTS ( 'NONE', 3,
 ( #19450, #17063, #27787, #6512, #16723, #24567, #11623, #27126, #17401, #27615 ),
 .UNSPECIFIED., .F., .F.,
 ( 4, 2, 2, 2, 4 ),
 ( 0.000000000000000000, 0.002305503304226491634, 0.004611006608452983269, 0.006916509912679474036, 0.009222013216905963068 ),
 .UNSPECIFIED. ) ;
#1361 = CARTESIAN_POINT ( 'NONE',  ( -10.00000000000000711, 206.9523078486584495, 29.49886208192143400 ) ) ;
#1362 = CARTESIAN_POINT ( 'NONE',  ( 45.51132485994280330, 146.1832212156128890, -12.13525491562423042 ) ) ;
#1363 = ORIENTED_EDGE ( 'NONE', *, *, #31628, .F. ) ;
#1364 = CARTESIAN_POINT ( 'NONE',  ( 9.984503880673470277, 203.7031108863295401, 89.15113791807857524 ) ) ;
#1365 = EDGE_LOOP ( 'NONE', ( #22857, #1283 ) ) ;
#1366 = DIRECTION ( 'NONE',  ( 0.000000000000000000, 0.000000000000000000, 1.000000000000000000 ) ) ;
#1367 = CARTESIAN_POINT ( 'NONE',  ( 0.000000000000000000, 0.000000000000000000, -6.800000000000000711 ) ) ;
#1368 = ORIENTED_EDGE ( 'NONE', *, *, #590, .T. ) ;
#1369 = CARTESIAN_POINT ( 'NONE',  ( -2.517493886308901807, 199.4062855549015012, 26.90113791807856813 ) ) ;
#1370 = CARTESIAN_POINT ( 'NONE',  ( 55.71132485994280614, 155.0000000000000000, -15.00000000000002487 ) ) ;
#1371 = EDGE_CURVE ( 'NONE', #3136, #6813, #17831, .T. ) ;
#1372 = CARTESIAN_POINT ( 'NONE',  ( 0.05014649552828275708, 196.4853777576173002, 1.748862081921434219 ) ) ;
#1373 = CARTESIAN_POINT ( 'NONE',  ( 50.87499999726881583, 138.6155565068815747, -3.929120461958505118E-15 ) ) ;
#1374 = ORIENTED_EDGE ( 'NONE', *, *, #24292, .T. ) ;
#1375 = CARTESIAN_POINT ( 'NONE',  ( 7.984503880673485376, 204.3529502787953902, 47.15113791807857524 ) ) ;
#1376 = CARTESIAN_POINT ( 'NONE',  ( 0.000000000000000000, 0.000000000000000000, 9.480888224575629408 ) ) ;
#1377 = CYLINDRICAL_SURFACE ( 'NONE', #8631, 15.00000000000001776 ) ;
#1378 = CARTESIAN_POINT ( 'NONE',  ( -8.062137200540822946, 201.0835637161416400, 95.19886208192143329 ) ) ;
#1379 = CARTESIAN_POINT ( 'NONE',  ( 56.77499999726881441, 140.1801316387863778, 4.815267126137185549 ) ) ;
#1380 = CARTESIAN_POINT ( 'NONE',  ( -9.984503880673473830, 210.2968891136704315, 27.65113791807855748 ) ) ;
#1381 = CARTESIAN_POINT ( 'NONE',  ( 0.1999999999999987899, 0.000000000000000000, 0.000000000000000000 ) ) ;
#1382 = CARTESIAN_POINT ( 'NONE',  ( -3.662846001189865142, 195.5725841191952838, 82.89886208192143613 ) ) ;
#1383 = DIRECTION ( 'NONE',  ( 0.000000000000000000, 0.7071067811865389130, -0.7071067811865561215 ) ) ;
#1384 = EDGE_CURVE ( 'NONE', #5506, #3951, #5563, .T. ) ;
#1385 = CARTESIAN_POINT ( 'NONE',  ( 80.60000000000000853, 159.7113355953771077, -14.50000000000000888 ) ) ;
#1386 = CARTESIAN_POINT ( 'NONE',  ( -56.33087447058203168, 194.9805812333615620, -1.253637678855320958 ) ) ;
#1387 = CARTESIAN_POINT ( 'NONE',  ( -4.945910536743085117, 206.2642604888503968, -6.000000000000014211 ) ) ;
#1388 = CARTESIAN_POINT ( 'NONE',  ( -6.139770520408369237, 215.5359834540460042, 93.95113791807854398 ) ) ;
#1389 = CARTESIAN_POINT ( 'NONE',  ( -3.499999999999996891, 4.286263797015732651E-16, 9.480888224575629408 ) ) ;
#1390 = CARTESIAN_POINT ( 'NONE',  ( 43.37499999726881583, 155.0000000000000000, -15.58253175000000823 ) ) ;
#1391 = CARTESIAN_POINT ( 'NONE',  ( 3.044812012440130555, 197.4746971517856764, 38.60113791807857098 ) ) ;
#1392 = CARTESIAN_POINT ( 'NONE',  ( 85.42499999726879878, 168.2552932293087906, -9.630534252274385310 ) ) ;
#1393 = CARTESIAN_POINT ( 'NONE',  ( 103.3032345859876102, 155.0000000000000000, 0.000000000000000000 ) ) ;
#1394 = EDGE_CURVE ( 'NONE', #20431, #4805, #4178, .T. ) ;
#1395 = DIRECTION ( 'NONE',  ( -0.000000000000000000, -0.000000000000000000, 1.000000000000000000 ) ) ;
#1396 = CARTESIAN_POINT ( 'NONE',  ( 48.09999999453763309, 159.7113355953771077, -14.50000000000000888 ) ) ;
#1397 =( BOUNDED_CURVE ( )  B_SPLINE_CURVE ( 2, ( #526, #26411, #26243, #10593, #8684, #8199, #10918, #11242, #5782, #16178, #31365 ),
 .UNSPECIFIED., .F., .T. ) 
 B_SPLINE_CURVE_WITH_KNOTS ( ( 3, 2, 2, 2, 2, 3 ),
 ( 0.5714285714285713969, 0.5749999999999999556, 0.5785714285714284033, 0.5821428571428569620, 0.5857142857142854098, 0.5892857142857139685 ),
 .UNSPECIFIED. ) 
 CURVE ( )  GEOMETRIC_REPRESENTATION_ITEM ( )  RATIONAL_B_SPLINE_CURVE ( ( 1.000000000000000000, 0.9510565162951534202, 1.000000000000000000, 0.9510565162951534202, 1.000000000000000000, 0.9510565162951534202, 1.000000000000000000, 0.9510565162951534202, 1.000000000000000000, 0.9510565162951564178, 0.9999999999999970024 ) ) 
 REPRESENTATION_ITEM ( '' )  );
#1398 = ORIENTED_EDGE ( 'NONE', *, *, #9346, .T. ) ;
#1399 = CARTESIAN_POINT ( 'NONE',  ( 12.00000000000000711, 206.9523078486586485, 20.00113791807856956 ) ) ;
#1400 = CARTESIAN_POINT ( 'NONE',  ( 117.5000000000000142, 155.0000000000000000, -6.938893903907228378E-15 ) ) ;
#1401 = CARTESIAN_POINT ( 'NONE',  ( -64.50000000000000000, 120.3589838486224437, 20.00000000000000000 ) ) ;
#1402 = EDGE_LOOP ( 'NONE', ( #32485, #23415, #19645, #30569 ) ) ;
#1403 = CARTESIAN_POINT ( 'NONE',  ( -9.736236675708031640, 214.0148392665760753, 41.79886208192143471 ) ) ;
#1404 = CARTESIAN_POINT ( 'NONE',  ( -8.118202686958039038, 201.1607312380087080, 6.201137918078566180 ) ) ;
#1405 = CARTESIAN_POINT ( 'NONE',  ( -0.05014649552810635652, 196.4853777576173002, 59.75113791807857666 ) ) ;
#1406 = EDGE_CURVE ( 'NONE', #29143, #25974, #30427, .T. ) ;
#1407 = CARTESIAN_POINT ( 'NONE',  ( -8.000000000000008882, 206.9523078486584780, 17.49886208192143400 ) ) ;
#1408 = CARTESIAN_POINT ( 'NONE',  ( 50.78867513459482552, 155.0000000000000000, -15.00000000000002487 ) ) ;
#1409 = VERTEX_POINT ( 'NONE', #4355 ) ;
#1410 = CARTESIAN_POINT ( 'NONE',  ( -6.500168698208244500, 211.6636982574061676, 95.79886208192144181 ) ) ;
#1411 = EDGE_CURVE ( 'NONE', #11140, #8132, #1300, .T. ) ;
#1412 = CARTESIAN_POINT ( 'NONE',  ( 109.0104235265664272, 155.0000000000000000, 0.000000000000000000 ) ) ;
#1413 = CARTESIAN_POINT ( 'NONE',  ( -7.984503880673488041, 209.6470497212046098, 39.65113791807857524 ) ) ;
#1414 = DIRECTION ( 'NONE',  ( 0.000000000000000000, 0.000000000000000000, -1.000000000000000000 ) ) ;
#1415 = EDGE_LOOP ( 'NONE', ( #27587, #28020, #15988, #9582, #29643, #3118 ) ) ;
#1416 = CARTESIAN_POINT ( 'NONE',  ( 38.62499999726880873, 138.6155565068815463, -3.929120461958505118E-15 ) ) ;
#1417 = CARTESIAN_POINT ( 'NONE',  ( -58.50000000000002132, 209.9999999999999716, 0.000000000000000000 ) ) ;
#1418 = CARTESIAN_POINT ( 'NONE',  ( 9.984503880673470277, 203.7031108863295401, -0.8488620819214341973 ) ) ;
#1419 = CARTESIAN_POINT ( 'NONE',  ( -3.135527875058982783, 216.4958274776886924, 66.09886208192143897 ) ) ;
#1420 = CARTESIAN_POINT ( 'NONE',  ( 42.57499999726881157, 145.8408176439707802, 12.60653300113718345 ) ) ;
#1421 = DIRECTION ( 'NONE',  ( 0.000000000000000000, 0.000000000000000000, -1.000000000000000000 ) ) ;
#1422 = CARTESIAN_POINT ( 'NONE',  ( -9.984503880673473830, 210.2968891136704315, 6.651137918078564581 ) ) ;
#1423 = EDGE_CURVE ( 'NONE', #13631, #32991, #13115, .T. ) ;
#1424 = CARTESIAN_POINT ( 'NONE',  ( 64.00000000000000000, 139.7537977485451393, -4.138211985947621020E-15 ) ) ;
#1425 = CARTESIAN_POINT ( 'NONE',  ( -16.00000000000000000, 1.959434878635765131E-15, -18.00000000000000000 ) ) ;
#1426 = CARTESIAN_POINT ( 'NONE',  ( 6.500168698208244500, 202.3363017425938324, 85.29886208192145602 ) ) ;
#1427 = DIRECTION ( 'NONE',  ( 0.000000000000000000, 1.000000000000000000, -1.478898702612462246E-15 ) ) ;
#1428 = CARTESIAN_POINT ( 'NONE',  ( 3.500000000000004885, 0.6879904500768362352, -2.869836757075876488 ) ) ;
#1429 = CARTESIAN_POINT ( 'NONE',  ( 66.22499999726879594, 149.9369285172503510, 15.58253174999999580 ) ) ;
#1431 = ORIENTED_EDGE ( 'NONE', *, *, #723, .F. ) ;
#1430 = CARTESIAN_POINT ( 'NONE',  ( -3.044812012440131443, 216.5253028482142952, 19.10113791807856742 ) ) ;
#1432 = CARTESIAN_POINT ( 'NONE',  ( 0.000000000000000000, 0.000000000000000000, -2.899999999999999911 ) ) ;
#1433 = CARTESIAN_POINT ( 'NONE',  ( 80.97499999726881015, 140.1801316387863778, -4.815267126137194431 ) ) ;
#1434 = CARTESIAN_POINT ( 'NONE',  ( -11.98450388067348804, 210.9467285061362247, 84.65113791807856103 ) ) ;
#1435 = EDGE_CURVE ( 'NONE', #18587, #26841, #4226, .T. ) ;
#1436 = CARTESIAN_POINT ( 'NONE',  ( 71.98867513459481415, 146.1832212156128890, 12.13525491562421976 ) ) ;
#1437 = CARTESIAN_POINT ( 'NONE',  ( 52.78867513459482552, 155.0000000000000000, -15.00000000000002487 ) ) ;
#1438 = CONICAL_SURFACE ( 'NONE', #19943, 4.057500000000000107, 1.047197551196593857 ) ;
#1439 = ORIENTED_EDGE ( 'NONE', *, *, #8775, .F. ) ;
#1440 = CARTESIAN_POINT ( 'NONE',  ( 7.375838497908012492, 217.2372850707501186, 69.54886208192141339 ) ) ;
#1441 = CARTESIAN_POINT ( 'NONE',  ( -3.044812012439970683, 197.4746971517856196, 79.89886208192143613 ) ) ;
#1442 = CARTESIAN_POINT ( 'NONE',  ( 11.98450388067341876, 210.9467285061363953, 12.84886208192143719 ) ) ;
#1443 = CARTESIAN_POINT ( 'NONE',  ( -6.815830331203684089, 0.6610623347507950109, -6.171384342982605631 ) ) ;
#1444 = CARTESIAN_POINT ( 'NONE',  ( 6.220909254589536808, 215.4770327129947702, 25.55113791807856671 ) ) ;
#1445 = EDGE_CURVE ( 'NONE', #562, #19762, #2143, .T. ) ;
#1446 = DIRECTION ( 'NONE',  ( -0.5000000000000004441, -0.8660254037844383745, 0.000000000000000000 ) ) ;
#1447 = CARTESIAN_POINT ( 'NONE',  ( -8.118202686958138514, 212.8392687619910930, 89.79886208192144181 ) ) ;
#1448 = AXIS2_PLACEMENT_3D ( 'NONE', #12317, #22712, #9769 ) ;
#1449 = CARTESIAN_POINT ( 'NONE',  ( 63.61132485994281893, 150.1262045565062806, -14.99999999999993072 ) ) ;
#1450 = EDGE_LOOP ( 'NONE', ( #15818, #25203 ) ) ;
#1451 = DIRECTION ( 'NONE',  ( 0.000000000000000000, -0.4999999999999995004, 0.8660254037844389297 ) ) ;
#1452 = CARTESIAN_POINT ( 'NONE',  ( 4.984841277089891776, 200.2242689037093726, 67.44886208192143329 ) ) ;
#1453 = VERTEX_POINT ( 'NONE', #9126 ) ;
#1454 = CARTESIAN_POINT ( 'NONE',  ( 85.32499999726880446, 164.1591823560292198, -12.60653300113719766 ) ) ;
#1455 = ORIENTED_EDGE ( 'NONE', *, *, #14682, .F. ) ;
#1456 = CARTESIAN_POINT ( 'NONE',  ( -67.50000000000000000, 155.0000000000000000, 6.938893903907228378E-15 ) ) ;
#1457 = CARTESIAN_POINT ( 'NONE',  ( 79.32499999726881867, 164.1591823560292198, -12.60653300113719766 ) ) ;
#1458 = CARTESIAN_POINT ( 'NONE',  ( 16.09259079475562615, -22.46320317811879264, -17.99999999999998579 ) ) ;
#1459 = CARTESIAN_POINT ( 'NONE',  ( 7.984503880673485376, 204.3529502787953902, 80.15113791807857524 ) ) ;
#1460 = CIRCLE ( 'NONE', #25958, 40.00000000000000711 ) ;
#1461 = CIRCLE ( 'NONE', #24856, 3.399999999999999911 ) ;
#1462 = CARTESIAN_POINT ( 'NONE',  ( 42.10000000000000142, 141.2096805137202580, -4.480746418436742040 ) ) ;
#1463 = CARTESIAN_POINT ( 'NONE',  ( 6.500168698208244500, 202.3363017425938324, 52.29886208192144892 ) ) ;
#1464 = EDGE_CURVE ( 'NONE', #7737, #13563, #32457, .T. ) ;
#1465 = EDGE_CURVE ( 'NONE', #1492, #15895, #8561, .T. ) ;
#1466 = AXIS2_PLACEMENT_3D ( 'NONE', #27737, #29794, #30294 ) ;
#1467 = CARTESIAN_POINT ( 'NONE',  ( 6.500000000000000000, 3.752776749732563921, -6.064240316920399110 ) ) ;
#1468 = CARTESIAN_POINT ( 'NONE',  ( 78.68867513459480278, 150.1262045565062522, -14.99999999999990763 ) ) ;
#1469 = LINE ( 'NONE', #27359, #5012 ) ;
#1470 = CARTESIAN_POINT ( 'NONE',  ( 53.62499999726881583, 171.3844434931184253, -7.942151717890134290E-15 ) ) ;
#1471 = CARTESIAN_POINT ( 'NONE',  ( 65.27499999726880731, 149.9369285172503510, -15.58253175000000823 ) ) ;
#1472 = CARTESIAN_POINT ( 'NONE',  ( 7.375838497908181246, 196.7627149292499666, 56.45113791807857240 ) ) ;
#1473 = CARTESIAN_POINT ( 'NONE',  ( -123.6258236071137446, -5.113356552508658837, 35.00001199999999102 ) ) ;
#1474 = ADVANCED_FACE ( 'NONE', ( #6406 ), #421, .T. ) ;
#1475 = CARTESIAN_POINT ( 'NONE',  ( 11.98450388067348271, 203.0532714938637753, 2.151137918078565914 ) ) ;
#1476 = ADVANCED_FACE ( 'NONE', ( #27189 ), #19854, .F. ) ;
#1477 = CARTESIAN_POINT ( 'NONE',  ( -6.139770520408368348, 215.5359834540460042, 78.95113791807857240 ) ) ;
#1478 = CARTESIAN_POINT ( 'NONE',  ( -7.456977232089471386, 217.1783343296987709, 38.94886208192143329 ) ) ;
#1479 = CARTESIAN_POINT ( 'NONE',  ( 6.139770520408223575, 215.5359834540460611, 48.54886208192143471 ) ) ;
#1480 = CARTESIAN_POINT ( 'NONE',  ( 83.59999999453762598, 141.2096805137202580, -4.480746418436742040 ) ) ;
#1481 = CARTESIAN_POINT ( 'NONE',  ( 12.00000000000000711, 206.9523078486586485, 89.00113791807858377 ) ) ;
#1482 = CONICAL_SURFACE ( 'NONE', #33017, 31.00000000000000000, 1.466076571675244411 ) ;
#1483 = CARTESIAN_POINT ( 'NONE',  ( -6.444103211791042618, 211.7408657792732356, 93.80113791807858092 ) ) ;
#1484 = CARTESIAN_POINT ( 'NONE',  ( -3.135527875058982783, 216.4958274776886924, 63.09886208192143187 ) ) ;
#1485 = CONICAL_SURFACE ( 'NONE', #10213, 32.00000000000002842, 0.1047197551196464710 ) ;
#1486 = CARTESIAN_POINT ( 'NONE',  ( 0.000000000000000000, 0.000000000000000000, 3.100000000000000533 ) ) ;
#1487 = EDGE_LOOP ( 'NONE', ( #7285, #14189, #23041, #24412 ) ) ;
#1488 = CARTESIAN_POINT ( 'NONE',  ( -0.05014649552828442242, 219.6175466908591716, 69.24886208192143044 ) ) ;
#1489 = ORIENTED_EDGE ( 'NONE', *, *, #4823, .T. ) ;
#1490 = CARTESIAN_POINT ( 'NONE',  ( 68.57499999726881867, 145.8408176439707802, 12.60653300113718345 ) ) ;
#1491 = CARTESIAN_POINT ( 'NONE',  ( 4.903702542908435547, 213.8346818373419751, 42.54886208192144181 ) ) ;
#1492 = VERTEX_POINT ( 'NONE', #16788 ) ;
#1493 = AXIS2_PLACEMENT_3D ( 'NONE', #20677, #28516, #8228 ) ;
#1494 = CARTESIAN_POINT ( 'NONE',  ( 84.87499999726881583, 138.6155565068815747, -3.929120461958505118E-15 ) ) ;
#1495 = DIRECTION ( 'NONE',  ( 0.000000000000000000, 0.000000000000000000, 1.000000000000000000 ) ) ;
#1496 = CARTESIAN_POINT ( 'NONE',  ( -9.207158067219113562, 207.6631797465213651, 102.8962158735644579 ) ) ;
#1497 = CARTESIAN_POINT ( 'NONE',  ( 8.000000000000008882, 206.9523078486586485, 62.00113791807856956 ) ) ;
#1498 = DIRECTION ( 'NONE',  ( 0.000000000000000000, 0.000000000000000000, -1.000000000000000000 ) ) ;
#1499 = CARTESIAN_POINT ( 'NONE',  ( -8.062137200540822946, 201.0835637161416400, 47.19886208192143329 ) ) ;
#1500 = ORIENTED_EDGE ( 'NONE', *, *, #5938, .T. ) ;
#1501 = DIRECTION ( 'NONE',  ( 0.000000000000000000, 1.000000000000000000, -9.682177540335733218E-15 ) ) ;
#1502 = DIRECTION ( 'NONE',  ( 1.000000000000000000, 0.000000000000000000, 0.000000000000000000 ) ) ;
#1503 = CARTESIAN_POINT ( 'NONE',  ( 0.000000000000000000, 0.000000000000000000, -2.899999999999999911 ) ) ;
#1504 = CARTESIAN_POINT ( 'NONE',  ( -6.500168698208244500, 211.6636982574061676, 26.79886208192143826 ) ) ;
#1505 = CARTESIAN_POINT ( 'NONE',  ( 3.044812012440130555, 197.4746971517856764, 62.60113791807857098 ) ) ;
#1506 = CARTESIAN_POINT ( 'NONE',  ( 3.044812012440130555, 197.4746971517856764, 44.60113791807857098 ) ) ;
#1507 = CARTESIAN_POINT ( 'NONE',  ( 71.41132485994282320, 142.2402378747194405, -9.270509831248439525 ) ) ;
#1508 = AXIS2_PLACEMENT_3D ( 'NONE', #25293, #33136, #15242 ) ;
#1509 = ITEM_DEFINED_TRANSFORMATION ( 'NONE', 'NONE', #20265,  #2404 ) ;
#1510 = CARTESIAN_POINT ( 'NONE',  ( -10.00000000000000711, 207.0476921513413515, 18.50113791807856956 ) ) ;
#1511 = CARTESIAN_POINT ( 'NONE',  ( 7.984503880673422316, 209.6470497212048372, 99.84886208192143897 ) ) ;
#1512 = CARTESIAN_POINT ( 'NONE',  ( 44.42499999726881299, 141.7447067706911810, 9.630534252274376428 ) ) ;
#1513 = CARTESIAN_POINT ( 'NONE',  ( 87.50000000000001421, 155.6617420473934885, -15.38934888333735884 ) ) ;
#1514 = CARTESIAN_POINT ( 'NONE',  ( -9.680171189290831535, 214.0920067884431148, 24.80113791807857027 ) ) ;
#1515 = DIRECTION ( 'NONE',  ( -0.000000000000000000, -0.000000000000000000, 1.000000000000000000 ) ) ;
#1516 = CARTESIAN_POINT ( 'NONE',  ( -3.044812012440131443, 216.5253028482142952, 76.10113791807856387 ) ) ;
#1517 = CARTESIAN_POINT ( 'NONE',  ( -9.984503880673475606, 210.2968891136704315, 48.65113791807857524 ) ) ;
#1518 = AXIS2_PLACEMENT_3D ( 'NONE', #2238, #23684, #33580 ) ;
#1519 = CARTESIAN_POINT ( 'NONE',  ( 97.20416941062678973, 155.0000000000000000, -32.00000000000000000 ) ) ;
#1520 = CARTESIAN_POINT ( 'NONE',  ( -6.938893903907228378E-15, 31.75426480542944319, 0.000000000000000000 ) ) ;
#1521 = CARTESIAN_POINT ( 'NONE',  ( 7.456977232089471386, 196.8216656703012006, 1.448862081921433953 ) ) ;
#1522 = CARTESIAN_POINT ( 'NONE',  ( -8.118202686958138514, 212.8392687619910930, 23.79886208192143471 ) ) ;
#1523 = CARTESIAN_POINT ( 'NONE',  ( 69.19999999453763451, 146.4771138417591203, 11.73074641843673227 ) ) ;
#1524 = ORIENTED_EDGE ( 'NONE', *, *, #31571, .T. ) ;
#1525 = CARTESIAN_POINT ( 'NONE',  ( -7.375838497908182134, 217.2372850707499765, 57.95113791807855819 ) ) ;
#1526 = CARTESIAN_POINT ( 'NONE',  ( -2.517493886308901807, 199.4062855549015012, 68.90113791807856103 ) ) ;
#1527 = CARTESIAN_POINT ( 'NONE',  ( 3.135527875058981895, 197.5041725223112792, 28.59886208192143897 ) ) ;
#1528 = ORIENTED_EDGE ( 'NONE', *, *, #28754, .T. ) ;
#1529 = CARTESIAN_POINT ( 'NONE',  ( -10.00000000000000711, 207.0476921513413515, 90.50113791807858377 ) ) ;
#1530 = CIRCLE ( 'NONE', #18391, 112.0000000000000426 ) ;
#1531 = EDGE_LOOP ( 'NONE', ( #25675, #4715, #28812, #32881 ) ) ;
#1532 = PRODUCT ( 'hex flange nut gradea_iso_ISO - 4161 - M8 - N', 'hex flange nut gradea_iso_ISO - 4161 - M8 - N', '', ( #18240 ) ) ;
#1533 = CONICAL_SURFACE ( 'NONE', #9166, 3.499999999999999556, 1.047197551196589638 ) ;
#1534 = CARTESIAN_POINT ( 'NONE',  ( 42.48867513459482836, 142.2402378747194405, -9.270509831248439525 ) ) ;
#1535 = CARTESIAN_POINT ( 'NONE',  ( 2.133938722758552675, 6.273523403446317204, -0.09463688534106567962 ) ) ;
#1536 = ORIENTED_EDGE ( 'NONE', *, *, #15348, .F. ) ;
#1537 = CARTESIAN_POINT ( 'NONE',  ( -6.444103211791042618, 211.7408657792732356, 30.80113791807857027 ) ) ;
#1538 = CARTESIAN_POINT ( 'NONE',  ( 55.31132485994280756, 140.7341522555726669, -4.635254915624220651 ) ) ;
#1539 = CARTESIAN_POINT ( 'NONE',  ( 6.139770520408223575, 215.5359834540460611, 12.54886208192143648 ) ) ;
#1540 = CARTESIAN_POINT ( 'NONE',  ( 50.47499999726881015, 149.9369285172503510, 15.58253174999999580 ) ) ;
#1542 = ORIENTED_EDGE ( 'NONE', *, *, #8231, .F. ) ;
#1541 = AXIS2_PLACEMENT_3D ( 'NONE', #27704, #4366, #11701 ) ;
#1543 = CARTESIAN_POINT ( 'NONE',  ( -7.984503880673488041, 209.6470497212046098, 45.65113791807857524 ) ) ;
#1544 = DIRECTION ( 'NONE',  ( -0.000000000000000000, -0.000000000000000000, -1.000000000000000000 ) ) ;
#1545 = DIRECTION ( 'NONE',  ( 0.000000000000000000, 0.000000000000000000, -1.000000000000000000 ) ) ;
#1546 = CARTESIAN_POINT ( 'NONE',  ( 8.118202686958138514, 201.1607312380088501, 88.29886208192142760 ) ) ;
#1547 = CARTESIAN_POINT ( 'NONE',  ( 58.57499999726881157, 145.8408176439707802, 12.60653300113718345 ) ) ;
#1548 = CARTESIAN_POINT ( 'NONE',  ( 6.139770520408368348, 198.4640165459539674, 29.45113791807856529 ) ) ;
#1549 = CARTESIAN_POINT ( 'NONE',  ( -11.00000000000000178, 206.7692714347155629, 108.3323677711372000 ) ) ;
#1550 = CARTESIAN_POINT ( 'NONE',  ( 3.135527875058820690, 216.4958274776887492, 19.40113791807856813 ) ) ;
#1551 = DIRECTION ( 'NONE',  ( 1.000000000000000000, 0.000000000000000000, 0.000000000000000000 ) ) ;
#1552 = CARTESIAN_POINT ( 'NONE',  ( 78.10000000000000853, 141.2096805137202580, -4.480746418436742040 ) ) ;
#1553 = CARTESIAN_POINT ( 'NONE',  ( -9.093938419273312590, -26.50387701106812344, -0.2340887491524524799 ) ) ;
#1554 = CARTESIAN_POINT ( 'NONE',  ( 8.399999999999998579, 0.000000000000000000, 4.000000000000000888 ) ) ;
#1555 = CARTESIAN_POINT ( 'NONE',  ( -0.05014649552807705357, 194.3824533091408000, 2.751137918078565114 ) ) ;
#1556 = AXIS2_PLACEMENT_3D ( 'NONE', #24295, #8307, #8795 ) ;
#1557 = CARTESIAN_POINT ( 'NONE',  ( -54.75000000000000711, -7.347880794884118356E-15, 35.00000000000000000 ) ) ;
#1558 = CARTESIAN_POINT ( 'NONE',  ( 41.87499999726880162, 171.3844434931184253, -7.942151717890132712E-15 ) ) ;
#1559 = CARTESIAN_POINT ( 'NONE',  ( -0.05014649552810635652, 196.4853777576173002, 44.75113791807858377 ) ) ;
#1560 = CIRCLE ( 'NONE', #7565, 6.500000000000000000 ) ;
#1561 = CARTESIAN_POINT ( 'NONE',  ( 84.22499999726879594, 149.9369285172503510, 15.58253174999999580 ) ) ;
#1562 = AXIS2_PLACEMENT_3D ( 'NONE', #7257, #10331, #18155 ) ;
#1563 = FACE_BOUND ( 'NONE', #24828, .T. ) ;
#1564 = DIRECTION ( 'NONE',  ( 0.000000000000000000, 0.000000000000000000, -1.000000000000000000 ) ) ;
#1565 = CARTESIAN_POINT ( 'NONE',  ( 46.39999999453763024, 168.7903194862797420, -4.480746418436745593 ) ) ;
#1566 = EDGE_LOOP ( 'NONE', ( #30199, #32332, #23952, #6736 ) ) ;
#1567 = CARTESIAN_POINT ( 'NONE',  ( -12.01549611932652972, 203.1486557965464499, 18.35113791807856387 ) ) ;
#1568 = FACE_OUTER_BOUND ( 'NONE', #10760, .T. ) ;
#1569 = EDGE_CURVE ( 'NONE', #4633, #19912, #4976, .T. ) ;
#1570 = CARTESIAN_POINT ( 'NONE',  ( 66.71132485994280614, 155.0000000000000000, 15.00000000000001243 ) ) ;
#1571 = ORIENTED_EDGE ( 'NONE', *, *, #15447, .F. ) ;
#1572 = CARTESIAN_POINT ( 'NONE',  ( 11.98450388067341876, 210.9467285061363953, 42.84886208192143187 ) ) ;
#1573 = CARTESIAN_POINT ( 'NONE',  ( 10.00000000000000711, 206.9523078486586201, 2.001137918078565558 ) ) ;
#1574 = CARTESIAN_POINT ( 'NONE',  ( -3.044812012440131443, 216.5253028482142952, 64.10113791807857808 ) ) ;
#1575 = CARTESIAN_POINT ( 'NONE',  ( 8.015496119326595448, 204.4483345814782638, 19.14886208192143968 ) ) ;
#1576 = CARTESIAN_POINT ( 'NONE',  ( 92.60208470531341618, 155.0000000000000000, 31.00000000000000000 ) ) ;
#1577 = EDGE_LOOP ( 'NONE', ( #29940, #16353, #31307, #23424 ) ) ;
#1578 = CARTESIAN_POINT ( 'NONE',  ( 4.984841277089891776, 200.2242689037093726, 100.4488620819214475 ) ) ;
#1579 = AXIS2_PLACEMENT_3D ( 'NONE', #10338, #33321, #5373 ) ;
#1580 = DIRECTION ( 'NONE',  ( 0.000000000000000000, 0.000000000000000000, -1.000000000000000000 ) ) ;
#1581 = CARTESIAN_POINT ( 'NONE',  ( 0.05014649552807626948, 215.4116977939061144, 40.25113791807856956 ) ) ;
#1582 = CARTESIAN_POINT ( 'NONE',  ( 8.399999999999998579, 0.000000000000000000, 0.000000000000000000 ) ) ;
#1583 = EDGE_LOOP ( 'NONE', ( #28454, #13185, #30058, #28016 ) ) ;
#1584 = CARTESIAN_POINT ( 'NONE',  ( 35.62499999726880873, 171.3844434931184253, -7.942151717890132712E-15 ) ) ;
#1585 = DIRECTION ( 'NONE',  ( -0.000000000000000000, -0.000000000000000000, 1.000000000000000000 ) ) ;
#1586 = CARTESIAN_POINT ( 'NONE',  ( -10.00000000000000711, 207.0476921513413515, 0.5011379180785656695 ) ) ;
#1587 = CIRCLE ( 'NONE', #5925, 8.331345277524542681 ) ;
#1588 = CARTESIAN_POINT ( 'NONE',  ( -9.984503880673420539, 203.7031108863293980, 65.34886208192143897 ) ) ;
#1589 = CARTESIAN_POINT ( 'NONE',  ( 40.07499999726879736, 168.2552932293087906, 9.630534252274372875 ) ) ;
#1590 = DIRECTION ( 'NONE',  ( 1.000000000000000000, -0.000000000000000000, -0.000000000000000000 ) ) ;
#1591 = CARTESIAN_POINT ( 'NONE',  ( -8.118202686958039038, 201.1607312380087080, 3.201137918078566180 ) ) ;
#1592 = CARTESIAN_POINT ( 'NONE',  ( 6.500000000000000888, 0.000000000000000000, 0.000000000000000000 ) ) ;
#1593 = CARTESIAN_POINT ( 'NONE',  ( 60.90000000000000568, 168.7903194862797420, -4.480746418436745593 ) ) ;
#1594 =( BOUNDED_CURVE ( )  B_SPLINE_CURVE ( 2, ( #20468, #30870, #7534, #2414, #12799, #23191, #10264, #20642, #31039, #352, #13622 ),
 .UNSPECIFIED., .F., .T. ) 
 B_SPLINE_CURVE_WITH_KNOTS ( ( 3, 2, 2, 2, 2, 3 ),
 ( 0.7857142857142856984, 0.7892857142857142572, 0.7928571428571428159, 0.7964285714285713746, 0.8000000000000000444, 0.8035714285714286031 ),
 .UNSPECIFIED. ) 
 CURVE ( )  GEOMETRIC_REPRESENTATION_ITEM ( )  RATIONAL_B_SPLINE_CURVE ( ( 1.000000000000000000, 0.9510565162951534202, 1.000000000000000000, 0.9510565162951534202, 1.000000000000000000, 0.9510565162951534202, 1.000000000000000000, 0.9510565162951534202, 1.000000000000000000, 0.9510565162951534202, 1.000000000000000000 ) ) 
 REPRESENTATION_ITEM ( '' )  );
#1595 = PLANE ( 'NONE',  #22922 ) ;
#1596 = CARTESIAN_POINT ( 'NONE',  ( 2.517493886309087436, 199.4062855549015865, 82.59886208192143897 ) ) ;
#1597 = CARTESIAN_POINT ( 'NONE',  ( -7.970070017554212960, 4.546953124339755625, -8.057670357645356773 ) ) ;
#1598 = CARTESIAN_POINT ( 'NONE',  ( -60.00000000000000000, -7.347880794884118356E-15, 270.4495957273638282 ) ) ;
#1599 = CARTESIAN_POINT ( 'NONE',  ( 62.02499999726880020, 160.0630714827496206, 15.58253174999999402 ) ) ;
#1601 = ORIENTED_EDGE ( 'NONE', *, *, #18063, .F. ) ;
#1600 = CARTESIAN_POINT ( 'NONE',  ( 10.01549611932653860, 210.2015048109876716, 16.85113791807856387 ) ) ;
#1602 = CARTESIAN_POINT ( 'NONE',  ( -68.50000000000000000, 215.0000000000000000, 0.000000000000000000 ) ) ;
#1603 = CARTESIAN_POINT ( 'NONE',  ( 79.77499999726880731, 169.8198683612136222, -4.815267126137197984 ) ) ;
#1604 = CARTESIAN_POINT ( 'NONE',  ( 11.98450388067348271, 203.0532714938637753, 83.15113791807856103 ) ) ;
#1605 = CONICAL_SURFACE ( 'NONE', #3771, 31.00000000000000000, 1.466076571675244411 ) ;
#1606 = LINE ( 'NONE', #11667, #20843 ) ;
#1607 = EDGE_CURVE ( 'NONE', #8578, #22189, #6963, .T. ) ;
#1608 = ORIENTED_EDGE ( 'NONE', *, *, #24349, .F. ) ;
#1609 = CARTESIAN_POINT ( 'NONE',  ( -11.98450388067341876, 203.0532714938636047, 74.34886208192142476 ) ) ;
#1610 = CARTESIAN_POINT ( 'NONE',  ( -8.062137200540822946, 201.0835637161416400, 80.19886208192143329 ) ) ;
#1611 = CARTESIAN_POINT ( 'NONE',  ( -12.01549611932659722, 210.8513442034533227, 17.64886208192143968 ) ) ;
#1612 = DIRECTION ( 'NONE',  ( 0.000000000000000000, 0.000000000000000000, -1.000000000000000000 ) ) ;
#1613 = CARTESIAN_POINT ( 'NONE',  ( 10.00000000000000711, 206.9523078486586201, 35.00113791807856956 ) ) ;
#1614 = CARTESIAN_POINT ( 'NONE',  ( 9.984503880673420539, 210.2968891136705167, 93.84886208192143897 ) ) ;
#1615 = EDGE_CURVE ( 'NONE', #31412, #31779, #972, .T. ) ;
#1616 = CARTESIAN_POINT ( 'NONE',  ( 105.0000000000000142, 3.061616997868383121E-14, 20.00000000000000000 ) ) ;
#1617 = EDGE_LOOP ( 'NONE', ( #31985, #3988, #7749, #18258 ) ) ;
#1618 = DIRECTION ( 'NONE',  ( -0.8660254037844381525, 0.5000000000000007772, 0.000000000000000000 ) ) ;
#1619 = CARTESIAN_POINT ( 'NONE',  ( -2.426778023690076225, 199.3768101843759553, 70.89886208192143613 ) ) ;
#1620 = ORIENTED_EDGE ( 'NONE', *, *, #3918, .T. ) ;
#1621 = CARTESIAN_POINT ( 'NONE',  ( 82.92499999726882720, 145.8408176439707802, -12.60653300113719588 ) ) ;
#1622 = ORIENTED_EDGE ( 'NONE', *, *, #19447, .F. ) ;
#1623 = CARTESIAN_POINT ( 'NONE',  ( 69.78867513459482552, 155.0000000000000000, 15.00000000000001243 ) ) ;
#1624 = CARTESIAN_POINT ( 'NONE',  ( 77.42499999726882720, 168.2552932293087906, -9.630534252274385310 ) ) ;
#1625 = EDGE_CURVE ( 'NONE', #16276, #8938, #29825, .T. ) ;
#1626 = CARTESIAN_POINT ( 'NONE',  ( -7.500000000000000000, 1.854554393013821745, -0.1880126015361722192 ) ) ;
#1627 = CARTESIAN_POINT ( 'NONE',  ( 8.015496119326531499, 209.5516654185219636, 79.85113791807857808 ) ) ;
#1628 = CARTESIAN_POINT ( 'NONE',  ( 74.98867513459481415, 163.8167787843871110, -12.13525491562423397 ) ) ;
#1629 = CARTESIAN_POINT ( 'NONE',  ( 41.59999999999999432, 150.2886644046228639, 14.49999999999999645 ) ) ;
#1630 = CARTESIAN_POINT ( 'NONE',  ( 0.05014649552828262524, 198.5883022060938572, 55.74886208192144466 ) ) ;
#1631 = EDGE_CURVE ( 'NONE', #14984, #23772, #7602, .T. ) ;
#1632 = PLANE ( 'NONE',  #19178 ) ;
#1633 = CARTESIAN_POINT ( 'NONE',  ( 78.78867513459481131, 155.0000000000000000, -15.00000000000002487 ) ) ;
#1634 = CARTESIAN_POINT ( 'NONE',  ( 27.49999999999999645, 5.390523180938858516, -17.71625836475401172 ) ) ;
#1635 = CARTESIAN_POINT ( 'NONE',  ( 53.22499999726879594, 160.0630714827496206, -15.58253175000000823 ) ) ;
#1636 = CARTESIAN_POINT ( 'NONE',  ( 63.47499999726881725, 160.0630714827496206, -15.58253175000000823 ) ) ;
#1637 = CARTESIAN_POINT ( 'NONE',  ( 11.98450388067348271, 203.0532714938637753, 62.15113791807858945 ) ) ;
#1638 = CARTESIAN_POINT ( 'NONE',  ( -127.6439996469471936, -4.587378538859854693, 35.00001199999999812 ) ) ;
#1639 = CARTESIAN_POINT ( 'NONE',  ( -0.05014649552807705357, 194.3824533091408000, -0.2488620819214344970 ) ) ;
#1640 = B_SPLINE_CURVE_WITH_KNOTS ( 'NONE', 3,
 ( #8047, #14729, #17630, #26259, #20182, #22572 ),
 .UNSPECIFIED., .F., .F.,
 ( 4, 2, 4 ),
 ( 2.380727409349380532E-07, 0.008032766472079795605, 0.01606529487141865678 ),
 .UNSPECIFIED. ) ;
#1641 = CARTESIAN_POINT ( 'NONE',  ( -0.05014649552810635652, 196.4853777576173002, 80.75113791807855534 ) ) ;
#1642 = CARTESIAN_POINT ( 'NONE',  ( -12.01549611932659722, 210.8513442034533227, 44.64886208192143613 ) ) ;
#1643 = CARTESIAN_POINT ( 'NONE',  ( 0.05014649552828275014, 196.4853777576173002, 46.74886208192143755 ) ) ;
#1644 = CARTESIAN_POINT ( 'NONE',  ( -64.50000000000000000, -2.605762844159085212, -20.00000000000000000 ) ) ;
#1645 = CARTESIAN_POINT ( 'NONE',  ( -12.00000000000000711, 207.0476921513413515, 84.50113791807856956 ) ) ;
#1646 = CARTESIAN_POINT ( 'NONE',  ( -9.984503880673473830, 210.2968891136704315, 0.6511379180785656917 ) ) ;
#1647 = CARTESIAN_POINT ( 'NONE',  ( 6.139770520408223575, 215.5359834540460611, 60.54886208192143471 ) ) ;
#1648 = ORIENTED_EDGE ( 'NONE', *, *, #25576, .T. ) ;
#1649 = CARTESIAN_POINT ( 'NONE',  ( 9.680171189290716072, 214.0920067884432854, 69.69886208192143329 ) ) ;
#1650 = EDGE_LOOP ( 'NONE', ( #21855, #8372 ) ) ;
#1651 = CARTESIAN_POINT ( 'NONE',  ( 71.77499999726882152, 169.8198683612136222, -4.815267126137197984 ) ) ;
#1652 = CARTESIAN_POINT ( 'NONE',  ( -2.426778023690076225, 199.3768101843759553, 46.89886208192144323 ) ) ;
#1653 = EDGE_LOOP ( 'NONE', ( #9933, #8897, #9960 ) ) ;
#1654 = EDGE_CURVE ( 'NONE', #6694, #31012, #5880, .T. ) ;
#1655 = EDGE_CURVE ( 'NONE', #30153, #24793, #17888, .T. ) ;
#1656 = CARTESIAN_POINT ( 'NONE',  ( 86.07499999726880446, 168.2552932293087906, 9.630534252274372875 ) ) ;
#1657 = CARTESIAN_POINT ( 'NONE',  ( 32.50000000000000000, 155.0000000000000000, -6.938893903907228378E-15 ) ) ;
#1658 = FACE_OUTER_BOUND ( 'NONE', #33344, .T. ) ;
#1659 = CARTESIAN_POINT ( 'NONE',  ( 6.444103211791042618, 202.2591342207267644, 62.30113791807858092 ) ) ;
#1660 = PRODUCT_DEFINITION ( 'UNKNOWN', '', #2328, #24753 ) ;
#1661 = EDGE_CURVE ( 'NONE', #21974, #31163, #33651, .T. ) ;
#1662 = DIRECTION ( 'NONE',  ( -1.000000000000000000, 0.000000000000000000, 0.000000000000000000 ) ) ;
#1663 = CARTESIAN_POINT ( 'NONE',  ( -0.05014649552828403384, 217.5146222423826714, 39.24886208192142334 ) ) ;
#1664 = VERTEX_POINT ( 'NONE', #18314 ) ;
#1665 = DIRECTION ( 'NONE',  ( 1.000000000000000000, 0.000000000000000000, 0.000000000000000000 ) ) ;
#1666 = PRESENTATION_STYLE_ASSIGNMENT (( #4217 ) ) ;
#1667 = DIRECTION ( 'NONE',  ( -1.000000000000000000, -0.000000000000000000, -0.000000000000000000 ) ) ;
#1668 = LINE ( 'NONE', #12060, #4955 ) ;
#1669 = CARTESIAN_POINT ( 'NONE',  ( -8.000000000000008882, 206.9523078486584780, 26.49886208192143400 ) ) ;
#1670 = EDGE_CURVE ( 'NONE', #22189, #8578, #14617, .T. ) ;
#1671 = CARTESIAN_POINT ( 'NONE',  ( -3.135527875058821579, 197.5041725223112223, 56.90113791807857524 ) ) ;
#1672 = CARTESIAN_POINT ( 'NONE',  ( -6.220909254589537696, 198.5229672870051161, 45.05113791807855961 ) ) ;
#1673 = LINE ( 'NONE', #14117, #24865 ) ;
#1674 = CARTESIAN_POINT ( 'NONE',  ( 10.00000000000000711, 206.9523078486586201, 17.00113791807856600 ) ) ;
#1675 = CARTESIAN_POINT ( 'NONE',  ( 0.05014649552807626948, 215.4116977939061144, 10.25113791807856600 ) ) ;
#1676 = CARTESIAN_POINT ( 'NONE',  ( 43.72499999726881015, 169.8198683612136222, 4.815267126137181997 ) ) ;
#1677 = CYLINDRICAL_SURFACE ( 'NONE', #23078, 15.00000000000001776 ) ;
#1678 = DIRECTION ( 'NONE',  ( 1.000000000000000000, 0.000000000000000000, 0.000000000000000000 ) ) ;
#1679 = CARTESIAN_POINT ( 'NONE',  ( 3.662846001190051659, 195.5725841191953691, 29.60113791807856742 ) ) ;
#1680 = CARTESIAN_POINT ( 'NONE',  ( 6.837824896291514243, -3.947820044545437224, -6.564402953523717166 ) ) ;
#1681 = CARTESIAN_POINT ( 'NONE',  ( -8.062137200540920645, 212.9164362838581894, 72.80113791807856671 ) ) ;
#1682 = CARTESIAN_POINT ( 'NONE',  ( 8.062137200540920645, 201.0835637161417822, 50.30113791807857382 ) ) ;
#1683 = CARTESIAN_POINT ( 'NONE',  ( 75.88867513459484826, 150.1262045565061385, 14.99999999999982947 ) ) ;
#1684 = CARTESIAN_POINT ( 'NONE',  ( -52.50000000000002132, 0.000000000000000000, -20.00000000000000000 ) ) ;
#1685 = CARTESIAN_POINT ( 'NONE',  ( -0.05014649552828442242, 219.6175466908591716, 18.24886208192143755 ) ) ;
#1686 = CARTESIAN_POINT ( 'NONE',  ( -9.984503880673420539, 203.7031108863293980, 17.34886208192143542 ) ) ;
#1687 = CARTESIAN_POINT ( 'NONE',  ( 68.19999999453763451, 163.5228861582408797, -11.73074641843674470 ) ) ;
#1688 = ORIENTED_EDGE ( 'NONE', *, *, #26058, .F. ) ;
#1689 = CARTESIAN_POINT ( 'NONE',  ( 9.736236675707914401, 214.0148392665762458, 61.70113791807857240 ) ) ;
#1690 = CARTESIAN_POINT ( 'NONE',  ( -2.426778023690262742, 214.6231898156240163, 67.10113791807857808 ) ) ;
#1691 = CARTESIAN_POINT ( 'NONE',  ( -6.220909254589682469, 215.4770327129946850, 29.94886208192142973 ) ) ;
#1692 = EDGE_CURVE ( 'NONE', #30073, #15658, #28705, .T. ) ;
#1693 = CARTESIAN_POINT ( 'NONE',  ( 6.499999999999999112, -3.752776749732576356, -0.8000000000000003775 ) ) ;
#1694 = VERTEX_POINT ( 'NONE', #5033 ) ;
#1695 = VERTEX_POINT ( 'NONE', #5196 ) ;
#1696 = CARTESIAN_POINT ( 'NONE',  ( 6.220909254589536808, 215.4770327129947702, 91.55113791807858092 ) ) ;
#1697 = ORIENTED_EDGE ( 'NONE', *, *, #213, .F. ) ;
#1698 = CARTESIAN_POINT ( 'NONE',  ( 87.49999999999995737, 167.3752416915453125, -9.523985490255702402 ) ) ;
#1699 = FACE_BOUND ( 'NONE', #15661, .T. ) ;
#1700 = ORIENTED_EDGE ( 'NONE', *, *, #14373, .T. ) ;
#1701 = CARTESIAN_POINT ( 'NONE',  ( -2.426778023690262742, 214.6231898156240163, 28.10113791807856742 ) ) ;
#1702 = CARTESIAN_POINT ( 'NONE',  ( 127.5000000000000000, 155.0000000000000000, -6.938893903907228378E-15 ) ) ;
#1703 = CARTESIAN_POINT ( 'NONE',  ( 10.00000000000000711, 207.0476921513415220, 15.99886208192143400 ) ) ;
#1704 = CARTESIAN_POINT ( 'NONE',  ( 58.27499999726880731, 160.0630714827496206, 15.58253174999999224 ) ) ;
#1705 = EDGE_LOOP ( 'NONE', ( #13701, #14443, #3420, #26950 ) ) ;
#1706 = CARTESIAN_POINT ( 'NONE',  ( -4.984841277089726574, 200.2242689037092305, 48.05113791807858092 ) ) ;
#1707 = DIRECTION ( 'NONE',  ( 1.000000000000000000, 0.000000000000000000, 0.000000000000000000 ) ) ;
#1708 = CARTESIAN_POINT ( 'NONE',  ( 4.000000000000003553, 0.000000000000000000, 0.000000000000000000 ) ) ;
#1709 = CARTESIAN_POINT ( 'NONE',  ( -8.118202686958138514, 212.8392687619910930, 95.79886208192144181 ) ) ;
#1710 = CARTESIAN_POINT ( 'NONE',  ( 67.57499999726881867, 164.1591823560292198, -12.60653300113719766 ) ) ;
#1711 = CARTESIAN_POINT ( 'NONE',  ( 8.062137200540920645, 201.0835637161417822, 29.30113791807857027 ) ) ;
#1712 = DIRECTION ( 'NONE',  ( 1.000000000000000000, 0.000000000000000000, 0.000000000000000000 ) ) ;
#1713 = CARTESIAN_POINT ( 'NONE',  ( 6.139770520408368348, 198.4640165459539674, 20.45113791807855819 ) ) ;
#1714 = DIRECTION ( 'NONE',  ( 1.000000000000000000, 0.000000000000000000, 0.000000000000000000 ) ) ;
#1715 = CARTESIAN_POINT ( 'NONE',  ( 82.00000000000001421, 139.7537977485451393, -4.138211985947621020E-15 ) ) ;
#1716 = CARTESIAN_POINT ( 'NONE',  ( -56.01643337169826964, 194.9989636249862599, -0.3293050612182487069 ) ) ;
#1717 = CARTESIAN_POINT ( 'NONE',  ( -68.50000000000000000, 215.0000000000000000, 0.000000000000000000 ) ) ;
#1718 = CARTESIAN_POINT ( 'NONE',  ( -9.736236675707914401, 199.9851607334237542, 0.2011379180785655418 ) ) ;
#1719 = DIRECTION ( 'NONE',  ( 0.000000000000000000, 0.000000000000000000, 1.000000000000000000 ) ) ;
#1720 = CARTESIAN_POINT ( 'NONE',  ( 44.97499999726881015, 140.1801316387863778, -4.815267126137194431 ) ) ;
#1721 = CARTESIAN_POINT ( 'NONE',  ( -8.062137200540920645, 212.9164362838581894, 42.80113791807857382 ) ) ;
#1722 = CARTESIAN_POINT ( 'NONE',  ( 83.02499999726879309, 149.9369285172503510, -15.58253175000000823 ) ) ;
#1723 = DIRECTION ( 'NONE',  ( -1.000000000000000000, -0.000000000000000000, -0.000000000000000000 ) ) ;
#1724 = CARTESIAN_POINT ( 'NONE',  ( 108.0049454219347354, 155.0000000000000000, 0.000000000000000000 ) ) ;
#1725 = CARTESIAN_POINT ( 'NONE',  ( 45.09999999453763309, 150.2886644046228639, 14.49999999999999645 ) ) ;
#1726 = ORIENTED_EDGE ( 'NONE', *, *, #20401, .F. ) ;
#1727 = CARTESIAN_POINT ( 'NONE',  ( 12.01549611932652972, 210.8513442034534933, 28.85113791807856032 ) ) ;
#1728 = CARTESIAN_POINT ( 'NONE',  ( -64.50000000000000000, -2.605762844159085212, -20.00000000000000000 ) ) ;
#1729 = CARTESIAN_POINT ( 'NONE',  ( -6.139770520408224463, 198.4640165459539389, 2.048862081921434264 ) ) ;
#1730 = CARTESIAN_POINT ( 'NONE',  ( 73.71132485994280614, 155.0000000000000000, -15.00000000000002487 ) ) ;
#1731 = ORIENTED_EDGE ( 'NONE', *, *, #24172, .F. ) ;
#1732 = AXIS2_PLACEMENT_3D ( 'NONE', #9905, #7356, #27280 ) ;
#1733 = CARTESIAN_POINT ( 'NONE',  ( 64.50000000000000000, 0.000000000000000000, 30.00000000000000000 ) ) ;
#1734 = CARTESIAN_POINT ( 'NONE',  ( 0.05014649552810505201, 217.5146222423826714, 64.25113791807856956 ) ) ;
#1735 =( BOUNDED_CURVE ( )  B_SPLINE_CURVE ( 3, ( #25427, #23389, #4815, #2266 ),
 .UNSPECIFIED., .F., .T. ) 
 B_SPLINE_CURVE_WITH_KNOTS ( ( 4, 4 ),
 ( 5.758306373677911871, 6.283185307179586232 ),
 .UNSPECIFIED. ) 
 CURVE ( )  GEOMETRIC_REPRESENTATION_ITEM ( )  RATIONAL_B_SPLINE_CURVE ( ( 1.000000000000000000, 0.9771733092046011038, 0.9771733092046011038, 1.000000000000000000 ) ) 
 REPRESENTATION_ITEM ( '' )  );
#1736 = CARTESIAN_POINT ( 'NONE',  ( 0.05014649552828262524, 198.5883022060938572, 19.74886208192143400 ) ) ;
#1737 = DIRECTION ( 'NONE',  ( -0.000000000000000000, -0.000000000000000000, -1.000000000000000000 ) ) ;
#1738 = EDGE_LOOP ( 'NONE', ( #5719, #22132, #19511, #15323 ) ) ;
#1739 = TOROIDAL_SURFACE ( 'NONE', #20227, 5.400000000000002132, 0.4000000000000000222 ) ;
#1740 = CARTESIAN_POINT ( 'NONE',  ( -7.984503880673488041, 209.6470497212046098, 0.6511379180785660248 ) ) ;
#1741 = FACE_OUTER_BOUND ( 'NONE', #4713, .T. ) ;
#1742 = CARTESIAN_POINT ( 'NONE',  ( 7.375838497908012492, 217.2372850707501186, 87.54886208192142760 ) ) ;
#1743 = CARTESIAN_POINT ( 'NONE',  ( 37.47499999726880304, 160.0630714827496206, -15.58253175000000823 ) ) ;
#1744 = ORIENTED_EDGE ( 'NONE', *, *, #31666, .F. ) ;
#1745 = CARTESIAN_POINT ( 'NONE',  ( 45.02499999726880731, 149.9369285172503510, -15.58253175000000823 ) ) ;
#1746 = CARTESIAN_POINT ( 'NONE',  ( 38.88867513459482694, 159.8737954434936057, -15.00000000000002665 ) ) ;
#1747 = CARTESIAN_POINT ( 'NONE',  ( 6.139770520408368348, 198.4640165459539674, -0.5488620819214343749 ) ) ;
#1748 = CARTESIAN_POINT ( 'NONE',  ( -8.118202686958138514, 212.8392687619910930, 68.79886208192144181 ) ) ;
#1749 = CARTESIAN_POINT ( 'NONE',  ( 42.77499999726880731, 140.1801316387863778, 4.815267126137185549 ) ) ;
#1750 = CARTESIAN_POINT ( 'NONE',  ( 1.153701847711638750, 3.375361811986500538, 1.891580053702728746E-15 ) ) ;
#1751 = CARTESIAN_POINT ( 'NONE',  ( 0.05014649552810505201, 217.5146222423826714, 7.251137918078566003 ) ) ;
#1752 = DIRECTION ( 'NONE',  ( 0.000000000000000000, -0.7071067811865434649, 0.7071067811865515695 ) ) ;
#1753 = ADVANCED_FACE ( 'NONE', ( #12697 ), #31102, .F. ) ;
#1754 = AXIS2_PLACEMENT_3D ( 'NONE', #28551, #10494, #15753 ) ;
#1755 = CARTESIAN_POINT ( 'NONE',  ( 62.39999999999999858, 150.2886644046228639, -14.50000000000000888 ) ) ;
#1756 = CARTESIAN_POINT ( 'NONE',  ( 10.01549611932653860, 210.2015048109876716, 85.85113791807857808 ) ) ;
#1757 = CARTESIAN_POINT ( 'NONE',  ( -119.7500000000000000, 0.000000000000000000, -35.00000000000000000 ) ) ;
#1758 = CARTESIAN_POINT ( 'NONE',  ( -6.500168698208244500, 211.6636982574061676, 86.79886208192142760 ) ) ;
#1759 = CARTESIAN_POINT ( 'NONE',  ( -7.298354728638373423, 4.926141412641537265, -7.913704048100170141 ) ) ;
#1760 = DIRECTION ( 'NONE',  ( -1.000000000000000000, 0.000000000000000000, -0.000000000000000000 ) ) ;
#1761 = CARTESIAN_POINT ( 'NONE',  ( -9.736236675708031640, 214.0148392665760753, 83.79886208192144181 ) ) ;
#1762 = CARTESIAN_POINT ( 'NONE',  ( 61.92499999726882010, 164.1591823560292198, 12.60653300113718167 ) ) ;
#1764 = ORIENTED_EDGE ( 'NONE', *, *, #27471, .F. ) ;
#1763 = CARTESIAN_POINT ( 'NONE',  ( -6.220909254589537696, 198.5229672870051445, 18.05113791807856671 ) ) ;
#1765 = CARTESIAN_POINT ( 'NONE',  ( 42.71132485994280614, 155.0000000000000000, 15.00000000000001243 ) ) ;
#1766 = CIRCLE ( 'NONE', #13181, 5.200000000000009948 ) ;
#1767 = CARTESIAN_POINT ( 'NONE',  ( 80.27499999726879309, 160.0630714827496206, 15.58253174999999402 ) ) ;
#1768 = CARTESIAN_POINT ( 'NONE',  ( 7.456977232089302632, 217.1783343296989131, 82.55113791807858092 ) ) ;
#1769 = CARTESIAN_POINT ( 'NONE',  ( -9.996365641501871124, 207.8097375604742467, 102.5363179372327096 ) ) ;
#1770 = ORIENTED_EDGE ( 'NONE', *, *, #945, .T. ) ;
#1771 = CARTESIAN_POINT ( 'NONE',  ( 0.05014649552828288198, 194.3824533091408000, 67.74886208192143044 ) ) ;
#1772 = CARTESIAN_POINT ( 'NONE',  ( -10.00000000000000711, 206.9523078486584495, 80.49886208192143044 ) ) ;
#1773 = CARTESIAN_POINT ( 'NONE',  ( -7.456977232089471386, 217.1783343296987709, 14.94886208192143506 ) ) ;
#1774 = CARTESIAN_POINT ( 'NONE',  ( -27.50000000000000000, -13.28298644054430611, -16.25870334244831383 ) ) ;
#1775 = CARTESIAN_POINT ( 'NONE',  ( 10.00000000000000711, 206.9523078486586201, 29.00113791807856956 ) ) ;
#1776 = EDGE_LOOP ( 'NONE', ( #1876, #22480, #11969, #27098 ) ) ;
#1777 = CARTESIAN_POINT ( 'NONE',  ( 10.00000000000000711, 207.0476921513415220, 93.99886208192144466 ) ) ;
#1778 = CIRCLE ( 'NONE', #1251, 12.00000000000001066 ) ;
#1779 = CARTESIAN_POINT ( 'NONE',  ( 2.075968632158072591, 6.306992450858666110, -6.056431503347234013 ) ) ;
#1780 = VERTEX_POINT ( 'NONE', #30592 ) ;
#1781 = DIRECTION ( 'NONE',  ( 0.000000000000000000, 0.8660254037844379305, -0.5000000000000014433 ) ) ;
#1782 = CARTESIAN_POINT ( 'NONE',  ( 7.984503880673422316, 209.6470497212048372, 81.84886208192142476 ) ) ;
#1783 = ORIENTED_EDGE ( 'NONE', *, *, #27467, .F. ) ;
#1784 = CARTESIAN_POINT ( 'NONE',  ( 81.32499999726880446, 164.1591823560292198, -12.60653300113719766 ) ) ;
#1785 = VERTEX_POINT ( 'NONE', #28376 ) ;
#1786 = CARTESIAN_POINT ( 'NONE',  ( 4.000000000000000000, -1.759474945355388176, -3.047499999999998099 ) ) ;
#1787 = CONICAL_SURFACE ( 'NONE', #24631, 32.10452846326766974, 1.466076571675243523 ) ;
#1788 = AXIS2_PLACEMENT_3D ( 'NONE', #23905, #3451, #6004 ) ;
#1789 = CARTESIAN_POINT ( 'NONE',  ( 75.92499999726881299, 164.1591823560292198, 12.60653300113718167 ) ) ;
#1790 = CARTESIAN_POINT ( 'NONE',  ( 53.78867513459483263, 155.0000000000000000, 15.00000000000001243 ) ) ;
#1791 = CARTESIAN_POINT ( 'NONE',  ( 2.517493886308900919, 214.5937144450984420, 76.40113791807856103 ) ) ;
#1792 = CARTESIAN_POINT ( 'NONE',  ( -3.500000000000000888, 1.362959798491825802, -2.760265505016211041 ) ) ;
#1793 = ADVANCED_FACE ( 'NONE', ( #14914 ), #12360, .F. ) ;
#1794 = CIRCLE ( 'NONE', #11597, 18.00000000000000711 ) ;
#1795 = CARTESIAN_POINT ( 'NONE',  ( 43.80000000000001137, 142.6655632788954620, 8.961492836873471646 ) ) ;
#1796 = CARTESIAN_POINT ( 'NONE',  ( -0.05014649552828365914, 215.4116977939061144, 57.24886208192145887 ) ) ;
#1797 = EDGE_CURVE ( 'NONE', #31418, #32263, #7015, .T. ) ;
#1798 = ADVANCED_FACE ( 'NONE', ( #23430, #1969 ), #93, .T. ) ;
#1799 = AXIS2_PLACEMENT_3D ( 'NONE', #12760, #28432, #33539 ) ;
#1800 = CARTESIAN_POINT ( 'NONE',  ( -27.50000000000000000, 15.87713240271469672, -18.00000000000000000 ) ) ;
#1801 = CARTESIAN_POINT ( 'NONE',  ( 117.5000000000000000, 61.05130719884917312, -52.99999999999945999 ) ) ;
#1802 = DIRECTION ( 'NONE',  ( 1.000000000000000000, -0.000000000000000000, -0.000000000000000000 ) ) ;
#1803 = CARTESIAN_POINT ( 'NONE',  ( 49.32499999726881157, 164.1591823560292198, -12.60653300113719766 ) ) ;
#1804 = CARTESIAN_POINT ( 'NONE',  ( 62.87499999726881583, 138.6155565068815463, -3.929120461958505118E-15 ) ) ;
#1805 = CARTESIAN_POINT ( 'NONE',  ( 7.375838497908181246, 196.7627149292499666, 53.45113791807857240 ) ) ;
#1806 = CARTESIAN_POINT ( 'NONE',  ( 40.71132485994280614, 155.0000000000000000, 15.00000000000001243 ) ) ;
#1807 = CARTESIAN_POINT ( 'NONE',  ( -11.98450388067348804, 210.9467285061362247, 0.6511379180785656917 ) ) ;
#1809 = CARTESIAN_POINT ( 'NONE',  ( 3.135527875058820690, 216.4958274776887492, 82.40113791807857524 ) ) ;
#1808 =( REPRESENTATION_RELATIONSHIP ('NONE','NONE', #25663, #30243 ) REPRESENTATION_RELATIONSHIP_WITH_TRANSFORMATION ( #32342 )SHAPE_REPRESENTATION_RELATIONSHIP( ) );
#1810 = CARTESIAN_POINT ( 'NONE',  ( -12.01549611932659722, 210.8513442034533227, 41.64886208192143613 ) ) ;
#1811 = CARTESIAN_POINT ( 'NONE',  ( 10.01549611932659367, 203.7984951890124421, 43.14886208192142902 ) ) ;
#1812 = CARTESIAN_POINT ( 'NONE',  ( -6.500000000000000000, 0.3213925021621126255, 6.556035011748282652E-16 ) ) ;
#1813 = AXIS2_PLACEMENT_3D ( 'NONE', #4996, #18112, #8223 ) ;
#1814 = CARTESIAN_POINT ( 'NONE',  ( 9.736236675707914401, 214.0148392665762458, 82.70113791807858661 ) ) ;
#1815 = CARTESIAN_POINT ( 'NONE',  ( 83.51132485994280330, 146.1832212156128890, -12.13525491562423042 ) ) ;
#1816 = CARTESIAN_POINT ( 'NONE',  ( -8.062137200540920645, 212.9164362838581894, 6.801137918078565825 ) ) ;
#1817 = CIRCLE ( 'NONE', #3443, 69.99999999999998579 ) ;
#1818 = EDGE_CURVE ( 'NONE', #1032, #16785, #2654, .T. ) ;
#1819 = CARTESIAN_POINT ( 'NONE',  ( -3.044812012439970683, 197.4746971517856196, 64.89886208192145034 ) ) ;
#1820 = CARTESIAN_POINT ( 'NONE',  ( 4.000000000000000000, 0.000000000000000000, 0.000000000000000000 ) ) ;
#1821 = EDGE_LOOP ( 'NONE', ( #1119, #3453 ) ) ;
#1822 = CARTESIAN_POINT ( 'NONE',  ( -7.456977232089471386, 217.1783343296987709, 74.94886208192143329 ) ) ;
#1823 = ORIENTED_EDGE ( 'NONE', *, *, #23098, .F. ) ;
#1824 = CARTESIAN_POINT ( 'NONE',  ( 80.87499999726881583, 138.6155565068815463, -3.929120461958505118E-15 ) ) ;
#1825 = CARTESIAN_POINT ( 'NONE',  ( -6.500168698208244500, 211.6636982574061676, 44.79886208192144181 ) ) ;
#1826 = EDGE_CURVE ( 'NONE', #26666, #33208, #33149, .T. ) ;
#1827 = ORIENTED_EDGE ( 'NONE', *, *, #20796, .F. ) ;
#1828 = CARTESIAN_POINT ( 'NONE',  ( 84.67499999726881299, 141.7447067706911810, 9.630534252274376428 ) ) ;
#1829 = CARTESIAN_POINT ( 'NONE',  ( -64.50000000000000000, 120.3589838486224579, -20.00000000000000000 ) ) ;
#1830 = PRESENTATION_LAYER_ASSIGNMENT (  '', '', ( #7833 ) ) ;
#1831 = CARTESIAN_POINT ( 'NONE',  ( 115.4999999999999858, 102.0000000000001990, 91.79869280115065067 ) ) ;
#1832 = STYLED_ITEM ( 'NONE', ( #2148 ), #15696 ) ;
#1833 = CARTESIAN_POINT ( 'NONE',  ( 55.12499999726881583, 155.0000000000000000, -15.58253175000000823 ) ) ;
#1834 = CARTESIAN_POINT ( 'NONE',  ( 87.50000000000001421, 155.0000000000000000, -6.938893903907228378E-15 ) ) ;
#1835 = ADVANCED_FACE ( 'NONE', ( #28027 ), #9738, .T. ) ;
#1836 = CARTESIAN_POINT ( 'NONE',  ( 3.135527875058981895, 197.5041725223112792, 40.59886208192143187 ) ) ;
#1837 = ORIENTED_EDGE ( 'NONE', *, *, #29441, .F. ) ;
#1838 = DIRECTION ( 'NONE',  ( 1.000000000000000000, 0.000000000000000000, 0.000000000000000000 ) ) ;
#1839 = AXIS2_PLACEMENT_3D ( 'NONE', #32751, #17255, #22197 ) ;
#1840 = CYLINDRICAL_SURFACE ( 'NONE', #11781, 12.00000000000000355 ) ;
#1841 = LINE ( 'NONE', #32841, #7687 ) ;
#1842 = CARTESIAN_POINT ( 'NONE',  ( -2.426778023690076225, 199.3768101843759553, 22.89886208192143613 ) ) ;
#1843 = AXIS2_PLACEMENT_3D ( 'NONE', #19421, #29826, #6487 ) ;
#1844 = CARTESIAN_POINT ( 'NONE',  ( 3.044812012440130555, 197.4746971517856764, 59.60113791807857808 ) ) ;
#1845 = CARTESIAN_POINT ( 'NONE',  ( -8.118202686958039038, 201.1607312380087080, 48.20113791807857950 ) ) ;
#1846 = CARTESIAN_POINT ( 'NONE',  ( 10.01549611932653860, 210.2015048109876716, 13.85113791807856742 ) ) ;
#1847 = CARTESIAN_POINT ( 'NONE',  ( -8.015496119326531499, 204.4483345814780364, 3.351137918078566535 ) ) ;
#1848 = CARTESIAN_POINT ( 'NONE',  ( 45.52499999726881441, 169.8198683612136222, -4.815267126137197984 ) ) ;
#1849 = CARTESIAN_POINT ( 'NONE',  ( -54.50000000000002132, 155.0000000000000000, 17.00000000000001421 ) ) ;
#1850 = CARTESIAN_POINT ( 'NONE',  ( -125.0000000000000000, 0.000000000000000000, -35.00000000000000000 ) ) ;
#1851 = CARTESIAN_POINT ( 'NONE',  ( 0.05014649552807549926, 219.6175466908591716, 28.25113791807856245 ) ) ;
#1852 = DIRECTION ( 'NONE',  ( 1.000000000000000000, 0.000000000000000000, 0.000000000000000000 ) ) ;
#1853 = EDGE_CURVE ( 'NONE', #10439, #8233, #21818, .T. ) ;
#1854 = CARTESIAN_POINT ( 'NONE',  ( 3.044812012440130555, 197.4746971517856764, 74.60113791807856387 ) ) ;
#1855 = CARTESIAN_POINT ( 'NONE',  ( 6.139770520408367460, 198.4640165459539389, 50.45113791807857240 ) ) ;
#1856 = LINE ( 'NONE', #6799, #28999 ) ;
#1857 = MECHANICAL_DESIGN_GEOMETRIC_PRESENTATION_REPRESENTATION (  '', ( #32884 ), #26900 ) ;
#1858 = CARTESIAN_POINT ( 'NONE',  ( 85.18867513459483121, 169.2658477444273331, -4.635254915624224203 ) ) ;
#1859 = CARTESIAN_POINT ( 'NONE',  ( 11.98450388067341876, 210.9467285061363953, 9.848862081921433642 ) ) ;
#1860 = CARTESIAN_POINT ( 'NONE',  ( -6.220909254589682469, 215.4770327129947134, 14.94886208192143329 ) ) ;
#1861 = CARTESIAN_POINT ( 'NONE',  ( 72.49999999453761745, 170.2462022514548323, -7.872454543227099337E-15 ) ) ;
#1862 = ORIENTED_EDGE ( 'NONE', *, *, #7924, .F. ) ;
#1863 = CARTESIAN_POINT ( 'NONE',  ( -3.753561863808691168, 195.6020594897209435, 62.90113791807858945 ) ) ;
#1864 = CARTESIAN_POINT ( 'NONE',  ( -6.500168698208129925, 202.3363017425936050, 78.20113791807857240 ) ) ;
#1865 = ADVANCED_FACE ( 'NONE', ( #6145 ), #11765, .F. ) ;
#1866 = CARTESIAN_POINT ( 'NONE',  ( -6.220909254589682469, 215.4770327129946850, 38.94886208192144039 ) ) ;
#1867 = CARTESIAN_POINT ( 'NONE',  ( -9.521242624480144912, 207.9188892840786878, 102.6634595774070533 ) ) ;
#1868 = ORIENTED_EDGE ( 'NONE', *, *, #27409, .F. ) ;
#1869 = COLOUR_RGB ( '', 0.72549020, 0.75294118, 0.79215686) ;
#1870 = ORIENTED_EDGE ( 'NONE', *, *, #28229, .F. ) ;
#1871 = AXIS2_PLACEMENT_3D ( 'NONE', #22106, #6777, #17162 ) ;
#1872 = ADVANCED_FACE ( 'NONE', ( #26935 ), #1377, .T. ) ;
#1873 = ORIENTED_EDGE ( 'NONE', *, *, #10837, .T. ) ;
#1874 = CYLINDRICAL_SURFACE ( 'NONE', #16753, 15.00000000000001776 ) ;
#1875 = CARTESIAN_POINT ( 'NONE',  ( 2.688402820137697713, 5.953403407568487182, -0.01956314070068190455 ) ) ;
#1876 = ORIENTED_EDGE ( 'NONE', *, *, #16847, .F. ) ;
#1877 = CARTESIAN_POINT ( 'NONE',  ( 2.426778023690261410, 199.3768101843759837, 32.60113791807857098 ) ) ;
#1878 = ADVANCED_BREP_SHAPE_REPRESENTATION ( '', ( #12506, #2404 ), #25772 ) ;
#1879 = CYLINDRICAL_SURFACE ( 'NONE', #10188, 2.000000000000000888 ) ;
#1880 = CARTESIAN_POINT ( 'NONE',  ( -3.135527875058982783, 216.4958274776886924, 12.09886208192143542 ) ) ;
#1881 = CARTESIAN_POINT ( 'NONE',  ( 53.57499999726881157, 164.1591823560292198, -12.60653300113719766 ) ) ;
#1882 = ORIENTED_EDGE ( 'NONE', *, *, #28419, .T. ) ;
#1883 = CARTESIAN_POINT ( 'NONE',  ( -2.517493886308901807, 199.4062855549015012, 47.90113791807857524 ) ) ;
#1884 = LINE ( 'NONE', #12269, #30881 ) ;
#1885 =( GEOMETRIC_REPRESENTATION_CONTEXT ( 3 ) GLOBAL_UNCERTAINTY_ASSIGNED_CONTEXT ( ( #2920 ) ) GLOBAL_UNIT_ASSIGNED_CONTEXT ( ( #133, #15793, #15959 ) ) REPRESENTATION_CONTEXT ( 'NONE', 'WORKASPACE' ) );
#1886 = DIRECTION ( 'NONE',  ( 1.000000000000000000, 0.000000000000000000, 0.000000000000000000 ) ) ;
#1887 = CARTESIAN_POINT ( 'NONE',  ( -3.135527875058982783, 216.4958274776886924, 102.0988620819214390 ) ) ;
#1888 = CARTESIAN_POINT ( 'NONE',  ( 66.47499999726882436, 149.9369285172503510, 15.58253174999999580 ) ) ;
#1889 = CARTESIAN_POINT ( 'NONE',  ( -6.139770520408369237, 215.5359834540460042, 27.95113791807856174 ) ) ;
#1890 = DIRECTION ( 'NONE',  ( 0.000000000000000000, -0.7071067811865442421, 0.7071067811865506814 ) ) ;
#1891 = CARTESIAN_POINT ( 'NONE',  ( 6.139770520408368348, 198.4640165459539674, 17.45113791807855819 ) ) ;
#1892 = DIRECTION ( 'NONE',  ( 0.000000000000000000, 0.000000000000000000, 1.000000000000000000 ) ) ;
#1893 = CARTESIAN_POINT ( 'NONE',  ( 80.90000000000000568, 168.7903194862797420, -4.480746418436745593 ) ) ;
#1894 = CARTESIAN_POINT ( 'NONE',  ( -58.17468396801123731, 194.9227987135369062, -2.484183799773476142 ) ) ;
#1895 = CARTESIAN_POINT ( 'NONE',  ( -1.860983896653666838E-15, 7.693909156113836190, -6.460786012259834621 ) ) ;
#1896 = CARTESIAN_POINT ( 'NONE',  ( 3.662846001190051659, 195.5725841191953691, -0.3988620819214345747 ) ) ;
#1897 = DIRECTION ( 'NONE',  ( 0.000000000000000000, 0.000000000000000000, 1.000000000000000000 ) ) ;
#1898 = CARTESIAN_POINT ( 'NONE',  ( 48.97499999726881725, 140.1801316387863778, -4.815267126137194431 ) ) ;
#1899 = EDGE_CURVE ( 'NONE', #16312, #19546, #5899, .T. ) ;
#1900 = CARTESIAN_POINT ( 'NONE',  ( -6.220909254589537696, 198.5229672870051161, 51.05113791807856671 ) ) ;
#1901 = EDGE_CURVE ( 'NONE', #253, #21688, #5459, .T. ) ;
#1902 = CARTESIAN_POINT ( 'NONE',  ( 81.02499999726880731, 149.9369285172503510, -15.58253175000000823 ) ) ;
#1903 = DIRECTION ( 'NONE',  ( 0.000000000000000000, 2.081668171172168119E-15, -1.000000000000000000 ) ) ;
#1904 = FACE_BOUND ( 'NONE', #21541, .T. ) ;
#1905 = CARTESIAN_POINT ( 'NONE',  ( 51.69999999453762030, 142.6655632788954620, -8.961492836873480528 ) ) ;
#1906 = EDGE_LOOP ( 'NONE', ( #30932, #13807 ) ) ;
#1907 = CARTESIAN_POINT ( 'NONE',  ( -9.680171189290831535, 214.0920067884431148, 24.80113791807857027 ) ) ;
#1908 = PRODUCT_DEFINITION ( 'UNKNOWN', '', #31143, #19299 ) ;
#1909 = ADVANCED_FACE ( 'NONE', ( #26594 ), #24551, .F. ) ;
#1910 = CARTESIAN_POINT ( 'NONE',  ( -11.00000000000000355, 206.9999999999998863, 103.5000000000000142 ) ) ;
#1911 = CARTESIAN_POINT ( 'NONE',  ( 10.01549611932659545, 203.7984951890123853, 7.148862081921433465 ) ) ;
#1912 = CARTESIAN_POINT ( 'NONE',  ( 100.4058500716420781, 155.0000000000000000, 0.000000000000000000 ) ) ;
#1913 = EDGE_LOOP ( 'NONE', ( #27322, #2739, #32652 ) ) ;
#1914 = LINE ( 'NONE', #1733, #4519 ) ;
#1915 = CARTESIAN_POINT ( 'NONE',  ( -3.135527875058821579, 197.5041725223112223, 62.90113791807858235 ) ) ;
#1916 = VERTEX_POINT ( 'NONE', #11603 ) ;
#1917 = CARTESIAN_POINT ( 'NONE',  ( 2.426778023690075337, 214.6231898156240447, 21.39886208192143613 ) ) ;
#1918 = DIRECTION ( 'NONE',  ( 0.000000000000000000, 0.000000000000000000, -1.000000000000000000 ) ) ;
#1919 = ORIENTED_EDGE ( 'NONE', *, *, #8328, .F. ) ;
#1920 = CARTESIAN_POINT ( 'NONE',  ( 8.000000000000008882, 206.9523078486586485, 2.001137918078566003 ) ) ;
#1921 = CARTESIAN_POINT ( 'NONE',  ( -3.093157300003891663, -6.874418838041293611, -6.051203375184721622E-15 ) ) ;
#1922 = CARTESIAN_POINT ( 'NONE',  ( 3.753561863808876797, 195.6020594897209719, 91.59886208192145318 ) ) ;
#1923 = CARTESIAN_POINT ( 'NONE',  ( 36.37499999726881583, 155.0000000000000000, 15.58253174999999402 ) ) ;
#1924 = ORIENTED_EDGE ( 'NONE', *, *, #23365, .F. ) ;
#1925 = CARTESIAN_POINT ( 'NONE',  ( 44.82499999726880446, 141.7447067706911810, -9.630534252274385310 ) ) ;
#1926 = FACE_OUTER_BOUND ( 'NONE', #26468, .T. ) ;
#1927 = CARTESIAN_POINT ( 'NONE',  ( 0.05014649552810505201, 217.5146222423826714, 1.251137918078566003 ) ) ;
#1928 = CARTESIAN_POINT ( 'NONE',  ( 8.118202686958138514, 201.1607312380088501, 73.29886208192142760 ) ) ;
#1929 = CARTESIAN_POINT ( 'NONE',  ( 46.07499999726881157, 168.2552932293087906, 9.630534252274372875 ) ) ;
#1930 = FACE_OUTER_BOUND ( 'NONE', #19675, .T. ) ;
#1931 = CARTESIAN_POINT ( 'NONE',  ( 0.05014649552810505201, 217.5146222423826714, 4.251137918078566003 ) ) ;
#1932 = CARTESIAN_POINT ( 'NONE',  ( -3.499999999999999556, -3.004629197474309385E-15, 0.000000000000000000 ) ) ;
#1933 = CARTESIAN_POINT ( 'NONE',  ( 58.00000000000000711, 139.7537977485451393, -4.138211985947621020E-15 ) ) ;
#1934 = CARTESIAN_POINT ( 'NONE',  ( 10.00000000000000711, 206.9523078486586201, 86.00113791807858377 ) ) ;
#1935 = CARTESIAN_POINT ( 'NONE',  ( 64.51132485994280330, 163.8167787843871110, 12.13525491562421621 ) ) ;
#1936 = CARTESIAN_POINT ( 'NONE',  ( 6.139770520408368348, 198.4640165459539674, 71.45113791807857240 ) ) ;
#1937 = CARTESIAN_POINT ( 'NONE',  ( 145.0000000000000000, 3.306546357697854049E-14, 20.00000000000000000 ) ) ;
#1938 = DIRECTION ( 'NONE',  ( -2.312964634635740985E-16, 1.000000000000000000, 0.000000000000000000 ) ) ;
#1939 = CARTESIAN_POINT ( 'NONE',  ( 11.98450388067341876, 210.9467285061363953, 87.84886208192142476 ) ) ;
#1940 = CARTESIAN_POINT ( 'NONE',  ( 64.52499999726882152, 140.1801316387863778, 4.815267126137185549 ) ) ;
#1942 = ORIENTED_EDGE ( 'NONE', *, *, #405, .T. ) ;
#1941 = CARTESIAN_POINT ( 'NONE',  ( -8.062137200540920645, 212.9164362838581894, 21.80113791807856671 ) ) ;
#1943 = DIRECTION ( 'NONE',  ( 0.000000000000000000, 0.000000000000000000, -1.000000000000000000 ) ) ;
#1944 = CARTESIAN_POINT ( 'NONE',  ( 85.27499999726879309, 149.9369285172503510, -15.58253175000000823 ) ) ;
#1945 = B_SPLINE_CURVE_WITH_KNOTS ( 'NONE', 3,
 ( #9290, #30425, #17302, #1298, #1458, #19684 ),
 .UNSPECIFIED., .F., .F.,
 ( 4, 2, 4 ),
 ( 2.380727408830323507E-07, 0.008032766472079741829, 0.01606529487141860127 ),
 .UNSPECIFIED. ) ;
#1946 = CARTESIAN_POINT ( 'NONE',  ( 3.753561863808689836, 218.3979405102790565, 88.40113791807857524 ) ) ;
#1947 =( BOUNDED_CURVE ( )  B_SPLINE_CURVE ( 2, ( #1623, #11852, #32626, #14569, #8783, #11349, #4013, #12013, #21730, #19682, #1123 ),
 .UNSPECIFIED., .F., .T. ) 
 B_SPLINE_CURVE_WITH_KNOTS ( ( 3, 2, 2, 2, 2, 3 ),
 ( 0.3214285714285712303, 0.3249999999999997891, 0.3285714285714283478, 0.3321428571428569620, 0.3357142857142855208, 0.3392857142857140795 ),
 .UNSPECIFIED. ) 
 CURVE ( )  GEOMETRIC_REPRESENTATION_ITEM ( )  RATIONAL_B_SPLINE_CURVE ( ( 1.000000000000002220, 0.9510565162951510887, 1.000000000000000000, 0.9510565162951534202, 1.000000000000000000, 0.9510565162951534202, 1.000000000000000000, 0.9510565162951534202, 1.000000000000000000, 0.9510565162951549745, 0.9999999999999984457 ) ) 
 REPRESENTATION_ITEM ( '' )  );
#1948 = DIRECTION ( 'NONE',  ( -1.000000000000000000, 0.000000000000000000, 0.000000000000000000 ) ) ;
#1949 = ORIENTED_EDGE ( 'NONE', *, *, #15619, .F. ) ;
#1950 = CARTESIAN_POINT ( 'NONE',  ( 3.753561863808876797, 195.6020594897209719, 73.59886208192142476 ) ) ;
#1951 = CARTESIAN_POINT ( 'NONE',  ( 10.00000000000000711, 207.0476921513415220, 78.99886208192144466 ) ) ;
#1952 = CARTESIAN_POINT ( 'NONE',  ( -7.375838497908014268, 196.7627149292498530, 14.04886208192143471 ) ) ;
#1953 = CARTESIAN_POINT ( 'NONE',  ( 1.650000000000000133, 0.000000000000000000, -2.899999999999999911 ) ) ;
#1954 = CARTESIAN_POINT ( 'NONE',  ( -8.118202686958039038, 201.1607312380087080, 30.20113791807856884 ) ) ;
#1955 = CARTESIAN_POINT ( 'NONE',  ( 77.50000000000000000, 155.0000000000000000, -15.50000000000001776 ) ) ;
#1956 = CARTESIAN_POINT ( 'NONE',  ( -6.139770520408224463, 198.4640165459539389, 95.04886208192144181 ) ) ;
#1957 = FACE_OUTER_BOUND ( 'NONE', #2642, .T. ) ;
#1958 = EDGE_LOOP ( 'NONE', ( #3589, #13076, #7075, #26419 ) ) ;
#1959 = CARTESIAN_POINT ( 'NONE',  ( 69.81132485994281467, 159.8737954434934920, -15.00000000000012434 ) ) ;
#1960 = CARTESIAN_POINT ( 'NONE',  ( -6.500168698208244500, 211.6636982574061676, 77.79886208192142760 ) ) ;
#1961 = ORIENTED_EDGE ( 'NONE', *, *, #28033, .F. ) ;
#1962 = CARTESIAN_POINT ( 'NONE',  ( 3.500000000000004441, -0.6807265984995719554, -2.870648692803527524 ) ) ;
#1963 = ORIENTED_EDGE ( 'NONE', *, *, #19778, .T. ) ;
#1964 = DIRECTION ( 'NONE',  ( -0.000000000000000000, -0.000000000000000000, 1.000000000000000000 ) ) ;
#1965 = CARTESIAN_POINT ( 'NONE',  ( 73.27499999726882152, 149.9369285172503510, -15.58253175000000823 ) ) ;
#1966 = CARTESIAN_POINT ( 'NONE',  ( 81.22499999726882436, 160.0630714827496206, -15.58253175000000823 ) ) ;
#1967 = CARTESIAN_POINT ( 'NONE',  ( -0.3755270751584372513, 206.7692714347155629, 108.3323677711371573 ) ) ;
#1968 = CARTESIAN_POINT ( 'NONE',  ( 8.015496119326531499, 209.5516654185219636, 82.85113791807857808 ) ) ;
#1969 = FACE_OUTER_BOUND ( 'NONE', #1365, .T. ) ;
#1970 =( LENGTH_UNIT ( ) NAMED_UNIT ( * ) SI_UNIT ( .MILLI., .METRE. ) );
#1971 = CARTESIAN_POINT ( 'NONE',  ( 41.20000000000000284, 167.3344367211045096, 8.961492836873468093 ) ) ;
#1972 = CARTESIAN_POINT ( 'NONE',  ( -8.015496119326597224, 209.5516654185217362, 56.64886208192143613 ) ) ;
#1973 = VECTOR ( 'NONE', #1760, 1000.000000000000000 ) ;
#1974 = DIRECTION ( 'NONE',  ( 0.000000000000000000, 0.000000000000000000, 1.000000000000000000 ) ) ;
#1975 = DIRECTION ( 'NONE',  ( 1.000000000000000000, -0.000000000000000000, -0.000000000000000000 ) ) ;
#1976 = CARTESIAN_POINT ( 'NONE',  ( -119.7500000000000000, 0.6872233929727673551, 35.00001200000000523 ) ) ;
#1977 = CARTESIAN_POINT ( 'NONE',  ( 58.92499999726881299, 145.8408176439707802, -12.60653300113719588 ) ) ;
#1978 = CARTESIAN_POINT ( 'NONE',  ( 64.67499999726878457, 141.7447067706911810, 9.630534252274376428 ) ) ;
#1979 = CARTESIAN_POINT ( 'NONE',  ( -0.05014649552807705357, 194.3824533091408000, 59.75113791807856245 ) ) ;
#1980 = B_SPLINE_CURVE_WITH_KNOTS ( 'NONE', 3,
 ( #7965, #28407, #15284, #22954, #18350, #10189 ),
 .UNSPECIFIED., .F., .F.,
 ( 4, 2, 4 ),
 ( 0.004444412883774350592, 0.006655097293744440673, 0.008865781703714530754 ),
 .UNSPECIFIED. ) ;
#1981 = PLANE ( 'NONE',  #9716 ) ;
#1982 = CARTESIAN_POINT ( 'NONE',  ( 3.662846001190051659, 195.5725841191953691, 2.601137918078566091 ) ) ;
#1983 = CARTESIAN_POINT ( 'NONE',  ( 3.135527875058820690, 216.4958274776887492, 73.40113791807857524 ) ) ;
#1984 = VECTOR ( 'NONE', #1667, 1000.000000000000000 ) ;
#1985 = CARTESIAN_POINT ( 'NONE',  ( 12.00000000000000711, 207.0476921513415220, 42.99886208192143044 ) ) ;
#1986 = CARTESIAN_POINT ( 'NONE',  ( 8.118202686958138514, 201.1607312380088501, 43.29886208192143471 ) ) ;
#1987 = DIRECTION ( 'NONE',  ( 0.000000000000000000, -0.4999999999999990563, 0.8660254037844391517 ) ) ;
#1988 = CARTESIAN_POINT ( 'NONE',  ( 9.736236675707914401, 214.0148392665762458, 85.70113791807858661 ) ) ;
#1989 = CARTESIAN_POINT ( 'NONE',  ( 82.91132485994279477, 146.1832212156128890, 12.13525491562421976 ) ) ;
#1990 = CARTESIAN_POINT ( 'NONE',  ( 3.135527875058820690, 216.4958274776887492, 4.401137918078565470 ) ) ;
#1991 = CARTESIAN_POINT ( 'NONE',  ( -0.05014649552828403384, 217.5146222423826714, 72.24886208192140202 ) ) ;
#1992 = EDGE_CURVE ( 'NONE', #2597, #15105, #31874, .T. ) ;
#1993 = DIRECTION ( 'NONE',  ( 0.000000000000000000, 0.000000000000000000, -1.000000000000000000 ) ) ;
#1994 = ORIENTED_EDGE ( 'NONE', *, *, #18228, .F. ) ;
#1995 = CARTESIAN_POINT ( 'NONE',  ( -9.736236675708031640, 214.0148392665760753, 71.79886208192142760 ) ) ;
#1996 = ORIENTED_EDGE ( 'NONE', *, *, #12415, .T. ) ;
#1997 = CARTESIAN_POINT ( 'NONE',  ( 76.77499999726880731, 140.1801316387863778, 4.815267126137185549 ) ) ;
#1998 = CARTESIAN_POINT ( 'NONE',  ( -8.015496119326597224, 209.5516654185217362, 56.64886208192143613 ) ) ;
#1999 = VERTEX_POINT ( 'NONE', #16875 ) ;
#2000 = B_SPLINE_CURVE_WITH_KNOTS ( 'NONE', 3,
 ( #18159, #23925, #28554, #15585, #26152, #13043, #97, #10498 ),
 .UNSPECIFIED., .F., .F.,
 ( 4, 2, 2, 4 ),
 ( 0.02832689070575901413, 0.03234239231761928957, 0.03635789392947956500, 0.04438889715320012974 ),
 .UNSPECIFIED. ) ;
#2001 = CONICAL_SURFACE ( 'NONE', #14490, 27.50000000000000355, 1.047197551196595411 ) ;
#2002 = CARTESIAN_POINT ( 'NONE',  ( 71.52499999726882152, 169.8198683612136222, -4.815267126137197984 ) ) ;
#2003 = FACE_OUTER_BOUND ( 'NONE', #30107, .T. ) ;
#2004 = COLOUR_RGB ( '', 0.31764706, 0.68627451, 0.89019608) ;
#2005 = LINE ( 'NONE', #27383, #32872 ) ;
#2006 = CARTESIAN_POINT ( 'NONE',  ( 56.42499999726881299, 141.7447067706911810, 9.630534252274376428 ) ) ;
#2007 = DIRECTION ( 'NONE',  ( -1.000000000000000000, -0.000000000000000000, -0.000000000000000000 ) ) ;
#2008 = CARTESIAN_POINT ( 'NONE',  ( 9.984503880673420539, 210.2968891136705167, 39.84886208192141765 ) ) ;
#2009 = VERTEX_POINT ( 'NONE', #3424 ) ;
#2010 = AXIS2_PLACEMENT_3D ( 'NONE', #12064, #22453, #9339 ) ;
#2011 = CARTESIAN_POINT ( 'NONE',  ( 0.000000000000000000, 0.000000000000000000, 9.480888224575629408 ) ) ;
#2012 = CARTESIAN_POINT ( 'NONE',  ( 2.075968632162763061, -6.306992450856140131, -6.056431503344847478 ) ) ;
#2013 = FACE_OUTER_BOUND ( 'NONE', #29654, .T. ) ;
#2014 = CARTESIAN_POINT ( 'NONE',  ( -7.984503880673422316, 204.3529502787951628, 29.34886208192143897 ) ) ;
#2015 = CARTESIAN_POINT ( 'NONE',  ( -9.984503880673473830, 210.2968891136704315, 69.65113791807854682 ) ) ;
#2016 = FACE_OUTER_BOUND ( 'NONE', #11926, .T. ) ;
#2017 = CARTESIAN_POINT ( 'NONE',  ( 3.135527875058820690, 216.4958274776887492, 49.40113791807857524 ) ) ;
#2018 = APPLICATION_CONTEXT ( 'automotive_design' ) ;
#2019 = ITEM_DEFINED_TRANSFORMATION ( 'NONE', 'NONE', #33331,  #2404 ) ;
#2020 = CARTESIAN_POINT ( 'NONE',  ( -8.062137200540920645, 212.9164362838581894, 21.80113791807856671 ) ) ;
#2021 = CARTESIAN_POINT ( 'NONE',  ( 8.000000000000008882, 206.9523078486586485, 8.001137918078566003 ) ) ;
#2022 = CARTESIAN_POINT ( 'NONE',  ( 0.5735064479039687635, -3.710337782248086747, -2.761158938895358350 ) ) ;
#2023 = CARTESIAN_POINT ( 'NONE',  ( 3.499999999999993339, -2.020725942163723143, -0.3126073911696551910 ) ) ;
#2024 = CARTESIAN_POINT ( 'NONE',  ( 12.00000000000000711, 206.9523078486586485, 29.00113791807856956 ) ) ;
#2025 = LINE ( 'NONE', #7138, #23818 ) ;
#2026 = AXIS2_PLACEMENT_3D ( 'NONE', #600, #24260, #8937 ) ;
#2027 = EDGE_CURVE ( 'NONE', #20133, #13309, #33132, .T. ) ;
#2028 = CARTESIAN_POINT ( 'NONE',  ( 10.00000000000000711, 206.9523078486586201, 74.00113791807858377 ) ) ;
#2029 = CARTESIAN_POINT ( 'NONE',  ( -9.984503880673475606, 210.2968891136704315, 45.65113791807856813 ) ) ;
#2030 = VECTOR ( 'NONE', #31162, 999.9999999999998863 ) ;
#2031 = CARTESIAN_POINT ( 'NONE',  ( 0.000000000000000000, 0.000000000000000000, 0.000000000000000000 ) ) ;
#2032 = CARTESIAN_POINT ( 'NONE',  ( 85.28867513459485394, 170.7719333635740497, -7.904646289410545231E-15 ) ) ;
#2033 = CARTESIAN_POINT ( 'NONE',  ( 11.98450388067341876, 210.9467285061363953, 15.84886208192143719 ) ) ;
#2034 = CARTESIAN_POINT ( 'NONE',  ( -3.044812012439970683, 197.4746971517856196, 22.89886208192143613 ) ) ;
#2035 = CARTESIAN_POINT ( 'NONE',  ( 76.29999999453761461, 167.3344367211045096, -8.961492836873482304 ) ) ;
#2036 = ORIENTED_EDGE ( 'NONE', *, *, #29715, .T. ) ;
#2037 = CARTESIAN_POINT ( 'NONE',  ( -11.98450388067348804, 210.9467285061362247, 57.65113791807858945 ) ) ;
#2038 = CARTESIAN_POINT ( 'NONE',  ( 6.500168698208129925, 211.6636982574063381, 76.70113791807857240 ) ) ;
#2039 = CARTESIAN_POINT ( 'NONE',  ( -3.044812012439970683, 197.4746971517856196, 37.89886208192143613 ) ) ;
#2040 = EDGE_CURVE ( 'NONE', #21429, #17270, #21992, .T. ) ;
#2041 = DIRECTION ( 'NONE',  ( 1.000000000000000000, -0.000000000000000000, -0.000000000000000000 ) ) ;
#2042 = AXIS2_PLACEMENT_3D ( 'NONE', #21703, #6196, #16414 ) ;
#2043 = ORIENTED_EDGE ( 'NONE', *, *, #15447, .T. ) ;
#2044 = ORIENTED_EDGE ( 'NONE', *, *, #6265, .F. ) ;
#2045 = VERTEX_POINT ( 'NONE', #8540 ) ;
#2046 = CARTESIAN_POINT ( 'NONE',  ( 51.78867513459482552, 155.0000000000000000, 15.00000000000001243 ) ) ;
#2047 = ADVANCED_FACE ( 'NONE', ( #16205 ), #18935, .T. ) ;
#2048 = CARTESIAN_POINT ( 'NONE',  ( 4.555094537983153558, 5.243183837310242623, -6.208110906918258287 ) ) ;
#2049 = EDGE_LOOP ( 'NONE', ( #24718, #18953, #9756, #29271 ) ) ;
#2050 = CARTESIAN_POINT ( 'NONE',  ( 7.984503880673485376, 204.3529502787953902, 29.15113791807857169 ) ) ;
#2051 = CARTESIAN_POINT ( 'NONE',  ( 55.01132485994281041, 142.2402378747194405, 9.270509831248432420 ) ) ;
#2052 = CARTESIAN_POINT ( 'NONE',  ( 10.00000000000000711, 207.0476921513415220, 9.998862081921435774 ) ) ;
#2053 = CARTESIAN_POINT ( 'NONE',  ( 53.47499999726881015, 160.0630714827496206, -15.58253175000000823 ) ) ;
#2054 = ORIENTED_EDGE ( 'NONE', *, *, #8945, .T. ) ;
#2055 = CARTESIAN_POINT ( 'NONE',  ( -2.426778023690262742, 214.6231898156240163, 61.10113791807857808 ) ) ;
#2056 = CARTESIAN_POINT ( 'NONE',  ( 0.000000000000000000, 0.000000000000000000, -2.899999999999999911 ) ) ;
#2057 = VECTOR ( 'NONE', #8457, 1000.000000000000000 ) ;
#2058 = DIRECTION ( 'NONE',  ( 0.000000000000000000, 0.000000000000000000, 1.000000000000000000 ) ) ;
#2059 = CARTESIAN_POINT ( 'NONE',  ( 3.135527875058981895, 197.5041725223112792, 100.5988620819214390 ) ) ;
#2060 = CARTESIAN_POINT ( 'NONE',  ( 68.47499999726878173, 149.9369285172503510, 15.58253174999999580 ) ) ;
#2061 = CARTESIAN_POINT ( 'NONE',  ( -10.00000000000000711, 207.0476921513413515, 39.50113791807856956 ) ) ;
#2062 = DIRECTION ( 'NONE',  ( -0.08583835255247916629, -0.09953364313786493278, -0.9913247858874408847 ) ) ;
#2063 = EDGE_CURVE ( 'NONE', #1148, #11257, #24961, .T. ) ;
#2064 = CARTESIAN_POINT ( 'NONE',  ( 6.220909254589536808, 215.4770327129947702, 16.55113791807857027 ) ) ;
#2065 = APPLICATION_PROTOCOL_DEFINITION ( 'draft international standard', 'automotive_design', 1998, #27683 ) ;
#2066 = CARTESIAN_POINT ( 'NONE',  ( 86.10000000000000853, 141.2096805137202580, -4.480746418436742040 ) ) ;
#2067 = DIRECTION ( 'NONE',  ( 0.000000000000000000, 0.000000000000000000, -1.000000000000000000 ) ) ;
#2068 = CARTESIAN_POINT ( 'NONE',  ( -9.949154985843399857, 217.7087784572769067, 102.9933096652613074 ) ) ;
#2069 = DIRECTION ( 'NONE',  ( -0.000000000000000000, -0.000000000000000000, 1.000000000000000000 ) ) ;
#2070 = CARTESIAN_POINT ( 'NONE',  ( 53.07499999726880446, 141.7447067706911810, -9.630534252274385310 ) ) ;
#2071 = EDGE_CURVE ( 'NONE', #30105, #15562, #25515, .T. ) ;
#2072 = CARTESIAN_POINT ( 'NONE',  ( -8.062137200540920645, 212.9164362838581894, 45.80113791807856671 ) ) ;
#2073 = CARTESIAN_POINT ( 'NONE',  ( 82.32499999726880446, 145.8408176439707802, 12.60653300113718345 ) ) ;
#2074 = DIRECTION ( 'NONE',  ( 1.000000000000000000, -0.000000000000000000, -0.000000000000000000 ) ) ;
#2075 = CARTESIAN_POINT ( 'NONE',  ( -0.6249999999999991118, -8.299410119600880265, -7.298562697733108173 ) ) ;
#2076 = CARTESIAN_POINT ( 'NONE',  ( 54.79999999453763593, 163.5228861582408797, 11.73074641843673049 ) ) ;
#2077 = EDGE_LOOP ( 'NONE', ( #31532, #20694 ) ) ;
#2078 = CARTESIAN_POINT ( 'NONE',  ( -12.00000000000000711, 207.0476921513413515, 33.50113791807857666 ) ) ;
#2079 = AXIS2_PLACEMENT_3D ( 'NONE', #27844, #33644, #25468 ) ;
#2080 = DIRECTION ( 'NONE',  ( -0.000000000000000000, -0.000000000000000000, 1.000000000000000000 ) ) ;
#2081 = B_SPLINE_CURVE_WITH_KNOTS ( 'NONE', 3,
 ( #9283, #32286, #6561, #3835, #24964 ),
 .UNSPECIFIED., .F., .F.,
 ( 4, 1, 4 ),
 ( 0.000000000000000000, 0.003752776749732569198, 0.007505553499465138396 ),
 .UNSPECIFIED. ) ;
#2082 = CARTESIAN_POINT ( 'NONE',  ( 8.118202686958138514, 201.1607312380088501, 13.29886208192143648 ) ) ;
#2083 = CIRCLE ( 'NONE', #24369, 2.500000000000000000 ) ;
#2084 = DIRECTION ( 'NONE',  ( 1.000000000000000000, 0.000000000000000000, 0.000000000000000000 ) ) ;
#2085 = VERTEX_POINT ( 'NONE', #24212 ) ;
#2086 = CARTESIAN_POINT ( 'NONE',  ( 10.01549611932653860, 210.2015048109876716, 7.851137918078566535 ) ) ;
#2087 = CARTESIAN_POINT ( 'NONE',  ( 6.139770520408368348, 198.4640165459539674, 59.45113791807855819 ) ) ;
#2088 = ORIENTED_EDGE ( 'NONE', *, *, #12049, .F. ) ;
#2089 = CARTESIAN_POINT ( 'NONE',  ( 8.000000000000008882, 207.0476921513415220, 21.99886208192143400 ) ) ;
#2090 = CIRCLE ( 'NONE', #13506, 12.10452846326765020 ) ;
#2091 = CARTESIAN_POINT ( 'NONE',  ( 6.500000000000000000, 3.752776749732573247, -0.8000000000000003775 ) ) ;
#2092 = ORIENTED_EDGE ( 'NONE', *, *, #32224, .T. ) ;
#2093 = CARTESIAN_POINT ( 'NONE',  ( 8.000000000000008882, 206.9523078486586485, 5.001137918078565114 ) ) ;
#2094 = EDGE_CURVE ( 'NONE', #2685, #8055, #18977, .T. ) ;
#2095 = EDGE_CURVE ( 'NONE', #31583, #27125, #471, .T. ) ;
#2096 = CARTESIAN_POINT ( 'NONE',  ( -125.0000000000000000, 0.000000000000000000, -35.00000000000000000 ) ) ;
#2097 = CARTESIAN_POINT ( 'NONE',  ( -9.736236675708031640, 214.0148392665760753, 92.79886208192142760 ) ) ;
#2098 = CARTESIAN_POINT ( 'NONE',  ( 39.77499999726881441, 169.8198683612136222, -4.815267126137197984 ) ) ;
#2099 = ORIENTED_EDGE ( 'NONE', *, *, #22368, .F. ) ;
#2100 = CARTESIAN_POINT ( 'NONE',  ( 42.12499999726881583, 155.0000000000000000, 15.58253174999999402 ) ) ;
#2101 = CARTESIAN_POINT ( 'NONE',  ( 128.2263702798682630, 4.198250922590480272, 35.00001199999999102 ) ) ;
#2102 = CARTESIAN_POINT ( 'NONE',  ( 3.783380760145018981E-16, -7.895640089090872671, -6.564402953523720718 ) ) ;
#2103 = AXIS2_PLACEMENT_3D ( 'NONE', #21080, #17861, #5416 ) ;
#2104 = CARTESIAN_POINT ( 'NONE',  ( 8.118202686958138514, 201.1607312380088501, 67.29886208192144181 ) ) ;
#2105 = CARTESIAN_POINT ( 'NONE',  ( 44.87499999726880873, 138.6155565068815463, -3.929120461958505118E-15 ) ) ;
#2106 = DIRECTION ( 'NONE',  ( 1.000000000000000000, 0.000000000000000000, 0.000000000000000000 ) ) ;
#2107 = CARTESIAN_POINT ( 'NONE',  ( 10.00000000000000711, 206.9523078486586201, -0.9988620819214343305 ) ) ;
#2108 = CARTESIAN_POINT ( 'NONE',  ( 8.551039143100586770, 208.8253170565643302, -0.4549153643320096307 ) ) ;
#2109 = EDGE_CURVE ( 'NONE', #32263, #5261, #11359, .T. ) ;
#2110 = AXIS2_PLACEMENT_3D ( 'NONE', #33217, #15659, #26059 ) ;
#2111 = CARTESIAN_POINT ( 'NONE',  ( 61.79999999999999716, 142.6655632788954620, 8.961492836873471646 ) ) ;
#2112 = CARTESIAN_POINT ( 'NONE',  ( 8.118202686958039038, 212.8392687619912635, 91.70113791807857240 ) ) ;
#2113 = CARTESIAN_POINT ( 'NONE',  ( -3.214438021527938005, -2.185595227304884425, -0.2174200650117698586 ) ) ;
#2114 = CARTESIAN_POINT ( 'NONE',  ( 8.118202686958039038, 212.8392687619912635, 73.70113791807857240 ) ) ;
#2115 = CARTESIAN_POINT ( 'NONE',  ( -7.112481253775184697, 4.553861071372892866, -7.781689322728085223 ) ) ;
#2116 = CARTESIAN_POINT ( 'NONE',  ( -96.16666666666678509, -63.33333333333321491, 11.66666666666661278 ) ) ;
#2117 = EDGE_CURVE ( 'NONE', #11134, #6637, #15716, .T. ) ;
#2118 = CARTESIAN_POINT ( 'NONE',  ( 3.662846001189864698, 218.4274158808046593, 84.39886208192143613 ) ) ;
#2119 = VECTOR ( 'NONE', #32, 1000.000000000000000 ) ;
#2120 = CARTESIAN_POINT ( 'NONE',  ( 61.32499999726881157, 164.1591823560292198, -12.60653300113719766 ) ) ;
#2122 = ORIENTED_EDGE ( 'NONE', *, *, #9157, .F. ) ;
#2121 = CARTESIAN_POINT ( 'NONE',  ( 3.135527875058820690, 216.4958274776887492, 34.40113791807856813 ) ) ;
#2123 = CARTESIAN_POINT ( 'NONE',  ( -59.75427847806285797, 194.9412682558892982, -2.168710897896606760 ) ) ;
#2124 = CARTESIAN_POINT ( 'NONE',  ( 34.99999999453763166, 155.0000000000000000, 14.49999999999999467 ) ) ;
#2125 = CARTESIAN_POINT ( 'NONE',  ( 3.753561863808689836, 218.3979405102790565, 97.40113791807858945 ) ) ;
#2126 = DIRECTION ( 'NONE',  ( -1.000000000000000000, 0.000000000000000000, 0.000000000000000000 ) ) ;
#2127 = ORIENTED_EDGE ( 'NONE', *, *, #19919, .T. ) ;
#2128 = CARTESIAN_POINT ( 'NONE',  ( 3.044812012439969795, 216.5253028482143520, 90.39886208192143613 ) ) ;
#2129 = CARTESIAN_POINT ( 'NONE',  ( 9.680171189290716072, 214.0920067884432854, 27.69886208192143684 ) ) ;
#2130 = CARTESIAN_POINT ( 'NONE',  ( -6.818286579240217193, 1.325012739682870810, -6.208253321455267759 ) ) ;
#2131 = VECTOR ( 'NONE', #9268, 1000.000000000000000 ) ;
#2132 = CARTESIAN_POINT ( 'NONE',  ( 3.135527875058820690, 216.4958274776887492, 37.40113791807857524 ) ) ;
#2133 = CARTESIAN_POINT ( 'NONE',  ( 66.28867513459483973, 139.2280666364260071, -4.041636747397287284E-15 ) ) ;
#2134 = CARTESIAN_POINT ( 'NONE',  ( 10.01549611932659545, 203.7984951890123853, 94.14886208192143613 ) ) ;
#2135 = FACE_OUTER_BOUND ( 'NONE', #29476, .T. ) ;
#2136 = EDGE_LOOP ( 'NONE', ( #33216, #22533, #24327, #939 ) ) ;
#2137 = CARTESIAN_POINT ( 'NONE',  ( 70.11132485994281183, 169.2658477444273331, -4.635254915624224203 ) ) ;
#2138 = CARTESIAN_POINT ( 'NONE',  ( -2.426778023690076225, 199.3768101843759553, 79.89886208192143613 ) ) ;
#2139 = ORIENTED_EDGE ( 'NONE', *, *, #26065, .T. ) ;
#2140 = DIRECTION ( 'NONE',  ( 0.000000000000000000, 0.000000000000000000, -1.000000000000000000 ) ) ;
#2141 = ORIENTED_EDGE ( 'NONE', *, *, #2063, .T. ) ;
#2142 = CARTESIAN_POINT ( 'NONE',  ( -125.0000000000000000, 0.000000000000000000, 20.00000000000000000 ) ) ;
#2143 = B_SPLINE_CURVE_WITH_KNOTS ( 'NONE', 3,
 ( #16956, #32297, #27351, #14236, #12193, #4017, #22073, #14739, #14411, #27520, #17134, #12018, #30080, #27852, #9629, #20026 ),
 .UNSPECIFIED., .F., .F.,
 ( 4, 2, 2, 2, 2, 2, 2, 4 ),
 ( 0.01344638572600751272, 0.01751370969988639420, 0.01954737168682584708, 0.02158103367376530690, 0.02361469566070476672, 0.02564835764764422307, 0.02768201963458367942, 0.02971568162152313924 ),
 .UNSPECIFIED. ) ;
#2144 = CARTESIAN_POINT ( 'NONE',  ( 79.92499999726881299, 164.1591823560292198, 12.60653300113718167 ) ) ;
#2145 = DIRECTION ( 'NONE',  ( -1.000000000000000000, 0.000000000000000000, 0.000000000000000000 ) ) ;
#2146 = CARTESIAN_POINT ( 'NONE',  ( -7.984503880673488041, 209.6470497212046098, 78.65113791807858945 ) ) ;
#2147 = CARTESIAN_POINT ( 'NONE',  ( 112.4999999999999858, 155.0000000000000000, -6.938893903907228378E-15 ) ) ;
#2148 = PRESENTATION_STYLE_ASSIGNMENT (( #2312 ) ) ;
#2149 = CARTESIAN_POINT ( 'NONE',  ( 41.39999999999999147, 159.7113355953771077, 14.49999999999999289 ) ) ;
#2150 = CARTESIAN_POINT ( 'NONE',  ( -6.444103211790928043, 202.2591342207265939, 53.19886208192144039 ) ) ;
#2151 = AXIS2_PLACEMENT_3D ( 'NONE', #32067, #18460, #11129 ) ;
#2152 = DIRECTION ( 'NONE',  ( 0.000000000000000000, 0.000000000000000000, 1.000000000000000000 ) ) ;
#2153 = CARTESIAN_POINT ( 'NONE',  ( -6.500000000000000888, 4.076783350660894811, -6.121918786669029444 ) ) ;
#2154 = CARTESIAN_POINT ( 'NONE',  ( -130.1133565525086908, 1.374176392886221842, 35.00001199999999812 ) ) ;
#2155 = CARTESIAN_POINT ( 'NONE',  ( 58.22499999726881015, 149.9369285172503510, 15.58253174999999580 ) ) ;
#2156 = CARTESIAN_POINT ( 'NONE',  ( 67.87499999726881583, 171.3844434931184253, -7.942151717890132712E-15 ) ) ;
#2157 = CARTESIAN_POINT ( 'NONE',  ( 0.05014649552807549926, 219.6175466908591716, 64.25113791807856956 ) ) ;
#2158 = DIRECTION ( 'NONE',  ( 1.000000000000000000, 0.000000000000000000, 0.000000000000000000 ) ) ;
#2159 = CARTESIAN_POINT ( 'NONE',  ( 3.753561863808689836, 218.3979405102790565, 7.401137918078566358 ) ) ;
#2160 = CARTESIAN_POINT ( 'NONE',  ( 9.984503880673473830, 203.7031108863295401, 77.15113791807857524 ) ) ;
#2161 = CARTESIAN_POINT ( 'NONE',  ( -3.753561863808878130, 218.3979405102790281, 39.09886208192143187 ) ) ;
#2162 = CARTESIAN_POINT ( 'NONE',  ( 8.062137200540822946, 212.9164362838583315, 60.69886208192143329 ) ) ;
#2163 = DIRECTION ( 'NONE',  ( 1.000000000000000000, 0.000000000000000000, 0.000000000000000000 ) ) ;
#2164 = CARTESIAN_POINT ( 'NONE',  ( -0.05014649552807705357, 194.3824533091408000, 83.75113791807856956 ) ) ;
#2165 = CARTESIAN_POINT ( 'NONE',  ( 74.18867513459481700, 140.7341522555726669, 4.635254915624211769 ) ) ;
#2166 = CARTESIAN_POINT ( 'NONE',  ( 3.044812012440130555, 197.4746971517856764, 8.601137918078565647 ) ) ;
#2167 = CARTESIAN_POINT ( 'NONE',  ( 3.044812012439969795, 216.5253028482143520, 66.39886208192143613 ) ) ;
#2168 = CARTESIAN_POINT ( 'NONE',  ( 92.60208470531341618, 155.0000000000000000, -12.10452846326763598 ) ) ;
#2169 = ORIENTED_EDGE ( 'NONE', *, *, #27707, .F. ) ;
#2170 = CARTESIAN_POINT ( 'NONE',  ( -11.98450388067341876, 203.0532714938636047, 71.34886208192142476 ) ) ;
#2171 = ORIENTED_EDGE ( 'NONE', *, *, #10125, .T. ) ;
#2172 = CARTESIAN_POINT ( 'NONE',  ( 79.97499999726881015, 169.8198683612136222, 4.815267126137181997 ) ) ;
#2173 = CARTESIAN_POINT ( 'NONE',  ( -6.444103211790928043, 202.2591342207265939, 50.19886208192144750 ) ) ;
#2174 = AXIS2_PLACEMENT_3D ( 'NONE', #9350, #3898, #19407 ) ;
#2175 = ORIENTED_EDGE ( 'NONE', *, *, #25017, .T. ) ;
#2176 = CARTESIAN_POINT ( 'NONE',  ( 70.62499999726881583, 138.6155565068815747, -3.929120461958505118E-15 ) ) ;
#2177 = CARTESIAN_POINT ( 'NONE',  ( -125.0000000000000000, 0.000000000000000000, 20.00000000000000000 ) ) ;
#2178 = CARTESIAN_POINT ( 'NONE',  ( -56.12844631811822893, 194.9921284422999292, -0.8077925457893648797 ) ) ;
#2179 = CARTESIAN_POINT ( 'NONE',  ( 65.72499999726881015, 169.8198683612136222, 4.815267126137181997 ) ) ;
#2180 = LINE ( 'NONE', #2696, #10740 ) ;
#2181 = CARTESIAN_POINT ( 'NONE',  ( 8.118202686958138514, 201.1607312380088501, 46.29886208192143471 ) ) ;
#2182 = VERTEX_POINT ( 'NONE', #22836 ) ;
#2183 = CYLINDRICAL_SURFACE ( 'NONE', #10236, 2.149999999999996803 ) ;
#2184 = DIRECTION ( 'NONE',  ( 1.000000000000000000, 0.000000000000000000, 0.000000000000000000 ) ) ;
#2185 = SHAPE_REPRESENTATION ( 'Internal Hydraulic Release Piston', ( #2404 ), #27952 ) ;
#2186 = CARTESIAN_POINT ( 'NONE',  ( 92.60208470531341618, 155.0000000000000000, 0.000000000000000000 ) ) ;
#2187 = CARTESIAN_POINT ( 'NONE',  ( -0.05014649552828365914, 215.4116977939061144, 27.24886208192143755 ) ) ;
#2188 = CARTESIAN_POINT ( 'NONE',  ( 3.044812012440130555, 197.4746971517856764, 68.60113791807857808 ) ) ;
#2189 = DIRECTION ( 'NONE',  ( -1.000000000000000000, 0.000000000000000000, 0.000000000000000000 ) ) ;
#2190 = ADVANCED_FACE ( 'NONE', ( #32712 ), #20065, .F. ) ;
#2191 = CARTESIAN_POINT ( 'NONE',  ( -9.984503880673473830, 210.2968891136704315, 54.65113791807858235 ) ) ;
#2192 = CONTEXT_DEPENDENT_SHAPE_REPRESENTATION ( #32699, #19341 ) ;
#2193 = CARTESIAN_POINT ( 'NONE',  ( 8.118202686958039038, 212.8392687619912635, 19.70113791807856884 ) ) ;
#2194 = CARTESIAN_POINT ( 'NONE',  ( 0.05014649552807626948, 215.4116977939061144, 7.251137918078565114 ) ) ;
#2195 = DIRECTION ( 'NONE',  ( 1.000000000000000000, 1.804112415015879625E-16, 0.000000000000000000 ) ) ;
#2196 = CARTESIAN_POINT ( 'NONE',  ( 37.42499999726881299, 168.2552932293087906, -9.630534252274387086 ) ) ;
#2197 = CARTESIAN_POINT ( 'NONE',  ( 3.662846001190051659, 195.5725841191953691, 32.60113791807857098 ) ) ;
#2198 = FACE_BOUND ( 'NONE', #2251, .T. ) ;
#2199 = CARTESIAN_POINT ( 'NONE',  ( -6.139770520408369237, 215.5359834540460042, 75.95113791807857240 ) ) ;
#2200 = CARTESIAN_POINT ( 'NONE',  ( 9.984503880673473830, 203.7031108863295401, 47.15113791807857524 ) ) ;
#2201 = DIRECTION ( 'NONE',  ( 0.8660254037844359321, 0.5000000000000046629, 0.000000000000000000 ) ) ;
#2202 = CARTESIAN_POINT ( 'NONE',  ( 7.456977232089471386, 196.8216656703012006, 10.44886208192143506 ) ) ;
#2203 = CARTESIAN_POINT ( 'NONE',  ( 8.062137200540822946, 212.9164362838583315, 24.69886208192143684 ) ) ;
#2204 = CARTESIAN_POINT ( 'NONE',  ( 73.09999999453764019, 150.2886644046228639, 14.49999999999999645 ) ) ;
#2205 = ORIENTED_EDGE ( 'NONE', *, *, #7919, .F. ) ;
#2206 = CARTESIAN_POINT ( 'NONE',  ( 3.662846001190051659, 195.5725841191953691, 53.60113791807856387 ) ) ;
#2207 = CARTESIAN_POINT ( 'NONE',  ( 7.984503880673485376, 204.3529502787953902, 80.15113791807857524 ) ) ;
#2208 = CARTESIAN_POINT ( 'NONE',  ( 8.118202686958138514, 201.1607312380088501, 40.29886208192143471 ) ) ;
#2209 = DIRECTION ( 'NONE',  ( 1.000000000000000000, -0.000000000000000000, -0.000000000000000000 ) ) ;
#2210 = VERTEX_POINT ( 'NONE', #25054 ) ;
#2211 = CARTESIAN_POINT ( 'NONE',  ( -3.662846001189865142, 195.5725841191952838, 43.89886208192143613 ) ) ;
#2212 = EDGE_LOOP ( 'NONE', ( #10140, #20740 ) ) ;
#2213 = EDGE_LOOP ( 'NONE', ( #7834, #204, #21981, #13188, #17457, #11834 ) ) ;
#2214 = CARTESIAN_POINT ( 'NONE',  ( -63.49999999999884892, 215.0000000000003979, 0.000000000000000000 ) ) ;
#2215 = DIRECTION ( 'NONE',  ( 0.000000000000000000, 0.000000000000000000, 1.000000000000000000 ) ) ;
#2216 = ORIENTED_EDGE ( 'NONE', *, *, #22715, .T. ) ;
#2217 = CARTESIAN_POINT ( 'NONE',  ( -6.500168698208129925, 202.3363017425936050, 36.20113791807857240 ) ) ;
#2218 = CARTESIAN_POINT ( 'NONE',  ( 81.71132485994280614, 155.0000000000000000, -15.00000000000002487 ) ) ;
#2219 = CARTESIAN_POINT ( 'NONE',  ( 10.01549611932659545, 203.7984951890123853, 13.14886208192143258 ) ) ;
#2220 = CARTESIAN_POINT ( 'NONE',  ( 56.27499999726880731, 160.0630714827496206, 15.58253174999999224 ) ) ;
#2221 = VERTEX_POINT ( 'NONE', #12106 ) ;
#2222 = CARTESIAN_POINT ( 'NONE',  ( 2.517493886308900919, 214.5937144450984420, 55.40113791807858235 ) ) ;
#2223 = DIRECTION ( 'NONE',  ( -1.000000000000000000, -0.000000000000000000, -0.000000000000000000 ) ) ;
#2224 = SURFACE_STYLE_FILL_AREA ( #17551 ) ;
#2225 = DIRECTION ( 'NONE',  ( 0.000000000000000000, 0.000000000000000000, 1.000000000000000000 ) ) ;
#2226 = CARTESIAN_POINT ( 'NONE',  ( 10.00000000000000711, 207.0476921513415220, 96.99886208192143044 ) ) ;
#2227 = CARTESIAN_POINT ( 'NONE',  ( 66.67499999726881299, 141.7447067706911810, 9.630534252274376428 ) ) ;
#2228 = CARTESIAN_POINT ( 'NONE',  ( 8.062137200540920645, 201.0835637161417822, 38.30113791807857382 ) ) ;
#2229 = DIRECTION ( 'NONE',  ( 0.000000000000000000, 0.9949972439410067482, -0.09990237509589337817 ) ) ;
#2230 = EDGE_CURVE ( 'NONE', #2182, #32112, #19509, .T. ) ;
#2231 = CARTESIAN_POINT ( 'NONE',  ( -10.00000000000000711, 207.0476921513413515, 21.50113791807856956 ) ) ;
#2232 = CARTESIAN_POINT ( 'NONE',  ( -10.00000000000000711, 206.9523078486584495, 101.4988620819214304 ) ) ;
#2233 = CARTESIAN_POINT ( 'NONE',  ( 34.02499999726880731, 160.0630714827496206, 15.58253174999999402 ) ) ;
#2234 = DIRECTION ( 'NONE',  ( 0.000000000000000000, 0.000000000000000000, -1.000000000000000000 ) ) ;
#2235 = FACE_OUTER_BOUND ( 'NONE', #16029, .T. ) ;
#2236 = CARTESIAN_POINT ( 'NONE',  ( 8.118202686958039038, 212.8392687619912635, 100.7011379180785866 ) ) ;
#2237 = EDGE_CURVE ( 'NONE', #28404, #29398, #25221, .T. ) ;
#2238 = CARTESIAN_POINT ( 'NONE',  ( 97.20416941062678973, 155.0000000000000000, 0.000000000000000000 ) ) ;
#2239 = CARTESIAN_POINT ( 'NONE',  ( 53.27499999726880731, 149.9369285172503510, -15.58253175000000823 ) ) ;
#2240 = CARTESIAN_POINT ( 'NONE',  ( 0.05014649552810505201, 217.5146222423826714, 49.25113791807857666 ) ) ;
#2241 = DIRECTION ( 'NONE',  ( 1.000000000000000000, 0.000000000000000000, 0.000000000000000000 ) ) ;
#2242 = EDGE_CURVE ( 'NONE', #25792, #19681, #24675, .T. ) ;
#2243 = CARTESIAN_POINT ( 'NONE',  ( -2.428571428571428381, 2.974142226500714333E-16, 2.066666666667000385 ) ) ;
#2244 = DIRECTION ( 'NONE',  ( 0.000000000000000000, 0.000000000000000000, 1.000000000000000000 ) ) ;
#2245 = CARTESIAN_POINT ( 'NONE',  ( 52.09999999453762598, 159.7113355953771077, -14.50000000000000888 ) ) ;
#2246 = ORIENTED_EDGE ( 'NONE', *, *, #23328, .F. ) ;
#2247 = CARTESIAN_POINT ( 'NONE',  ( 7.456977232089302632, 217.1783343296989131, 25.55113791807857027 ) ) ;
#2248 = DIRECTION ( 'NONE',  ( 0.000000000000000000, 0.000000000000000000, -1.000000000000000000 ) ) ;
#2249 = CARTESIAN_POINT ( 'NONE',  ( -10.01549611932659722, 210.2015048109875011, 8.648862081921436129 ) ) ;
#2250 = DIRECTION ( 'NONE',  ( 0.000000000000000000, 0.000000000000000000, -1.000000000000000000 ) ) ;
#2251 = EDGE_LOOP ( 'NONE', ( #26956, #17710 ) ) ;
#2252 = CARTESIAN_POINT ( 'NONE',  ( 0.05014649552810505201, 217.5146222423826714, 10.25113791807856778 ) ) ;
#2253 = CARTESIAN_POINT ( 'NONE',  ( -10.00000000000000711, 207.0476921513413515, 75.50113791807858377 ) ) ;
#2254 = ADVANCED_FACE ( 'NONE', ( #33402 ), #4825, .T. ) ;
#2255 = ORIENTED_EDGE ( 'NONE', *, *, #17675, .F. ) ;
#2256 = CARTESIAN_POINT ( 'NONE',  ( 8.000000000000008882, 207.0476921513415220, 24.99886208192143400 ) ) ;
#2257 = LINE ( 'NONE', #30198, #15419 ) ;
#2258 = CONICAL_SURFACE ( 'NONE', #6597, 3.499999999999999556, 1.047197551196589638 ) ;
#2259 = ORIENTED_EDGE ( 'NONE', *, *, #16821, .F. ) ;
#2260 = CARTESIAN_POINT ( 'NONE',  ( -4.984841277089726574, 200.2242689037092305, 3.051137918078566269 ) ) ;
#2261 = EDGE_CURVE ( 'NONE', #27176, #32104, #10074, .T. ) ;
#2262 = CARTESIAN_POINT ( 'NONE',  ( -12.00000000000000711, 206.9523078486584780, 86.49886208192144466 ) ) ;
#2263 = CARTESIAN_POINT ( 'NONE',  ( 38.17499999726881299, 164.1591823560292198, 12.60653300113718167 ) ) ;
#2264 = VERTEX_POINT ( 'NONE', #4435 ) ;
#2265 = CARTESIAN_POINT ( 'NONE',  ( 44.12499999726881583, 155.0000000000000000, 15.58253174999999402 ) ) ;
#2266 = CARTESIAN_POINT ( 'NONE',  ( -65.20000000000000284, -7.347880794884118356E-15, 19.29999999999998295 ) ) ;
#2267 = CARTESIAN_POINT ( 'NONE',  ( 10.00000000000000711, 206.9523078486586201, 8.001137918078566003 ) ) ;
#2268 = CARTESIAN_POINT ( 'NONE',  ( 9.984503880673420539, 210.2968891136705167, 69.84886208192143897 ) ) ;
#2269 = CARTESIAN_POINT ( 'NONE',  ( 47.47499999726881015, 160.0630714827496206, -15.58253175000000823 ) ) ;
#2270 = CARTESIAN_POINT ( 'NONE',  ( -67.50000599999999906, 155.0000000000000000, 17.00000000000001421 ) ) ;
#2271 = CARTESIAN_POINT ( 'NONE',  ( 3.044812012440130555, 197.4746971517856764, 17.60113791807856742 ) ) ;
#2272 = CARTESIAN_POINT ( 'NONE',  ( -16.66875746037183248, -22.13055319862718662, -0.1142222407377356808 ) ) ;
#2273 = CARTESIAN_POINT ( 'NONE',  ( 68.00000000000001421, 139.7537977485451393, -4.138211985947621020E-15 ) ) ;
#2274 = CARTESIAN_POINT ( 'NONE',  ( 8.118202686958039038, 212.8392687619912635, 94.70113791807857240 ) ) ;
#2275 = FACE_OUTER_BOUND ( 'NONE', #6180, .T. ) ;
#2276 = CARTESIAN_POINT ( 'NONE',  ( 0.05014649552810505201, 217.5146222423826714, 76.25113791807855534 ) ) ;
#2277 = CARTESIAN_POINT ( 'NONE',  ( -4.419133455862249704, 6.108866147517435508, -7.026396753507433424 ) ) ;
#2278 = CARTESIAN_POINT ( 'NONE',  ( 33.37499999726880873, 155.0000000000000000, -15.58253175000000823 ) ) ;
#2279 = CARTESIAN_POINT ( 'NONE',  ( -11.98450388067341876, 203.0532714938636047, 83.34886208192143897 ) ) ;
#2280 = CARTESIAN_POINT ( 'NONE',  ( 72.52499999726882152, 140.1801316387863778, 4.815267126137185549 ) ) ;
#2282 = ORIENTED_EDGE ( 'NONE', *, *, #24533, .F. ) ;
#2281 = CARTESIAN_POINT ( 'NONE',  ( 10.01549611932653860, 210.2015048109876716, 28.85113791807856387 ) ) ;
#2283 = DIRECTION ( 'NONE',  ( 0.000000000000000000, -0.7071067811865540120, -0.7071067811865411334 ) ) ;
#2284 = AXIS2_PLACEMENT_3D ( 'NONE', #19617, #14669, #2067 ) ;
#2285 = CARTESIAN_POINT ( 'NONE',  ( 35.29999999453763593, 142.6655632788954620, 8.961492836873471646 ) ) ;
#2286 = CARTESIAN_POINT ( 'NONE',  ( -3.753561863808691168, 195.6020594897209435, 98.90113791807858945 ) ) ;
#2287 = EDGE_CURVE ( 'NONE', #30017, #18599, #30683, .T. ) ;
#2288 = LINE ( 'NONE', #12842, #12668 ) ;
#2289 = ORIENTED_EDGE ( 'NONE', *, *, #7532, .F. ) ;
#2290 = CARTESIAN_POINT ( 'NONE',  ( 3.135527875058981895, 197.5041725223112792, 85.59886208192143897 ) ) ;
#2291 = AXIS2_PLACEMENT_3D ( 'NONE', #19859, #12199, #22586 ) ;
#2292 = CARTESIAN_POINT ( 'NONE',  ( 11.98450388067341876, 210.9467285061363953, 21.84886208192143542 ) ) ;
#2293 = LINE ( 'NONE', #7916, #8862 ) ;
#2294 = CARTESIAN_POINT ( 'NONE',  ( -10.00000000000000711, 207.0476921513413515, 30.50113791807856600 ) ) ;
#2295 = ORIENTED_EDGE ( 'NONE', *, *, #23532, .T. ) ;
#2296 = ADVANCED_FACE ( 'NONE', ( #32885 ), #29338, .T. ) ;
#2297 = CARTESIAN_POINT ( 'NONE',  ( -10.00000000000000711, 206.9523078486584495, 95.49886208192144466 ) ) ;
#2298 = DIRECTION ( 'NONE',  ( 0.000000000000000000, 0.000000000000000000, -1.000000000000000000 ) ) ;
#2299 = VERTEX_POINT ( 'NONE', #7168 ) ;
#2300 = CARTESIAN_POINT ( 'NONE',  ( 69.91132485994280898, 163.8167787843871110, -12.13525491562423397 ) ) ;
#2301 = CARTESIAN_POINT ( 'NONE',  ( -2.426778023690076225, 199.3768101843759553, 82.89886208192143613 ) ) ;
#2302 = EDGE_CURVE ( 'NONE', #4633, #31418, #30982, .T. ) ;
#2303 = ORIENTED_EDGE ( 'NONE', *, *, #1655, .T. ) ;
#2304 = FACE_OUTER_BOUND ( 'NONE', #1531, .T. ) ;
#2305 = ORIENTED_EDGE ( 'NONE', *, *, #7539, .F. ) ;
#2306 = CARTESIAN_POINT ( 'NONE',  ( 81.41132485994280898, 142.2402378747194405, -9.270509831248439525 ) ) ;
#2307 = CARTESIAN_POINT ( 'NONE',  ( -6.444103211791042618, 211.7408657792732356, 60.80113791807858092 ) ) ;
#2308 = CARTESIAN_POINT ( 'NONE',  ( 81.52499999726880731, 169.8198683612136222, -4.815267126137197984 ) ) ;
#2309 = PLANE ( 'NONE',  #25202 ) ;
#2310 = CARTESIAN_POINT ( 'NONE',  ( 0.05014649552807626948, 215.4116977939061144, 88.25113791807856956 ) ) ;
#2311 = DIRECTION ( 'NONE',  ( -1.000000000000000000, -0.000000000000000000, -0.000000000000000000 ) ) ;
#2313 = VECTOR ( 'NONE', #14414, 1000.000000000000114 ) ;
#2312 = SURFACE_STYLE_USAGE ( .BOTH. , #33150 ) ;
#2314 = CARTESIAN_POINT ( 'NONE',  ( 48.79999999999999716, 167.3344367211045096, -8.961492836873482304 ) ) ;
#2315 = CARTESIAN_POINT ( 'NONE',  ( 7.984503880673422316, 209.6470497212048372, 63.84886208192143187 ) ) ;
#2316 = CARTESIAN_POINT ( 'NONE',  ( 38.71132485994280614, 155.0000000000000000, 15.00000000000001243 ) ) ;
#2317 = CARTESIAN_POINT ( 'NONE',  ( 9.984503880673473830, 203.7031108863295401, 2.151137918078566358 ) ) ;
#2318 = DIRECTION ( 'NONE',  ( 0.000000000000000000, 0.000000000000000000, 1.000000000000000000 ) ) ;
#2319 = CARTESIAN_POINT ( 'NONE',  ( -124.3127766070272457, 5.250000000000003553, 35.00001199999999812 ) ) ;
#2320 = CARTESIAN_POINT ( 'NONE',  ( 58.02499999726880731, 160.0630714827496206, 15.58253174999999224 ) ) ;
#2321 = CARTESIAN_POINT ( 'NONE',  ( 69.87499999726880162, 171.3844434931184253, -7.942151717890132712E-15 ) ) ;
#2322 = CARTESIAN_POINT ( 'NONE',  ( -7.456977232089304408, 196.8216656703010301, 63.05113791807858092 ) ) ;
#2323 = FACE_BOUND ( 'NONE', #12251, .T. ) ;
#2324 = CARTESIAN_POINT ( 'NONE',  ( 12.01549611932652972, 210.8513442034534933, 10.85113791807856565 ) ) ;
#2325 = EDGE_CURVE ( 'NONE', #33225, #30802, #15185, .T. ) ;
#2326 = CARTESIAN_POINT ( 'NONE',  ( 6.139770520408367460, 198.4640165459539389, 92.45113791807857240 ) ) ;
#2327 = CARTESIAN_POINT ( 'NONE',  ( 3.662846001189864698, 218.4274158808046593, 48.39886208192143613 ) ) ;
#2328 = PRODUCT_DEFINITION_FORMATION_WITH_SPECIFIED_SOURCE ( 'ANY', '', #23052, .NOT_KNOWN. ) ;
#2329 = CARTESIAN_POINT ( 'NONE',  ( -6.220909254589682469, 215.4770327129947134, 56.94886208192143329 ) ) ;
#2330 = LINE ( 'NONE', #20551, #4129 ) ;
#2331 = CARTESIAN_POINT ( 'NONE',  ( -3.753561863808691168, 195.6020594897209435, 98.90113791807858945 ) ) ;
#2332 = CARTESIAN_POINT ( 'NONE',  ( -67.50001199999999812, 160.4776661921571588, 16.13174377802662462 ) ) ;
#2333 = CARTESIAN_POINT ( 'NONE',  ( -3.044812012440131443, 216.5253028482142952, 4.101137918078565647 ) ) ;
#2334 = EDGE_CURVE ( 'NONE', #23864, #8655, #27770, .T. ) ;
#2335 = CARTESIAN_POINT ( 'NONE',  ( 0.05014649552828275708, 196.4853777576173002, 70.74886208192143044 ) ) ;
#2336 = CARTESIAN_POINT ( 'NONE',  ( 115.4999999999999858, 207.9999999999998010, -91.79869280115066488 ) ) ;
#2337 = ORIENTED_EDGE ( 'NONE', *, *, #6806, .F. ) ;
#2338 = CARTESIAN_POINT ( 'NONE',  ( 9.680171189290716072, 214.0920067884432854, 81.69886208192144750 ) ) ;
#2339 = CARTESIAN_POINT ( 'NONE',  ( 3.044812012440130555, 197.4746971517856764, 92.60113791807857808 ) ) ;
#2340 = CIRCLE ( 'NONE', #6134, 98.00000000000000000 ) ;
#2341 = ORIENTED_EDGE ( 'NONE', *, *, #32267, .F. ) ;
#2342 = CARTESIAN_POINT ( 'NONE',  ( 78.27499999726880731, 160.0630714827496206, 15.58253174999999402 ) ) ;
#2343 = CARTESIAN_POINT ( 'NONE',  ( 4.903702542908435547, 213.8346818373419751, 54.54886208192144181 ) ) ;
#2344 = ORIENTED_EDGE ( 'NONE', *, *, #21993, .T. ) ;
#2345 = CARTESIAN_POINT ( 'NONE',  ( 71.72499999726881015, 169.8198683612136222, 4.815267126137181997 ) ) ;
#2346 = CARTESIAN_POINT ( 'NONE',  ( 6.818262094730843437, 1.323628772216571381, -6.207787212118422104 ) ) ;
#2347 = CARTESIAN_POINT ( 'NONE',  ( -56.84624105109630676, 194.9558714263463912, 1.881936590917415941 ) ) ;
#2348 = CARTESIAN_POINT ( 'NONE',  ( 66.52499999726880731, 140.1801316387863778, 4.815267126137185549 ) ) ;
#2349 = DIRECTION ( 'NONE',  ( -0.000000000000000000, -0.000000000000000000, -1.000000000000000000 ) ) ;
#2350 = CARTESIAN_POINT ( 'NONE',  ( -0.05014649552828403384, 217.5146222423826714, 48.24886208192142334 ) ) ;
#2351 = EDGE_LOOP ( 'NONE', ( #6560, #11998 ) ) ;
#2352 = DIRECTION ( 'NONE',  ( 0.000000000000000000, 0.000000000000000000, 1.000000000000000000 ) ) ;
#2353 = VECTOR ( 'NONE', #21963, 1000.000000000000000 ) ;
#2354 = DIRECTION ( 'NONE',  ( -1.000000000000000000, 0.000000000000000000, -0.000000000000000000 ) ) ;
#2355 = CARTESIAN_POINT ( 'NONE',  ( -6.500168698208244500, 211.6636982574061676, 38.79886208192143471 ) ) ;
#2356 = CARTESIAN_POINT ( 'NONE',  ( -8.062137200540920645, 212.9164362838581894, 69.80113791807856671 ) ) ;
#2357 = DIRECTION ( 'NONE',  ( 1.000000000000000000, -0.000000000000000000, -0.000000000000000000 ) ) ;
#2358 = CARTESIAN_POINT ( 'NONE',  ( 6.139770520408368348, 198.4640165459539674, 53.45113791807855108 ) ) ;
#2359 = ITEM_DEFINED_TRANSFORMATION ( 'NONE', 'NONE', #22993,  #2404 ) ;
#2360 = CARTESIAN_POINT ( 'NONE',  ( 3.135527875058820690, 216.4958274776887492, 31.40113791807857524 ) ) ;
#2361 = CARTESIAN_POINT ( 'NONE',  ( -2.426778023690262742, 214.6231898156240163, 1.101137918078566091 ) ) ;
#2362 = CARTESIAN_POINT ( 'NONE',  ( 46.78867513459482552, 155.0000000000000000, -15.00000000000002487 ) ) ;
#2363 = CIRCLE ( 'NONE', #24112, 2.149999999999985256 ) ;
#2364 = CARTESIAN_POINT ( 'NONE',  ( 0.2855619784720492826, -3.876582599186272127, -0.2174200650117948386 ) ) ;
#2365 = CARTESIAN_POINT ( 'NONE',  ( 41.02499999726880731, 149.9369285172503510, -15.58253175000000823 ) ) ;
#2366 = CARTESIAN_POINT ( 'NONE',  ( -7.375838497908182134, 217.2372850707499765, 36.95113791807856529 ) ) ;
#2367 = CYLINDRICAL_SURFACE ( 'NONE', #23840, 5.250000000000004441 ) ;
#2368 = AXIS2_PLACEMENT_3D ( 'NONE', #10280, #31377, #20658 ) ;
#2369 = CARTESIAN_POINT ( 'NONE',  ( 3.044812012440130555, 197.4746971517856764, 86.60113791807857808 ) ) ;
#2370 = CARTESIAN_POINT ( 'NONE',  ( -3.044812012440131443, 216.5253028482142952, 61.10113791807857098 ) ) ;
#2371 = CONICAL_SURFACE ( 'NONE', #22466, 27.50000000000000355, 1.047197551196595411 ) ;
#2372 = CARTESIAN_POINT ( 'NONE',  ( 0.000000000000000000, 0.000000000000000000, 2.066666666667000385 ) ) ;
#2373 = CARTESIAN_POINT ( 'NONE',  ( -9.680171189290716072, 199.9079932115567146, 17.19886208192143684 ) ) ;
#2374 = CARTESIAN_POINT ( 'NONE',  ( 6.220909254589680693, 198.5229672870052582, 25.44886208192143684 ) ) ;
#2375 = CARTESIAN_POINT ( 'NONE',  ( 75.09999999453762598, 150.2886644046228639, 14.49999999999999645 ) ) ;
#2376 = EDGE_LOOP ( 'NONE', ( #24903, #22825, #26963 ) ) ;
#2377 = CARTESIAN_POINT ( 'NONE',  ( -0.05014649552807705357, 194.3824533091408000, 71.75113791807856956 ) ) ;
#2378 = CARTESIAN_POINT ( 'NONE',  ( 0.05014649552807626948, 215.4116977939061144, 76.25113791807856956 ) ) ;
#2379 = CARTESIAN_POINT ( 'NONE',  ( -9.984503880673420539, 203.7031108863293980, 38.34886208192143897 ) ) ;
#2380 = DIRECTION ( 'NONE',  ( -0.000000000000000000, -0.000000000000000000, -1.000000000000000000 ) ) ;
#2381 = VERTEX_POINT ( 'NONE', #14997 ) ;
#2382 = CARTESIAN_POINT ( 'NONE',  ( -7.456977232089471386, 217.1783343296987709, 38.94886208192143329 ) ) ;
#2383 = AXIS2_PLACEMENT_3D ( 'NONE', #5252, #30654, #20597 ) ;
#2384 = ORIENTED_EDGE ( 'NONE', *, *, #27422, .T. ) ;
#2385 = ORIENTED_EDGE ( 'NONE', *, *, #25125, .T. ) ;
#2386 = CARTESIAN_POINT ( 'NONE',  ( 32.50000000000000000, 155.0000000000000000, -6.938893903907228378E-15 ) ) ;
#2387 = CARTESIAN_POINT ( 'NONE',  ( -6.815830331203685866, -1.210827632163352847E-13, -6.171384342982610960 ) ) ;
#2388 = ORIENTED_EDGE ( 'NONE', *, *, #18646, .F. ) ;
#2389 = PRESENTATION_LAYER_ASSIGNMENT (  '', '', ( #30672 ) ) ;
#2390 = CARTESIAN_POINT ( 'NONE',  ( 4.984841277089725686, 213.7757310962907411, 37.55113791807855961 ) ) ;
#2391 = VECTOR ( 'NONE', #322, 1000.000000000000114 ) ;
#2392 = DIRECTION ( 'NONE',  ( 0.7071067811865474617, 8.659560562354932858E-17, 0.7071067811865474617 ) ) ;
#2393 = CARTESIAN_POINT ( 'NONE',  ( 8.062137200540822946, 212.9164362838583315, 27.69886208192143684 ) ) ;
#2394 = AXIS2_PLACEMENT_3D ( 'NONE', #2422, #10096, #23196 ) ;
#2395 = CARTESIAN_POINT ( 'NONE',  ( 57.67499999726880588, 168.2552932293087906, -9.630534252274387086 ) ) ;
#2396 = ORIENTED_EDGE ( 'NONE', *, *, #14305, .T. ) ;
#2397 = CARTESIAN_POINT ( 'NONE',  ( 92.60208470531341618, 155.0000000000000000, 32.00000000000002842 ) ) ;
#2398 = SURFACE_SIDE_STYLE ('',( #2224 ) ) ;
#2399 = CARTESIAN_POINT ( 'NONE',  ( 2.000000000000000000, -1.329782007511004727, 0.7677500000000014868 ) ) ;
#2400 = CARTESIAN_POINT ( 'NONE',  ( -3.135527875058982783, 216.4958274776886924, 99.09886208192143897 ) ) ;
#2401 = CARTESIAN_POINT ( 'NONE',  ( -3.044812012440131443, 216.5253028482142952, 46.10113791807857098 ) ) ;
#2402 = CARTESIAN_POINT ( 'NONE',  ( 10.01549611932653860, 210.2015048109876716, 22.85113791807856742 ) ) ;
#2403 = DIRECTION ( 'NONE',  ( 1.000000000000000000, 0.000000000000000000, 0.000000000000000000 ) ) ;
#2404 = AXIS2_PLACEMENT_3D ( 'NONE', #8872, #11941, #4266 ) ;
#2405 = CARTESIAN_POINT ( 'NONE',  ( 8.000000000000008882, 207.0476921513415220, 84.99886208192144466 ) ) ;
#2406 = CARTESIAN_POINT ( 'NONE',  ( 33.62499999726881583, 171.3844434931184253, -7.942151717890132712E-15 ) ) ;
#2407 = SURFACE_STYLE_FILL_AREA ( #7858 ) ;
#2408 = PLANE ( 'NONE',  #12067 ) ;
#2409 = CARTESIAN_POINT ( 'NONE',  ( 9.736236675707914401, 214.0148392665762458, 13.70113791807856707 ) ) ;
#2410 = DIRECTION ( 'NONE',  ( 0.000000000000000000, 0.000000000000000000, 1.000000000000000000 ) ) ;
#2411 = CARTESIAN_POINT ( 'NONE',  ( 49.17499999726881299, 145.8408176439707802, -12.60653300113719588 ) ) ;
#2412 = CARTESIAN_POINT ( 'NONE',  ( -9.984503880673473830, 210.2968891136704315, 60.65113791807856103 ) ) ;
#2413 = CARTESIAN_POINT ( 'NONE',  ( 86.62499999726883004, 138.6155565068815463, -3.929120461958505118E-15 ) ) ;
#2414 = CARTESIAN_POINT ( 'NONE',  ( 78.01132485994284593, 167.7597621252805880, -9.270509831248443078 ) ) ;
#2415 = DIRECTION ( 'NONE',  ( -0.000000000000000000, 1.100686371591861952E-15, 1.000000000000000000 ) ) ;
#2416 = MECHANICAL_DESIGN_GEOMETRIC_PRESENTATION_REPRESENTATION (  '', ( #13299 ), #21439 ) ;
#2417 = CARTESIAN_POINT ( 'NONE',  ( 52.79999999453763593, 163.5228861582408797, 11.73074641843673049 ) ) ;
#2418 = ORIENTED_EDGE ( 'NONE', *, *, #32627, .T. ) ;
#2419 = CARTESIAN_POINT ( 'NONE',  ( 0.05014649552807549926, 219.6175466908591716, 25.25113791807856956 ) ) ;
#2420 = B_SPLINE_CURVE_WITH_KNOTS ( 'NONE', 3,
 ( #16033, #31218, #15368, #209, #28493, #12988, #5645, #23703, #25760, #26260 ),
 .UNSPECIFIED., .F., .F.,
 ( 4, 2, 2, 2, 4 ),
 ( 0.01606529487141860127, 0.01806591702017404377, 0.02006653916892948628, 0.02406778346644037475, 0.03207027206146215170 ),
 .UNSPECIFIED. ) ;
#2421 = AXIS2_PLACEMENT_3D ( 'NONE', #12261, #33039, #11932 ) ;
#2422 = CARTESIAN_POINT ( 'NONE',  ( 127.5000000000000000, 155.0000000000000000, -6.938893903907228378E-15 ) ) ;
#2423 = CARTESIAN_POINT ( 'NONE',  ( -6.139770520408224463, 198.4640165459539389, 8.048862081921434708 ) ) ;
#2424 = CARTESIAN_POINT ( 'NONE',  ( 32.50000000000000000, 155.0000000000000000, 15.00000000000001243 ) ) ;
#2425 = ORIENTED_EDGE ( 'NONE', *, *, #11054, .T. ) ;
#2426 = CARTESIAN_POINT ( 'NONE',  ( -8.062137200540920645, 212.9164362838581894, 12.80113791807856671 ) ) ;
#2427 = CARTESIAN_POINT ( 'NONE',  ( 10.00000000000000711, 206.9523078486586201, 74.00113791807858377 ) ) ;
#2428 = VERTEX_POINT ( 'NONE', #7346 ) ;
#2429 = CARTESIAN_POINT ( 'NONE',  ( -7.984503880673422316, 204.3529502787951628, 35.34886208192144608 ) ) ;
#2430 = EDGE_CURVE ( 'NONE', #17495, #24155, #17726, .T. ) ;
#2431 = PRESENTATION_LAYER_ASSIGNMENT (  '', '', ( #26347 ) ) ;
#2432 = DIRECTION ( 'NONE',  ( 1.000000000000000000, 0.000000000000000000, 0.000000000000000000 ) ) ;
#2433 = CARTESIAN_POINT ( 'NONE',  ( 79.57499999726881867, 164.1591823560292198, -12.60653300113719766 ) ) ;
#2434 = ORIENTED_EDGE ( 'NONE', *, *, #20489, .T. ) ;
#2435 = CARTESIAN_POINT ( 'NONE',  ( 2.517493886308900919, 214.5937144450984420, 7.401137918078566358 ) ) ;
#2436 = CARTESIAN_POINT ( 'NONE',  ( 12.01549611932659367, 203.1486557965466773, 97.14886208192146455 ) ) ;
#2437 = CARTESIAN_POINT ( 'NONE',  ( 34.67499999726880588, 141.7447067706911810, 9.630534252274376428 ) ) ;
#2438 = ORIENTED_EDGE ( 'NONE', *, *, #17837, .T. ) ;
#2439 = CARTESIAN_POINT ( 'NONE',  ( 41.62499999726880162, 171.3844434931184253, -7.942151717890132712E-15 ) ) ;
#2440 = CARTESIAN_POINT ( 'NONE',  ( 66.78867513459482552, 155.0000000000000000, -15.00000000000002487 ) ) ;
#2441 = EDGE_CURVE ( 'NONE', #28404, #5476, #4849, .T. ) ;
#2442 = CARTESIAN_POINT ( 'NONE',  ( 3.135527875058820690, 216.4958274776887492, 10.40113791807856636 ) ) ;
#2443 = AXIS2_PLACEMENT_3D ( 'NONE', #24136, #3023, #21414 ) ;
#2444 = CARTESIAN_POINT ( 'NONE',  ( 6.139770520408223575, 215.5359834540460611, 75.54886208192139918 ) ) ;
#2445 = CARTESIAN_POINT ( 'NONE',  ( 47.37499999726880873, 155.0000000000000000, -15.58253175000000823 ) ) ;
#2446 = CARTESIAN_POINT ( 'NONE',  ( 89.50000000000001421, 155.0000000000000000, -6.938893903907228378E-15 ) ) ;
#2447 = CARTESIAN_POINT ( 'NONE',  ( -0.05014649552810635652, 196.4853777576173002, 8.751137918078562450 ) ) ;
#2448 = FACE_OUTER_BOUND ( 'NONE', #29818, .T. ) ;
#2449 = CARTESIAN_POINT ( 'NONE',  ( 70.40000000000000568, 150.2886644046228639, -14.50000000000000888 ) ) ;
#2450 = CARTESIAN_POINT ( 'NONE',  ( 6.220909254589536808, 215.4770327129947702, 100.5511379180785809 ) ) ;
#2451 = DIRECTION ( 'NONE',  ( 0.000000000000000000, 0.7071067811865475727, 0.7071067811865475727 ) ) ;
#2452 = CARTESIAN_POINT ( 'NONE',  ( 10.00000000000000711, 206.9523078486586201, 80.00113791807856956 ) ) ;
#2453 = CARTESIAN_POINT ( 'NONE',  ( 4.000000000000000000, -3.004629197474319246E-15, -3.047499999999999876 ) ) ;
#2454 = CARTESIAN_POINT ( 'NONE',  ( 27.50000000000000711, 10.70896984529284879, -1.097913889158304235 ) ) ;
#2455 = CARTESIAN_POINT ( 'NONE',  ( -0.05014649552828442242, 219.6175466908591716, 93.24886208192143044 ) ) ;
#2456 = CARTESIAN_POINT ( 'NONE',  ( 67.52499999726880731, 169.8198683612136222, -4.815267126137197984 ) ) ;
#2457 = ORIENTED_EDGE ( 'NONE', *, *, #7239, .F. ) ;
#2458 = CARTESIAN_POINT ( 'NONE',  ( -59.14934243545564385, 194.9267577168561161, -2.419719764051426747 ) ) ;
#2459 = CARTESIAN_POINT ( 'NONE',  ( 37.39999999453763024, 141.2096805137202580, 4.480746418436733158 ) ) ;
#2460 = CARTESIAN_POINT ( 'NONE',  ( 9.736236675707914401, 214.0148392665762458, 91.70113791807857240 ) ) ;
#2461 = EDGE_CURVE ( 'NONE', #33083, #6207, #11942, .T. ) ;
#2462 = DIRECTION ( 'NONE',  ( -0.000000000000000000, 0.000000000000000000, 1.000000000000000000 ) ) ;
#2463 = ORIENTED_EDGE ( 'NONE', *, *, #19799, .F. ) ;
#2464 = CARTESIAN_POINT ( 'NONE',  ( 3.135527875058981895, 197.5041725223112792, 82.59886208192143897 ) ) ;
#2465 = CARTESIAN_POINT ( 'NONE',  ( 7.375838497908012492, 217.2372850707501186, 21.54886208192143471 ) ) ;
#2466 = CARTESIAN_POINT ( 'NONE',  ( -52.50000000000002132, 155.0000000000000000, 6.938893903907228378E-15 ) ) ;
#2467 = CARTESIAN_POINT ( 'NONE',  ( -3.135527875058821579, 197.5041725223112223, 44.90113791807857524 ) ) ;
#2468 = EDGE_LOOP ( 'NONE', ( #21190, #44, #10482, #2924, #29269, #18804 ) ) ;
#2469 = CARTESIAN_POINT ( 'NONE',  ( 6.500168698208244500, 202.3363017425938324, 1.298862081921434930 ) ) ;
#2470 = EDGE_CURVE ( 'NONE', #11897, #12741, #3041, .T. ) ;
#2471 = CARTESIAN_POINT ( 'NONE',  ( -1.156317065392244547, 3.373851915354613595, -0.02993401039713676146 ) ) ;
#2472 = ORIENTED_EDGE ( 'NONE', *, *, #5437, .T. ) ;
#2473 = CARTESIAN_POINT ( 'NONE',  ( -8.015496119326597224, 209.5516654185217362, 83.64886208192143613 ) ) ;
#2474 = VERTEX_POINT ( 'NONE', #26072 ) ;
#2475 = CARTESIAN_POINT ( 'NONE',  ( 34.41132485994280898, 167.7597621252805880, 9.270509831248428867 ) ) ;
#2476 = VERTEX_POINT ( 'NONE', #2399 ) ;
#2477 = CARTESIAN_POINT ( 'NONE',  ( -67.50000000000000000, 155.0000000000000000, -37.00000000000000000 ) ) ;
#2478 = EDGE_CURVE ( 'NONE', #28367, #26329, #175, .T. ) ;
#2479 = CARTESIAN_POINT ( 'NONE',  ( -8.000000000000008882, 207.0476921513413515, 57.50113791807857666 ) ) ;
#2480 = CARTESIAN_POINT ( 'NONE',  ( 85.82499999726879025, 168.2552932293087906, 9.630534252274372875 ) ) ;
#2481 = CYLINDRICAL_SURFACE ( 'NONE', #11610, 2.149999999999999023 ) ;
#2482 = CARTESIAN_POINT ( 'NONE',  ( 2.426778023690261410, 199.3768101843759837, 89.60113791807857808 ) ) ;
#2483 = DIRECTION ( 'NONE',  ( 0.000000000000000000, 0.000000000000000000, -1.000000000000000000 ) ) ;
#2484 = B_SPLINE_CURVE_WITH_KNOTS ( 'NONE', 3,
 ( #32960, #20020, #7079, #1962, #10974, #6013 ),
 .UNSPECIFIED., .F., .F.,
 ( 4, 2, 4 ),
 ( 0.003605240635278499518, 0.004627368318297494891, 0.005649496001316489831 ),
 .UNSPECIFIED. ) ;
#2485 = CARTESIAN_POINT ( 'NONE',  ( 47.70000000000000284, 146.4771138417591203, 11.73074641843673227 ) ) ;
#2486 = CARTESIAN_POINT ( 'NONE',  ( -7.984503880673422316, 204.3529502787951628, 62.34886208192144608 ) ) ;
#2487 = CARTESIAN_POINT ( 'NONE',  ( -1.474514954580286030E-14, 206.9977241638431167, -6.000000000000014211 ) ) ;
#2488 = ADVANCED_FACE ( 'NONE', ( #2892 ), #10731, .T. ) ;
#2489 = CARTESIAN_POINT ( 'NONE',  ( 53.92499999726881299, 164.1591823560292198, 12.60653300113718167 ) ) ;
#2490 = CARTESIAN_POINT ( 'NONE',  ( 95.70416941062676131, 155.0000000000000000, 0.000000000000000000 ) ) ;
#2491 = PLANE ( 'NONE',  #18442 ) ;
#2492 = CARTESIAN_POINT ( 'NONE',  ( 55.52499999726881441, 169.8198683612136222, -4.815267126137197984 ) ) ;
#2493 = CARTESIAN_POINT ( 'NONE',  ( 71.17499999726881299, 145.8408176439707802, -12.60653300113719588 ) ) ;
#2494 = CARTESIAN_POINT ( 'NONE',  ( 12.01549611932652972, 210.8513442034534933, 70.85113791807857808 ) ) ;
#2495 = FACE_OUTER_BOUND ( 'NONE', #5360, .T. ) ;
#2496 = CARTESIAN_POINT ( 'NONE',  ( 12.01549611932652972, 210.8513442034534933, 7.851137918078565647 ) ) ;
#2497 = CARTESIAN_POINT ( 'NONE',  ( -8.118202686958039038, 201.1607312380087080, 84.20113791807858661 ) ) ;
#2498 = CARTESIAN_POINT ( 'NONE',  ( 9.736236675708031640, 199.9851607334238963, 52.29886208192143471 ) ) ;
#2499 = CARTESIAN_POINT ( 'NONE',  ( -0.05014649552828402690, 217.5146222423826714, 57.24886208192143755 ) ) ;
#2500 = CARTESIAN_POINT ( 'NONE',  ( 32.50000000000000000, 155.0000000000000000, 15.00000000000001243 ) ) ;
#2501 = CARTESIAN_POINT ( 'NONE',  ( 12.00000000000000711, 206.9523078486586485, 95.00113791807856956 ) ) ;
#2502 = LINE ( 'NONE', #15937, #15920 ) ;
#2503 = CARTESIAN_POINT ( 'NONE',  ( -6.220909254589537696, 198.5229672870051161, 18.05113791807856671 ) ) ;
#2504 = CARTESIAN_POINT ( 'NONE',  ( -0.05014649552828403384, 217.5146222423826714, 66.24886208192143044 ) ) ;
#2505 = ORIENTED_EDGE ( 'NONE', *, *, #6759, .F. ) ;
#2506 = CARTESIAN_POINT ( 'NONE',  ( 12.00000000000000711, 207.0476921513415220, 81.99886208192144466 ) ) ;
#2507 = CARTESIAN_POINT ( 'NONE',  ( -9.984503880673473830, 210.2968891136704315, 87.65113791807854682 ) ) ;
#2508 = EDGE_LOOP ( 'NONE', ( #32994, #9884, #9445, #29988 ) ) ;
#2509 = CARTESIAN_POINT ( 'NONE',  ( 76.47499999726881015, 149.9369285172503510, 15.58253174999999580 ) ) ;
#2510 = CARTESIAN_POINT ( 'NONE',  ( -8.015496119326597224, 209.5516654185217362, 47.64886208192145034 ) ) ;
#2511 = EDGE_LOOP ( 'NONE', ( #2793, #21886, #22794, #18548 ) ) ;
#2512 = CARTESIAN_POINT ( 'NONE',  ( 73.32499999726880446, 164.1591823560292198, -12.60653300113719766 ) ) ;
#2513 = CARTESIAN_POINT ( 'NONE',  ( 6.815765296784352500, 0.6502800852031724865, -6.170377922158368555 ) ) ;
#2514 = CARTESIAN_POINT ( 'NONE',  ( 125.5000000000000000, 155.0000000000010800, 106.0000000000000142 ) ) ;
#2515 = CARTESIAN_POINT ( 'NONE',  ( 65.12499999726881583, 155.0000000000000000, -15.58253175000000823 ) ) ;
#2516 = ADVANCED_FACE ( 'NONE', ( #25896 ), #18566, .F. ) ;
#2517 = CARTESIAN_POINT ( 'NONE',  ( 5.000000000000000000, -2.342598717236912265, -4.057499999999995666 ) ) ;
#2518 = ADVANCED_FACE ( 'NONE', ( #31513 ), #5609, .T. ) ;
#2519 = CARTESIAN_POINT ( 'NONE',  ( -6.139770520408224463, 198.4640165459539389, 50.04886208192143471 ) ) ;
#2520 = CIRCLE ( 'NONE', #5235, 6.500000000000000888 ) ;
#2521 = ORIENTED_EDGE ( 'NONE', *, *, #814, .T. ) ;
#2522 = FACE_OUTER_BOUND ( 'NONE', #239, .T. ) ;
#2523 = CARTESIAN_POINT ( 'NONE',  ( 7.908030677224553884, -3.059924800338349904, -7.792662696733364314 ) ) ;
#2524 = CARTESIAN_POINT ( 'NONE',  ( -6.500168698208244500, 211.6636982574061676, 32.79886208192143471 ) ) ;
#2525 = EDGE_CURVE ( 'NONE', #13221, #4173, #16269, .T. ) ;
#2526 = CARTESIAN_POINT ( 'NONE',  ( -6.220909254589537696, 198.5229672870051161, 69.05113791807858092 ) ) ;
#2527 = CARTESIAN_POINT ( 'NONE',  ( 45.68867513459483121, 159.8737954434933499, 15.00000000000019895 ) ) ;
#2528 = EDGE_CURVE ( 'NONE', #5597, #5932, #1587, .T. ) ;
#2529 = CARTESIAN_POINT ( 'NONE',  ( 10.00000000000000711, 206.9523078486586201, 53.00113791807857666 ) ) ;
#2530 = ITEM_DEFINED_TRANSFORMATION ( 'NONE', 'NONE', #21354,  #2404 ) ;
#2531 = CARTESIAN_POINT ( 'NONE',  ( -0.05014649552810635652, 196.4853777576173002, 26.75113791807856956 ) ) ;
#2532 = CARTESIAN_POINT ( 'NONE',  ( 7.984503880673485376, 204.3529502787953902, 11.15113791807856636 ) ) ;
#2533 = CARTESIAN_POINT ( 'NONE',  ( 45.88867513459483405, 150.1262045565061385, 14.99999999999982947 ) ) ;
#2534 = FACE_OUTER_BOUND ( 'NONE', #31931, .T. ) ;
#2535 = CARTESIAN_POINT ( 'NONE',  ( 37.82499999726881157, 168.2552932293087906, 9.630534252274372875 ) ) ;
#2536 = CARTESIAN_POINT ( 'NONE',  ( -11.98450388067348804, 210.9467285061362247, 39.65113791807857524 ) ) ;
#2537 = FACE_BOUND ( 'NONE', #23999, .T. ) ;
#2538 = ADVANCED_FACE ( 'NONE', ( #20623 ), #13438, .T. ) ;
#2539 = CARTESIAN_POINT ( 'NONE',  ( 10.01549611932653860, 210.2015048109876716, 88.85113791807857808 ) ) ;
#2540 = CARTESIAN_POINT ( 'NONE',  ( 6.220909254589536808, 215.4770327129947987, 58.55113791807858092 ) ) ;
#2541 = DIRECTION ( 'NONE',  ( 0.000000000000000000, 0.000000000000000000, -1.000000000000000000 ) ) ;
#2542 = CARTESIAN_POINT ( 'NONE',  ( 7.456977232089471386, 196.8216656703012006, 22.44886208192143329 ) ) ;
#2543 = CARTESIAN_POINT ( 'NONE',  ( -9.984503880673420539, 203.7031108863293980, 32.34886208192143187 ) ) ;
#2544 = CARTESIAN_POINT ( 'NONE',  ( 71.49999999453763166, 139.7537977485451393, -4.138211985947621020E-15 ) ) ;
#2545 = CARTESIAN_POINT ( 'NONE',  ( 11.98450388067348271, 203.0532714938637753, 68.15113791807856103 ) ) ;
#2546 = CARTESIAN_POINT ( 'NONE',  ( 4.903702542908601636, 200.1653181626581102, 80.45113791807857240 ) ) ;
#2547 = CARTESIAN_POINT ( 'NONE',  ( 3.044812012439969795, 216.5253028482143520, 39.39886208192143613 ) ) ;
#2548 = CIRCLE ( 'NONE', #16678, 12.00000000000001066 ) ;
#2549 = CARTESIAN_POINT ( 'NONE',  ( 6.500000000000000000, 3.752776749732563921, -8.000000000000000000 ) ) ;
#2550 = ORIENTED_EDGE ( 'NONE', *, *, #8975, .F. ) ;
#2551 = CARTESIAN_POINT ( 'NONE',  ( -7.375838497908014268, 196.7627149292498530, 50.04886208192142760 ) ) ;
#2552 = CLOSED_SHELL ( 'NONE', ( #14178, #11432, #7090, #30837, #30292, #9393, #21364, #29876, #20785, #33222, #582, #29313, #784, #22912, #3831, #30402, #13477, #17247, #31221, #21046, #25635, #9358, #22087, #18319, #5590, #32889, #8098 ) ) ;
#2553 = ORIENTED_EDGE ( 'NONE', *, *, #21809, .T. ) ;
#2554 = ORIENTED_EDGE ( 'NONE', *, *, #28844, .F. ) ;
#2555 = CIRCLE ( 'NONE', #3607, 5.249999999999991118 ) ;
#2556 = DIRECTION ( 'NONE',  ( -1.000000000000000000, -0.000000000000000000, -0.000000000000000000 ) ) ;
#2557 = CARTESIAN_POINT ( 'NONE',  ( 55.98867513459482126, 146.1832212156128890, 12.13525491562421976 ) ) ;
#2558 = ORIENTED_EDGE ( 'NONE', *, *, #13893, .F. ) ;
#2559 = CARTESIAN_POINT ( 'NONE',  ( 4.903702542908601636, 200.1653181626581102, 38.45113791807856529 ) ) ;
#2560 = DIRECTION ( 'NONE',  ( 0.000000000000000000, 0.000000000000000000, -1.000000000000000000 ) ) ;
#2561 = CARTESIAN_POINT ( 'NONE',  ( -8.118202686958138514, 212.8392687619910930, 23.79886208192143471 ) ) ;
#2562 = CARTESIAN_POINT ( 'NONE',  ( 60.47499999726880304, 149.9369285172503510, 15.58253174999999580 ) ) ;
#2563 = EDGE_LOOP ( 'NONE', ( #6399, #7677, #30970, #31090 ) ) ;
#2564 = CARTESIAN_POINT ( 'NONE',  ( -58.50000000000002132, 209.9999999999999716, 2.500000000000000000 ) ) ;
#2565 = SHAPE_REPRESENTATION_RELATIONSHIP ( 'NONE' , 'NONE' ,  #2185, #14909 ) ;
#2566 = DIRECTION ( 'NONE',  ( -0.000000000000000000, -0.000000000000000000, 1.000000000000000000 ) ) ;
#2567 = CARTESIAN_POINT ( 'NONE',  ( -2.517493886309087880, 214.5937144450984135, 3.098862081921434974 ) ) ;
#2568 = CARTESIAN_POINT ( 'NONE',  ( 10.00000000000000711, 206.9523078486586201, 44.00113791807857666 ) ) ;
#2569 = CARTESIAN_POINT ( 'NONE',  ( 0.000000000000000000, -4.685197434473814759, 3.903127820947815962E-15 ) ) ;
#2570 = CARTESIAN_POINT ( 'NONE',  ( -0.05014649552810635652, 196.4853777576173002, 29.75113791807856956 ) ) ;
#2571 = DIRECTION ( 'NONE',  ( 1.000000000000000000, 0.000000000000000000, 0.000000000000000000 ) ) ;
#2572 = AXIS2_PLACEMENT_3D ( 'NONE', #3204, #8166, #26209 ) ;
#2573 = APPLICATION_PROTOCOL_DEFINITION ( 'draft international standard', 'automotive_design', 1998, #13745 ) ;
#2574 = AXIS2_PLACEMENT_3D ( 'NONE', #8335, #13936, #6089 ) ;
#2575 = CARTESIAN_POINT ( 'NONE',  ( -8.000000000000008882, 206.9523078486584780, 92.49886208192144466 ) ) ;
#2576 = CARTESIAN_POINT ( 'NONE',  ( 35.02499999726880020, 149.9369285172503510, -15.58253175000000823 ) ) ;
#2577 = CARTESIAN_POINT ( 'NONE',  ( 4.200000000000001954, 0.000000000000000000, 0.000000000000000000 ) ) ;
#2578 = CARTESIAN_POINT ( 'NONE',  ( -25.25067902531498376, 17.17577847294296234, -16.29357272760983477 ) ) ;
#2579 = CARTESIAN_POINT ( 'NONE',  ( 7.456977232089302632, 217.1783343296989131, 7.551137918078564049 ) ) ;
#2580 = CARTESIAN_POINT ( 'NONE',  ( 48.08867513459482268, 142.2402378747194405, 9.270509831248432420 ) ) ;
#2581 = CARTESIAN_POINT ( 'NONE',  ( 49.77499999726880731, 169.8198683612136222, -4.815267126137197984 ) ) ;
#2582 = CARTESIAN_POINT ( 'NONE',  ( -8.062137200540920645, 212.9164362838581894, 57.80113791807857382 ) ) ;
#2583 = AXIS2_PLACEMENT_3D ( 'NONE', #27846, #1964, #30933 ) ;
#2584 = CARTESIAN_POINT ( 'NONE',  ( 34.71132485994281325, 155.0000000000000000, 15.00000000000001243 ) ) ;
#2585 = CARTESIAN_POINT ( 'NONE',  ( -3.250000000000003997, -5.629165124598849879, 0.000000000000000000 ) ) ;
#2586 = CARTESIAN_POINT ( 'NONE',  ( 65.61132485994279762, 150.1262045565062806, -14.99999999999993072 ) ) ;
#2587 = CARTESIAN_POINT ( 'NONE',  ( 54.09999999453763309, 159.7113355953771077, -14.50000000000000888 ) ) ;
#2588 = VERTEX_POINT ( 'NONE', #23507 ) ;
#2589 = CARTESIAN_POINT ( 'NONE',  ( 9.736236675707914401, 214.0148392665762458, 37.70113791807857240 ) ) ;
#2590 = CARTESIAN_POINT ( 'NONE',  ( 47.71132485994280614, 155.0000000000000000, -15.00000000000002487 ) ) ;
#2591 = CARTESIAN_POINT ( 'NONE',  ( -0.05014649552828403384, 217.5146222423826714, 12.24886208192143755 ) ) ;
#2592 = CARTESIAN_POINT ( 'NONE',  ( 59.81132485994281467, 159.8737954434935489, -15.00000000000007638 ) ) ;
#2593 = EDGE_LOOP ( 'NONE', ( #30834, #2607, #27081, #23781 ) ) ;
#2594 = CARTESIAN_POINT ( 'NONE',  ( 0.05014649552810505201, 217.5146222423826714, 13.25113791807856778 ) ) ;
#2595 = CARTESIAN_POINT ( 'NONE',  ( -3.135527875058821579, 197.5041725223112223, 74.90113791807857524 ) ) ;
#2596 = TOROIDAL_SURFACE ( 'NONE', #21608, 8.331345277524542681, 0.6186547224754559426 ) ;
#2597 = VERTEX_POINT ( 'NONE', #7515 ) ;
#2598 = CARTESIAN_POINT ( 'NONE',  ( 6.500168698208244500, 202.3363017425938324, 34.29886208192144181 ) ) ;
#2599 = VECTOR ( 'NONE', #8286, 1000.000000000000000 ) ;
#2600 = AXIS2_PLACEMENT_3D ( 'NONE', #18352, #25681, #4726 ) ;
#2601 = FACE_OUTER_BOUND ( 'NONE', #15989, .T. ) ;
#2602 = ORIENTED_EDGE ( 'NONE', *, *, #5442, .T. ) ;
#2603 = CARTESIAN_POINT ( 'NONE',  ( -2.517493886308901807, 199.4062855549015012, 14.90113791807856636 ) ) ;
#2604 = CARTESIAN_POINT ( 'NONE',  ( -3.662846001189865142, 195.5725841191952838, 97.89886208192146455 ) ) ;
#2605 = CARTESIAN_POINT ( 'NONE',  ( 45.37499999726880873, 155.0000000000000000, -15.58253175000000823 ) ) ;
#2607 = ORIENTED_EDGE ( 'NONE', *, *, #7532, .T. ) ;
#2606 = AXIS2_PLACEMENT_3D ( 'NONE', #2487, #31106, #7768 ) ;
#2608 = CARTESIAN_POINT ( 'NONE',  ( 47.82499999726881867, 168.2552932293087906, 9.630534252274372875 ) ) ;
#2609 = DIRECTION ( 'NONE',  ( 0.000000000000000000, 0.000000000000000000, 1.000000000000000000 ) ) ;
#2610 = CARTESIAN_POINT ( 'NONE',  ( -10.01549611932653860, 203.7984951890123284, 9.351137918078569200 ) ) ;
#2611 = CARTESIAN_POINT ( 'NONE',  ( 6.139770520408223575, 215.5359834540460611, 84.54886208192141339 ) ) ;
#2612 = CARTESIAN_POINT ( 'NONE',  ( 46.87499999726880873, 138.6155565068815463, -3.929120461958505118E-15 ) ) ;
#2613 = CARTESIAN_POINT ( 'NONE',  ( -67.50001199999996970, 138.8682562219733541, -5.477666192157146341 ) ) ;
#2614 = CARTESIAN_POINT ( 'NONE',  ( -3.044812012440131443, 216.5253028482142952, 13.10113791807856742 ) ) ;
#2615 = DIRECTION ( 'NONE',  ( 1.000000000000000000, 0.000000000000000000, 0.000000000000000000 ) ) ;
#2616 = CARTESIAN_POINT ( 'NONE',  ( 70.60000000000000853, 159.7113355953771077, -14.50000000000000888 ) ) ;
#2617 = CARTESIAN_POINT ( 'NONE',  ( -10.00000000000000711, 207.0476921513413515, 96.50113791807856956 ) ) ;
#2618 = CARTESIAN_POINT ( 'NONE',  ( 37.78867513459481842, 155.0000000000000000, 15.00000000000001243 ) ) ;
#2619 = CARTESIAN_POINT ( 'NONE',  ( 10.00000000000000711, 206.9523078486586201, 83.00113791807856956 ) ) ;
#2620 = AXIS2_PLACEMENT_3D ( 'NONE', #27731, #32498, #4567 ) ;
#2621 = CARTESIAN_POINT ( 'NONE',  ( -27.50000000000000000, 13.30988860919478078, -1.715101482986570502 ) ) ;
#2622 = FACE_OUTER_BOUND ( 'NONE', #4761, .T. ) ;
#2623 = CARTESIAN_POINT ( 'NONE',  ( -7.375838497908014268, 196.7627149292498530, 92.04886208192142760 ) ) ;
#2624 = EDGE_CURVE ( 'NONE', #33027, #13306, #29875, .T. ) ;
#2625 = CIRCLE ( 'NONE', #23284, 2.149999999999985256 ) ;
#2626 = CARTESIAN_POINT ( 'NONE',  ( 69.02499999726880731, 149.9369285172503510, -15.58253175000000823 ) ) ;
#2627 = AXIS2_PLACEMENT_3D ( 'NONE', #9466, #21900, #19349 ) ;
#2628 = EDGE_LOOP ( 'NONE', ( #28820, #26747, #6296, #23074, #16613, #15198 ) ) ;
#2629 = CARTESIAN_POINT ( 'NONE',  ( 58.71132485994280614, 155.0000000000000000, 15.00000000000001243 ) ) ;
#2630 = CARTESIAN_POINT ( 'NONE',  ( 86.67499999726878457, 141.7447067706911810, 9.630534252274376428 ) ) ;
#2631 = CARTESIAN_POINT ( 'NONE',  ( 12.00000000000000711, 206.9523078486586485, 98.00113791807856956 ) ) ;
#2632 = DIRECTION ( 'NONE',  ( 0.000000000000000000, 0.000000000000000000, 1.000000000000000000 ) ) ;
#2633 = VECTOR ( 'NONE', #33063, 1000.000000000000000 ) ;
#2634 = ORIENTED_EDGE ( 'NONE', *, *, #11989, .T. ) ;
#2635 = CARTESIAN_POINT ( 'NONE',  ( 10.00000000000000711, 207.0476921513415220, 90.99886208192144466 ) ) ;
#2636 = CARTESIAN_POINT ( 'NONE',  ( -3.662846001189865142, 195.5725841191952838, 19.89886208192143613 ) ) ;
#2637 = DIRECTION ( 'NONE',  ( -1.000000000000000000, 0.000000000000000000, 0.000000000000000000 ) ) ;
#2638 = CARTESIAN_POINT ( 'NONE',  ( 10.01549611932653860, 210.2015048109876716, 40.85113791807857098 ) ) ;
#2639 = ORIENTED_EDGE ( 'NONE', *, *, #25144, .T. ) ;
#2640 = CARTESIAN_POINT ( 'NONE',  ( 0.05014649552828262524, 198.5883022060938572, 1.748862081921434886 ) ) ;
#2641 = DIRECTION ( 'NONE',  ( -1.000000000000000000, -0.000000000000000000, 0.000000000000000000 ) ) ;
#2642 = EDGE_LOOP ( 'NONE', ( #28613, #26321, #25959, #14763 ) ) ;
#2643 = CARTESIAN_POINT ( 'NONE',  ( 8.000000000000008882, 207.0476921513415220, 87.99886208192144466 ) ) ;
#2644 = CIRCLE ( 'NONE', #443, 0.9999999999999992228 ) ;
#2645 = ORIENTED_EDGE ( 'NONE', *, *, #30971, .F. ) ;
#2646 = CIRCLE ( 'NONE', #4824, 24.99999999999999289 ) ;
#2647 = CARTESIAN_POINT ( 'NONE',  ( 8.000000000000008882, 206.9523078486586485, 35.00113791807857666 ) ) ;
#2648 = CARTESIAN_POINT ( 'NONE',  ( 55.91132485994280898, 163.8167787843871110, -12.13525491562423397 ) ) ;
#2649 = EDGE_LOOP ( 'NONE', ( #10358, #32918, #23450 ) ) ;
#2650 = CARTESIAN_POINT ( 'NONE',  ( 34.22499999726881015, 149.9369285172503510, 15.58253174999999580 ) ) ;
#2651 = CARTESIAN_POINT ( 'NONE',  ( 82.32499999726880446, 145.8408176439707802, 12.60653300113718345 ) ) ;
#2652 = LINE ( 'NONE', #25643, #15958 ) ;
#2653 = CARTESIAN_POINT ( 'NONE',  ( 4.984841277089725686, 213.7757310962907411, 88.55113791807858092 ) ) ;
#2654 = LINE ( 'NONE', #10493, #13003 ) ;
#2655 = VECTOR ( 'NONE', #29930, 1000.000000000000000 ) ;
#2656 = FILL_AREA_STYLE ('',( #31433 ) ) ;
#2657 = CARTESIAN_POINT ( 'NONE',  ( 46.70000000000000284, 163.5228861582408797, -11.73074641843674470 ) ) ;
#2658 = CARTESIAN_POINT ( 'NONE',  ( 8.000000000000008882, 207.0476921513415220, 63.99886208192143044 ) ) ;
#2659 = CARTESIAN_POINT ( 'NONE',  ( 92.60208470531341618, 155.0000000000000000, 12.10452846326765020 ) ) ;
#2660 = EDGE_CURVE ( 'NONE', #23167, #9113, #12785, .T. ) ;
#2661 = CARTESIAN_POINT ( 'NONE',  ( 54.32499999726880446, 145.8408176439707802, 12.60653300113718345 ) ) ;
#2662 = CARTESIAN_POINT ( 'NONE',  ( -8.062137200540920645, 212.9164362838581894, 0.8011379180785658249 ) ) ;
#2663 = CARTESIAN_POINT ( 'NONE',  ( -2.500000000000000000, 7.216878364870324525, -7.063244554130001518 ) ) ;
#2664 = CARTESIAN_POINT ( 'NONE',  ( 56.52499999726881441, 140.1801316387863778, 4.815267126137185549 ) ) ;
#2665 = CARTESIAN_POINT ( 'NONE',  ( 71.07499999726880446, 141.7447067706911810, -9.630534252274385310 ) ) ;
#2666 = CARTESIAN_POINT ( 'NONE',  ( 7.375838497908181246, 196.7627149292499666, 71.45113791807854398 ) ) ;
#2667 = LINE ( 'NONE', #7776, #31465 ) ;
#2668 = AXIS2_PLACEMENT_3D ( 'NONE', #29695, #24760, #11645 ) ;
#2669 = CARTESIAN_POINT ( 'NONE',  ( -3.753561863808691168, 195.6020594897209435, 11.90113791807856813 ) ) ;
#2670 = CARTESIAN_POINT ( 'NONE',  ( 10.00000000000000711, 206.9523078486586201, 83.00113791807856956 ) ) ;
#2671 = CARTESIAN_POINT ( 'NONE',  ( 85.38867513459483405, 169.2658477444273331, 4.635254915624208216 ) ) ;
#2672 = ADVANCED_FACE ( 'NONE', ( #5115 ), #23962, .F. ) ;
#2673 = VECTOR ( 'NONE', #2311, 1000.000000000000000 ) ;
#2674 = CARTESIAN_POINT ( 'NONE',  ( 7.456977232089471386, 196.8216656703012006, 49.44886208192144039 ) ) ;
#2675 = CARTESIAN_POINT ( 'NONE',  ( 0.05014649552828275014, 196.4853777576173002, 58.74886208192143044 ) ) ;
#2676 = CARTESIAN_POINT ( 'NONE',  ( -3.662846001190052991, 218.4274158808045740, 94.10113791807857808 ) ) ;
#2677 = CARTESIAN_POINT ( 'NONE',  ( -67.50001199999998391, 159.4078036646551197, 16.45628302766014528 ) ) ;
#2678 = CARTESIAN_POINT ( 'NONE',  ( -9.984503880673473830, 210.2968891136704315, 9.651137918078568134 ) ) ;
#2679 = CARTESIAN_POINT ( 'NONE',  ( 0.05014649552828275708, 196.4853777576173002, 79.74886208192143044 ) ) ;
#2680 = APPLICATION_CONTEXT ( 'automotive_design' ) ;
#2681 = AXIS2_PLACEMENT_3D ( 'NONE', #20295, #24901, #6678 ) ;
#2682 = ORIENTED_EDGE ( 'NONE', *, *, #14249, .T. ) ;
#2683 = CARTESIAN_POINT ( 'NONE',  ( 0.05014649552828288198, 194.3824533091408000, 79.74886208192143044 ) ) ;
#2684 = DIRECTION ( 'NONE',  ( -1.000000000000000000, -0.000000000000000000, -0.000000000000000000 ) ) ;
#2685 = VERTEX_POINT ( 'NONE', #20952 ) ;
#2686 = DIRECTION ( 'NONE',  ( -1.000000000000000000, -0.000000000000000000, -0.000000000000000000 ) ) ;
#2687 = CARTESIAN_POINT ( 'NONE',  ( 2.517493886309087436, 199.4062855549015865, 58.59886208192145318 ) ) ;
#2688 = EDGE_LOOP ( 'NONE', ( #32080, #32577, #29359, #16102 ) ) ;
#2689 = ADVANCED_FACE ( 'NONE', ( #10408 ), #31346, .T. ) ;
#2690 = CARTESIAN_POINT ( 'NONE',  ( 74.52499999726880731, 140.1801316387863778, 4.815267126137185549 ) ) ;
#2691 = DIRECTION ( 'NONE',  ( 0.000000000000000000, 0.000000000000000000, 1.000000000000000000 ) ) ;
#2692 = CARTESIAN_POINT ( 'NONE',  ( -56.08018104464575515, 194.9950560901275480, -0.6488614982153378952 ) ) ;
#2693 = CIRCLE ( 'NONE', #19527, 4.200000000000001954 ) ;
#2694 = EDGE_CURVE ( 'NONE', #23832, #31784, #22331, .T. ) ;
#2695 = CARTESIAN_POINT ( 'NONE',  ( 62.22499999726881725, 149.9369285172503510, 15.58253174999999580 ) ) ;
#2696 = CARTESIAN_POINT ( 'NONE',  ( 92.60208470531341618, 155.0000000000000000, -12.99999999999999822 ) ) ;
#2697 = CARTESIAN_POINT ( 'NONE',  ( -3.044812012439970683, 197.4746971517856196, 49.89886208192143613 ) ) ;
#2698 = ORIENTED_EDGE ( 'NONE', *, *, #15203, .T. ) ;
#2699 = DIRECTION ( 'NONE',  ( 0.000000000000000000, 1.000000000000000000, -9.859324684083082301E-16 ) ) ;
#2700 = FILL_AREA_STYLE_COLOUR ( '', #6226 ) ;
#2701 = CARTESIAN_POINT ( 'NONE',  ( 42.71132485994280614, 155.0000000000000000, 15.00000000000001243 ) ) ;
#2702 = CARTESIAN_POINT ( 'NONE',  ( 4.984841277089891776, 200.2242689037093726, 37.44886208192144039 ) ) ;
#2703 = CARTESIAN_POINT ( 'NONE',  ( -6.220909254589537696, 198.5229672870051161, 75.05113791807858092 ) ) ;
#2704 = FACE_OUTER_BOUND ( 'NONE', #11685, .T. ) ;
#2705 = CARTESIAN_POINT ( 'NONE',  ( 10.00000000000000711, 206.9523078486586201, 56.00113791807856956 ) ) ;
#2706 = CARTESIAN_POINT ( 'NONE',  ( -3.044812012440131443, 216.5253028482142952, 28.10113791807857098 ) ) ;
#2707 = CARTESIAN_POINT ( 'NONE',  ( 2.517493886308900919, 214.5937144450984420, 16.40113791807856458 ) ) ;
#2708 = CARTESIAN_POINT ( 'NONE',  ( 87.17499999726881299, 145.8408176439707802, -12.60653300113719588 ) ) ;
#2709 = CARTESIAN_POINT ( 'NONE',  ( -150.0000000000000000, 0.000000000000000000, 35.00000000000000000 ) ) ;
#2710 = CARTESIAN_POINT ( 'NONE',  ( 36.52499999726881441, 140.1801316387863778, 4.815267126137185549 ) ) ;
#2711 =( BOUNDED_CURVE ( )  B_SPLINE_CURVE ( 2, ( #10898, #32162, #21275, #19055, #3548, #18730, #24503, #31671, #26391, #26547, #13941 ),
 .UNSPECIFIED., .F., .T. ) 
 B_SPLINE_CURVE_WITH_KNOTS ( ( 3, 2, 2, 2, 2, 3 ),
 ( 0.03571428571428574700, 0.03928571428571431962, 0.04285714285714289917, 0.04642857142857147179, 0.05000000000000005135, 0.05357142857142861703 ),
 .UNSPECIFIED. ) 
 CURVE ( )  GEOMETRIC_REPRESENTATION_ITEM ( )  RATIONAL_B_SPLINE_CURVE ( ( 0.9999999999999995559, 0.9510565162951538642, 1.000000000000000000, 0.9510565162951534202, 1.000000000000000000, 0.9510565162951534202, 1.000000000000000000, 0.9510565162951534202, 1.000000000000000000, 0.9510565162951527540, 1.000000000000000666 ) ) 
 REPRESENTATION_ITEM ( '' )  );
#2712 = CARTESIAN_POINT ( 'NONE',  ( -9.736236675707914401, 199.9851607334237542, 39.20113791807857240 ) ) ;
#2713 = DIRECTION ( 'NONE',  ( -0.000000000000000000, -0.000000000000000000, 1.000000000000000000 ) ) ;
#2714 = CARTESIAN_POINT ( 'NONE',  ( 10.00000000000000711, 206.9523078486586201, 86.00113791807858377 ) ) ;
#2715 = CARTESIAN_POINT ( 'NONE',  ( 0.05014649552810506589, 217.5146222423826714, 58.25113791807856956 ) ) ;
#2716 = CARTESIAN_POINT ( 'NONE',  ( 12.01549611932659367, 203.1486557965466773, 19.14886208192143968 ) ) ;
#2717 = CARTESIAN_POINT ( 'NONE',  ( -3.135527875058982783, 216.4958274776886924, 33.09886208192143187 ) ) ;
#2718 = CARTESIAN_POINT ( 'NONE',  ( 80.89999999453763735, 159.7113355953771077, 14.49999999999999289 ) ) ;
#2719 = CARTESIAN_POINT ( 'NONE',  ( -3.662846001190052991, 218.4274158808045740, 70.10113791807857808 ) ) ;
#2720 = CIRCLE ( 'NONE', #30454, 3.499999999999996003 ) ;
#2721 = CARTESIAN_POINT ( 'NONE',  ( -2.426778023690262742, 214.6231898156240163, 85.10113791807857808 ) ) ;
#2722 = EDGE_CURVE ( 'NONE', #6290, #15366, #17716, .T. ) ;
#2723 = CARTESIAN_POINT ( 'NONE',  ( -0.05014649552828403384, 217.5146222423826714, 51.24886208192143755 ) ) ;
#2724 = ADVANCED_FACE ( 'NONE', ( #3723 ), #21946, .T. ) ;
#2725 = CARTESIAN_POINT ( 'NONE',  ( 48.98867513459481415, 163.8167787843871110, -12.13525491562423397 ) ) ;
#2726 = VERTEX_POINT ( 'NONE', #13943 ) ;
#2727 = CARTESIAN_POINT ( 'NONE',  ( 9.736236675708031640, 199.9851607334238963, 55.29886208192143471 ) ) ;
#2728 = VERTEX_POINT ( 'NONE', #14113 ) ;
#2729 = ORIENTED_EDGE ( 'NONE', *, *, #1692, .T. ) ;
#2730 = EDGE_CURVE ( 'NONE', #20904, #29148, #11559, .T. ) ;
#2731 = DIRECTION ( 'NONE',  ( 0.000000000000000000, 0.000000000000000000, 1.000000000000000000 ) ) ;
#2732 = DIRECTION ( 'NONE',  ( 1.000000000000000000, 0.000000000000000000, 0.000000000000000000 ) ) ;
#2733 = ORIENTED_EDGE ( 'NONE', *, *, #21234, .T. ) ;
#2734 = CARTESIAN_POINT ( 'NONE',  ( -2.426778023690262742, 214.6231898156240163, 46.10113791807857098 ) ) ;
#2735 = EDGE_CURVE ( 'NONE', #20904, #6439, #27778, .T. ) ;
#2736 = SURFACE_STYLE_USAGE ( .BOTH. , #23170 ) ;
#2737 = CARTESIAN_POINT ( 'NONE',  ( 8.062137200540822946, 212.9164362838583315, 18.69886208192143329 ) ) ;
#2738 = CARTESIAN_POINT ( 'NONE',  ( 63.67499999726880588, 168.2552932293087906, -9.630534252274387086 ) ) ;
#2739 = ORIENTED_EDGE ( 'NONE', *, *, #23532, .F. ) ;
#2740 = CARTESIAN_POINT ( 'NONE',  ( -67.50000000000000000, 155.0000000000000000, 6.938893903907228378E-15 ) ) ;
#2741 = ADVANCED_BREP_SHAPE_REPRESENTATION ( '', ( #23155, #2404 ), #13844 ) ;
#2742 = CARTESIAN_POINT ( 'NONE',  ( -0.6508621380849236582, -8.763657152406455708, -7.907633014911225722 ) ) ;
#2743 = CARTESIAN_POINT ( 'NONE',  ( -6.444103211790928043, 202.2591342207265939, 5.198862081921435063 ) ) ;
#2744 = CARTESIAN_POINT ( 'NONE',  ( -8.062137200540920645, 212.9164362838581894, 42.80113791807857382 ) ) ;
#2745 = SURFACE_STYLE_USAGE ( .BOTH. , #15337 ) ;
#2746 = CARTESIAN_POINT ( 'NONE',  ( -0.05014649552810635652, 196.4853777576173002, 26.75113791807856956 ) ) ;
#2747 = CARTESIAN_POINT ( 'NONE',  ( 8.118202686958138514, 201.1607312380088501, 103.2988620819214418 ) ) ;
#2748 = DIRECTION ( 'NONE',  ( 0.9237280213470682178, 0.3830490080632377725, 1.131240564625405124E-16 ) ) ;
#2749 = CARTESIAN_POINT ( 'NONE',  ( -2.517493886309087880, 214.5937144450984135, 90.09886208192143897 ) ) ;
#2750 = CARTESIAN_POINT ( 'NONE',  ( 83.70000000000000284, 146.4771138417591203, 11.73074641843673227 ) ) ;
#2751 = DIRECTION ( 'NONE',  ( 1.000000000000000000, 0.000000000000000000, 0.000000000000000000 ) ) ;
#2752 = CARTESIAN_POINT ( 'NONE',  ( -12.01549611932652972, 203.1486557965464499, 12.35113791807856565 ) ) ;
#2753 = CARTESIAN_POINT ( 'NONE',  ( 60.63708498984762940, 155.0000000000000000, 6.938893903907228378E-15 ) ) ;
#2754 = CARTESIAN_POINT ( 'NONE',  ( 58.57499999726881157, 145.8408176439707802, 12.60653300113718345 ) ) ;
#2755 = CARTESIAN_POINT ( 'NONE',  ( 10.01549611932653860, 210.2015048109876716, 55.85113791807857808 ) ) ;
#2756 = CARTESIAN_POINT ( 'NONE',  ( 87.82499999726881867, 168.2552932293087906, 9.630534252274372875 ) ) ;
#2757 = DIRECTION ( 'NONE',  ( 1.000000000000000000, 0.000000000000000000, 0.000000000000000000 ) ) ;
#2758 = CARTESIAN_POINT ( 'NONE',  ( 10.01549611932659367, 203.7984951890124421, 1.148862081921434131 ) ) ;
#2759 = CARTESIAN_POINT ( 'NONE',  ( 62.89999999453763024, 159.7113355953771077, 14.49999999999999289 ) ) ;
#2760 = VERTEX_POINT ( 'NONE', #11222 ) ;
#2761 = CARTESIAN_POINT ( 'NONE',  ( 3.753561863808689836, 218.3979405102790565, 34.40113791807856813 ) ) ;
#2762 = CARTESIAN_POINT ( 'NONE',  ( 37.78867513459481842, 155.0000000000000000, 15.00000000000001243 ) ) ;
#2763 = CARTESIAN_POINT ( 'NONE',  ( 6.139770520408223575, 215.5359834540460611, 12.54886208192143648 ) ) ;
#2764 = ADVANCED_FACE ( 'NONE', ( #24506 ), #32337, .F. ) ;
#2765 = CARTESIAN_POINT ( 'NONE',  ( 59.91132485994281609, 163.8167787843871110, -12.13525491562423397 ) ) ;
#2766 = ORIENTED_EDGE ( 'NONE', *, *, #20533, .F. ) ;
#2767 = CARTESIAN_POINT ( 'NONE',  ( 8.118202686958039038, 212.8392687619912635, 73.70113791807857240 ) ) ;
#2768 = ORIENTED_EDGE ( 'NONE', *, *, #19308, .F. ) ;
#2769 = CARTESIAN_POINT ( 'NONE',  ( -4.903702542908436435, 200.1653181626580249, 29.04886208192143471 ) ) ;
#2770 = CARTESIAN_POINT ( 'NONE',  ( 0.000000000000000000, 0.000000000000000000, 0.000000000000000000 ) ) ;
#2771 = ORIENTED_EDGE ( 'NONE', *, *, #17842, .F. ) ;
#2772 = CARTESIAN_POINT ( 'NONE',  ( 0.05014649552807626948, 215.4116977939061144, 13.25113791807856423 ) ) ;
#2773 = CARTESIAN_POINT ( 'NONE',  ( -0.05014649552828442242, 219.6175466908591716, 99.24886208192143044 ) ) ;
#2774 = AXIS2_PLACEMENT_3D ( 'NONE', #31193, #5458, #4959 ) ;
#2775 = CARTESIAN_POINT ( 'NONE',  ( 41.67499999726881299, 168.2552932293087906, -9.630534252274387086 ) ) ;
#2776 = ORIENTED_EDGE ( 'NONE', *, *, #33029, .F. ) ;
#2777 = CARTESIAN_POINT ( 'NONE',  ( 52.92499999726881299, 145.8408176439707802, -12.60653300113719588 ) ) ;
#2778 = CARTESIAN_POINT ( 'NONE',  ( 2.000000000000000000, 0.000000000000000000, 0.000000000000000000 ) ) ;
#2779 = CARTESIAN_POINT ( 'NONE',  ( -8.118202686958039038, 201.1607312380087080, 6.201137918078566180 ) ) ;
#2780 = CARTESIAN_POINT ( 'NONE',  ( -8.118202686958138514, 212.8392687619910930, 77.79886208192144181 ) ) ;
#2781 = CARTESIAN_POINT ( 'NONE',  ( 54.17499999726881299, 164.1591823560292198, 12.60653300113718167 ) ) ;
#2782 = CARTESIAN_POINT ( 'NONE',  ( 78.81132485994281467, 150.1262045565064227, 15.00000000000001599 ) ) ;
#2783 = CARTESIAN_POINT ( 'NONE',  ( -8.118202686958039038, 201.1607312380087080, 12.20113791807856707 ) ) ;
#2784 = CARTESIAN_POINT ( 'NONE',  ( 79.50000000000000000, 155.0000000000000000, -69.99999999999998579 ) ) ;
#2785 = CARTESIAN_POINT ( 'NONE',  ( 67.00000000000001421, 170.2462022514548323, -7.872454543227099337E-15 ) ) ;
#2786 = FACE_BOUND ( 'NONE', #10971, .T. ) ;
#2787 = FACE_OUTER_BOUND ( 'NONE', #5141, .T. ) ;
#2788 = CARTESIAN_POINT ( 'NONE',  ( 6.220909254589536808, 215.4770327129947702, 88.55113791807853829 ) ) ;
#2789 = CARTESIAN_POINT ( 'NONE',  ( 56.88867513459482694, 159.8737954434937478, -14.99999999999993072 ) ) ;
#2790 = CARTESIAN_POINT ( 'NONE',  ( 38.67499999726879878, 141.7447067706911810, 9.630534252274376428 ) ) ;
#2791 = CARTESIAN_POINT ( 'NONE',  ( -9.680171189290716072, 199.9079932115567146, 95.19886208192144750 ) ) ;
#2792 = CARTESIAN_POINT ( 'NONE',  ( 69.62499999726883004, 171.3844434931184253, -7.942151717890132712E-15 ) ) ;
#2793 = ORIENTED_EDGE ( 'NONE', *, *, #5823, .T. ) ;
#2794 = CARTESIAN_POINT ( 'NONE',  ( -60.87270596256635713, 194.9921970430798979, -0.8044259506661830539 ) ) ;
#2795 = CARTESIAN_POINT ( 'NONE',  ( 36.69999999453762740, 167.3344367211045096, 8.961492836873468093 ) ) ;
#2796 = CARTESIAN_POINT ( 'NONE',  ( -0.05014649552807705357, 194.3824533091408000, 92.75113791807858377 ) ) ;
#2797 = CARTESIAN_POINT ( 'NONE',  ( 0.1999999999999987899, 4.041334437186265510E-16, -3.299999999999999822 ) ) ;
#2798 = EDGE_LOOP ( 'NONE', ( #23207, #14517, #8782, #25710 ) ) ;
#2799 = CARTESIAN_POINT ( 'NONE',  ( -6.220909254589682469, 215.4770327129947134, 98.94886208192143329 ) ) ;
#2800 = CARTESIAN_POINT ( 'NONE',  ( 0.05014649552828288198, 194.3824533091408000, 22.74886208192143755 ) ) ;
#2801 = DIRECTION ( 'NONE',  ( 0.000000000000000000, 0.4999999999999990008, -0.8660254037844391517 ) ) ;
#2802 = CARTESIAN_POINT ( 'NONE',  ( -6.139770520408369237, 215.5359834540460042, 39.95113791807857240 ) ) ;
#2803 = ORIENTED_EDGE ( 'NONE', *, *, #31409, .F. ) ;
#2804 = CARTESIAN_POINT ( 'NONE',  ( -2.517493886309087880, 214.5937144450984135, 3.098862081921434974 ) ) ;
#2805 = CARTESIAN_POINT ( 'NONE',  ( 74.41132485994282320, 167.7597621252805880, 9.270509831248428867 ) ) ;
#2806 = ORIENTED_EDGE ( 'NONE', *, *, #14161, .F. ) ;
#2807 = CARTESIAN_POINT ( 'NONE',  ( -6.500168698208244500, 211.6636982574061676, 92.79886208192142760 ) ) ;
#2808 = ADVANCED_FACE ( 'NONE', ( #9001 ), #25061, .T. ) ;
#2809 = CARTESIAN_POINT ( 'NONE',  ( 8.015496119326531499, 209.5516654185219636, 28.85113791807856032 ) ) ;
#2810 = FACE_BOUND ( 'NONE', #27161, .T. ) ;
#2811 = EDGE_LOOP ( 'NONE', ( #20272, #1188, #20856, #9872 ) ) ;
#2812 = DIRECTION ( 'NONE',  ( -1.000000000000000000, -0.000000000000000000, -0.000000000000000000 ) ) ;
#2813 = CARTESIAN_POINT ( 'NONE',  ( 33.47499999726881015, 160.0630714827496206, -15.58253175000000823 ) ) ;
#2814 = CYLINDRICAL_SURFACE ( 'NONE', #13238, 2.000000000000000888 ) ;
#2815 = CARTESIAN_POINT ( 'NONE',  ( 2.517493886308900919, 214.5937144450984420, 85.40113791807856103 ) ) ;
#2816 = DIRECTION ( 'NONE',  ( -1.000000000000000000, 0.000000000000000000, 0.000000000000000000 ) ) ;
#2817 = CARTESIAN_POINT ( 'NONE',  ( 49.00000000000000711, 170.2462022514548323, -7.872454543227099337E-15 ) ) ;
#2818 = CARTESIAN_POINT ( 'NONE',  ( -8.000000000000008882, 206.9523078486584780, 59.49886208192144466 ) ) ;
#2819 = CYLINDRICAL_SURFACE ( 'NONE', #22161, 5.249999999999991118 ) ;
#2820 = CARTESIAN_POINT ( 'NONE',  ( 51.62499999726880873, 171.3844434931184253, -7.942151717890132712E-15 ) ) ;
#2821 = CARTESIAN_POINT ( 'NONE',  ( 3.044812012440130555, 197.4746971517856764, 5.601137918078566535 ) ) ;
#2822 = AXIS2_PLACEMENT_3D ( 'NONE', #32750, #4651, #32925 ) ;
#2823 = CARTESIAN_POINT ( 'NONE',  ( 61.52499999726881441, 169.8198683612136222, -4.815267126137197984 ) ) ;
#2824 = CARTESIAN_POINT ( 'NONE',  ( 70.07499999726881867, 168.2552932293087906, 9.630534252274372875 ) ) ;
#2825 = CARTESIAN_POINT ( 'NONE',  ( 0.05014649552807549926, 219.6175466908591716, 70.25113791807856956 ) ) ;
#2826 = DIRECTION ( 'NONE',  ( 1.000000000000000000, 0.000000000000000000, 0.000000000000000000 ) ) ;
#2827 = CARTESIAN_POINT ( 'NONE',  ( 6.139770520408367460, 198.4640165459539389, 83.45113791807858661 ) ) ;
#2828 = CARTESIAN_POINT ( 'NONE',  ( 60.00000000000000000, 7.347880794884118356E-15, 20.00000000000000000 ) ) ;
#2829 = CARTESIAN_POINT ( 'NONE',  ( -11.98450388067341876, 203.0532714938636047, 56.34886208192143187 ) ) ;
#2830 = CARTESIAN_POINT ( 'NONE',  ( -9.984503880673420539, 203.7031108863293980, 56.34886208192142476 ) ) ;
#2831 = CARTESIAN_POINT ( 'NONE',  ( -0.05014649552807705357, 194.3824533091408000, 95.75113791807856956 ) ) ;
#2832 = FACE_OUTER_BOUND ( 'NONE', #25921, .T. ) ;
#2833 = CARTESIAN_POINT ( 'NONE',  ( 9.984503880673470277, 203.7031108863295401, 11.15113791807856636 ) ) ;
#2834 = CARTESIAN_POINT ( 'NONE',  ( 8.118202686958138514, 201.1607312380088501, 76.29886208192144181 ) ) ;
#2835 = EDGE_LOOP ( 'NONE', ( #7498, #12892, #504 ) ) ;
#2836 = CARTESIAN_POINT ( 'NONE',  ( 9.984503880673470277, 203.7031108863295401, 98.15113791807858945 ) ) ;
#2837 = ORIENTED_EDGE ( 'NONE', *, *, #12643, .F. ) ;
#2838 = CARTESIAN_POINT ( 'NONE',  ( 32.50000000000000000, 155.0000000000000000, -6.938893903907228378E-15 ) ) ;
#2839 = CARTESIAN_POINT ( 'NONE',  ( 7.984503880673422316, 209.6470497212048372, 57.84886208192144608 ) ) ;
#2840 = VERTEX_POINT ( 'NONE', #24677 ) ;
#2841 =( BOUNDED_SURFACE ( )  B_SPLINE_SURFACE ( 3, 2, ( 
 ( #25300, #4516, #14908 ),
 ( #22750, #20187, #13033 ),
 ( #10652, #89, #18481 ),
 ( #3297, #23425, #26144 ),
 ( #15749, #10488, #18641 ),
 ( #18976, #21523, #13681 ),
 ( #16248, #13193, #21191 ),
 ( #5688, #20867, #31749 ) ),
 .UNSPECIFIED., .F., .F., .T. ) 
 B_SPLINE_SURFACE_WITH_KNOTS ( ( 4, 2, 2, 4 ),
 ( 3, 3 ),
 ( 0.03861844051980969222, 0.04325213341840641185, 0.04556897986770477166, 0.04788582631700313147 ),
 ( 0.000000000000000000, 1.000000000000000000 ),
 .UNSPECIFIED. ) 
 GEOMETRIC_REPRESENTATION_ITEM ( )  RATIONAL_B_SPLINE_SURFACE ( (
 ( 1.000000000000000000, 0.8047781759831921233, 1.000000000000000000),
 ( 1.000000000000000000, 0.8123762462806503049, 1.000000000000000000),
 ( 1.000000000000000000, 0.8190659850614813164, 1.000000000000000000),
 ( 1.000000000000000000, 0.8191937571014595854, 1.000000000000000000),
 ( 1.000000000000000000, 0.8176092952779865364, 1.000000000000000000),
 ( 1.000000000000000000, 0.8122962088597069918, 1.000000000000000000),
 ( 1.000000000000000000, 0.8086311330827506971, 1.000000000000000000),
 ( 1.000000000000000000, 0.8047712282214323221, 1.000000000000000000) ) ) 
 REPRESENTATION_ITEM ( '' )  SURFACE ( )  );
#2842 = ADVANCED_FACE ( 'NONE', ( #10900 ), #13624, .T. ) ;
#2843 = CARTESIAN_POINT ( 'NONE',  ( 77.62499999726880162, 171.3844434931184253, -7.942151717890134290E-15 ) ) ;
#2844 = DIRECTION ( 'NONE',  ( 1.000000000000000000, 0.000000000000000000, 0.000000000000000000 ) ) ;
#2845 = CARTESIAN_POINT ( 'NONE',  ( -56.07926260655170836, 194.9951118559247050, 0.6454098859825110335 ) ) ;
#2846 = ADVANCED_FACE ( 'NONE', ( #16494 ), #1003, .F. ) ;
#2847 = UNCERTAINTY_MEASURE_WITH_UNIT (LENGTH_MEASURE( 1.000000000000000082E-05 ), #3926, 'distance_accuracy_value', 'NONE');
#2848 = CARTESIAN_POINT ( 'NONE',  ( 70.92499999726881299, 145.8408176439707802, -12.60653300113719588 ) ) ;
#2849 = CARTESIAN_POINT ( 'NONE',  ( -4.984841277089726574, 200.2242689037092305, 57.05113791807856671 ) ) ;
#2850 = DIRECTION ( 'NONE',  ( 1.000000000000000000, -0.000000000000000000, -0.000000000000000000 ) ) ;
#2851 = CARTESIAN_POINT ( 'NONE',  ( -8.118202686958138514, 212.8392687619910930, 47.79886208192143471 ) ) ;
#2852 = CARTESIAN_POINT ( 'NONE',  ( -9.297231092197758784, 206.2510696422452838, 104.2062683007240338 ) ) ;
#2853 = ADVANCED_FACE ( 'NONE', ( #21776 ), #30510, .T. ) ;
#2854 = DIRECTION ( 'NONE',  ( -0.5000000000000061062, 0.000000000000000000, 0.8660254037844351549 ) ) ;
#2855 = CARTESIAN_POINT ( 'NONE',  ( -6.444103211790928043, 202.2591342207265939, 35.19886208192144039 ) ) ;
#2856 = CARTESIAN_POINT ( 'NONE',  ( 0.05014649552810505201, 217.5146222423826714, 82.25113791807858377 ) ) ;
#2857 = CARTESIAN_POINT ( 'NONE',  ( 125.5000000000000000, 229.9533188057749555, 74.95331880577313655 ) ) ;
#2858 = CARTESIAN_POINT ( 'NONE',  ( 0.05014649552810505201, 217.5146222423826714, 58.25113791807856245 ) ) ;
#2859 = AXIS2_PLACEMENT_3D ( 'NONE', #24729, #21527, #1383 ) ;
#2860 = CARTESIAN_POINT ( 'NONE',  ( -3.135527875058821579, 197.5041725223112223, 23.90113791807856813 ) ) ;
#2861 = CARTESIAN_POINT ( 'NONE',  ( -6.500168698208129925, 202.3363017425936050, 15.20113791807857062 ) ) ;
#2862 = CARTESIAN_POINT ( 'NONE',  ( 46.58867513459481557, 146.1832212156128890, -12.13525491562423042 ) ) ;
#2863 = CARTESIAN_POINT ( 'NONE',  ( 72.99495483890930814, 155.0000000000000000, -15.50000000000001776 ) ) ;
#2864 = CARTESIAN_POINT ( 'NONE',  ( 38.42499999726880588, 141.7447067706911810, 9.630534252274376428 ) ) ;
#2865 = CARTESIAN_POINT ( 'NONE',  ( -9.680171189290831535, 214.0920067884431148, 42.80113791807857382 ) ) ;
#2866 = CARTESIAN_POINT ( 'NONE',  ( 60.00000000000000000, 7.347880794884118356E-15, 35.00000000000000000 ) ) ;
#2867 = CARTESIAN_POINT ( 'NONE',  ( -3.135527875058821579, 197.5041725223112223, 86.90113791807857524 ) ) ;
#2868 = CARTESIAN_POINT ( 'NONE',  ( 8.118202686958039038, 212.8392687619912635, 58.70113791807857240 ) ) ;
#2869 = CARTESIAN_POINT ( 'NONE',  ( 12.00000000000000711, 207.0476921513415220, 24.99886208192143400 ) ) ;
#2870 = CARTESIAN_POINT ( 'NONE',  ( -10.00000000000000711, 206.9523078486584495, 32.49886208192143044 ) ) ;
#2871 = CARTESIAN_POINT ( 'NONE',  ( 82.29999999453764303, 167.3344367211045096, -8.961492836873482304 ) ) ;
#2872 = AXIS2_PLACEMENT_3D ( 'NONE', #19834, #9787, #4333 ) ;
#2873 = CARTESIAN_POINT ( 'NONE',  ( -9.736236675707914401, 199.9851607334237542, 69.20113791807857240 ) ) ;
#2874 = CARTESIAN_POINT ( 'NONE',  ( -6.500168698208129925, 202.3363017425936050, 90.20113791807857240 ) ) ;
#2875 = EDGE_CURVE ( 'NONE', #27919, #25683, #11398, .T. ) ;
#2876 = AXIS2_PLACEMENT_3D ( 'NONE', #9612, #9277, #19670 ) ;
#2877 = CARTESIAN_POINT ( 'NONE',  ( -9.984503880673420539, 203.7031108863293980, 53.34886208192143897 ) ) ;
#2878 = DIRECTION ( 'NONE',  ( 1.000000000000000000, -0.000000000000000000, -0.000000000000000000 ) ) ;
#2879 = ORIENTED_EDGE ( 'NONE', *, *, #30577, .F. ) ;
#2880 = CARTESIAN_POINT ( 'NONE',  ( -0.05014649552828442242, 219.6175466908591716, 48.24886208192144466 ) ) ;
#2881 = VERTEX_POINT ( 'NONE', #19227 ) ;
#2882 = ORIENTED_EDGE ( 'NONE', *, *, #26989, .F. ) ;
#2883 = EDGE_CURVE ( 'NONE', #25547, #11897, #18841, .T. ) ;
#2884 = CARTESIAN_POINT ( 'NONE',  ( 125.0000000000000000, 4.592425496802574367E-14, -35.00000000000000000 ) ) ;
#2885 = CARTESIAN_POINT ( 'NONE',  ( -125.0000000000000000, 25.00000000000000000, 35.00000000000000000 ) ) ;
#2886 = CARTESIAN_POINT ( 'NONE',  ( 2.517493886308900919, 214.5937144450984420, 46.40113791807856813 ) ) ;
#2887 = CARTESIAN_POINT ( 'NONE',  ( 10.00000000000000711, 207.0476921513415220, 27.99886208192143755 ) ) ;
#2888 = CARTESIAN_POINT ( 'NONE',  ( 65.27499999726880731, 149.9369285172503510, -15.58253175000000823 ) ) ;
#2889 = ORIENTED_EDGE ( 'NONE', *, *, #31198, .F. ) ;
#2890 = DIRECTION ( 'NONE',  ( -6.106226635438360972E-16, 0.04769215134144213358, -0.9988620819214358848 ) ) ;
#2891 = TOROIDAL_SURFACE ( 'NONE', #19225, 69.99999999999998579, 27.99999999999999645 ) ;
#2892 = FACE_OUTER_BOUND ( 'NONE', #5791, .T. ) ;
#2893 = CARTESIAN_POINT ( 'NONE',  ( 8.015496119326595448, 204.4483345814782638, 1.148862081921434797 ) ) ;
#2894 = CIRCLE ( 'NONE', #17014, 40.00000000000000711 ) ;
#2895 = CARTESIAN_POINT ( 'NONE',  ( 10.00000000000000711, 206.9523078486586201, 56.00113791807856956 ) ) ;
#2896 = CARTESIAN_POINT ( 'NONE',  ( 32.50000000000000000, 155.0000000000000000, -6.938893903907228378E-15 ) ) ;
#2897 = EDGE_CURVE ( 'NONE', #615, #895, #20173, .T. ) ;
#2898 = CARTESIAN_POINT ( 'NONE',  ( 9.984503880673470277, 203.7031108863295401, 32.15113791807857524 ) ) ;
#2899 = FACE_OUTER_BOUND ( 'NONE', #26462, .T. ) ;
#2900 = AXIS2_PLACEMENT_3D ( 'NONE', #17674, #5401, #30974 ) ;
#2901 = APPLICATION_PROTOCOL_DEFINITION ( 'draft international standard', 'automotive_design', 1998, #8976 ) ;
#2902 = CARTESIAN_POINT ( 'NONE',  ( -0.05014649552828365914, 215.4116977939061144, 90.24886208192144466 ) ) ;
#2903 = CARTESIAN_POINT ( 'NONE',  ( 41.32499999726881157, 164.1591823560292198, -12.60653300113719766 ) ) ;
#2904 = DIRECTION ( 'NONE',  ( 0.000000000000000000, -0.5000000000000013323, -0.8660254037844379305 ) ) ;
#2905 = CARTESIAN_POINT ( 'NONE',  ( 18.00000000000000711, 2.204364238465236217E-15, -17.97459999999999525 ) ) ;
#2906 = CARTESIAN_POINT ( 'NONE',  ( 12.00000000000000711, 206.9523078486586485, 8.001137918078566003 ) ) ;
#2907 = LINE ( 'NONE', #21126, #5343 ) ;
#2908 = CARTESIAN_POINT ( 'NONE',  ( 55.57499999726881157, 164.1591823560292198, -12.60653300113719766 ) ) ;
#2909 = ADVANCED_FACE ( 'NONE', ( #3219 ), #15259, .F. ) ;
#2910 = CARTESIAN_POINT ( 'NONE',  ( -6.220909254589537696, 198.5229672870051161, 60.05113791807855961 ) ) ;
#2911 = CARTESIAN_POINT ( 'NONE',  ( 10.00000000000000711, 206.9523078486586201, 32.00113791807856956 ) ) ;
#2912 = CARTESIAN_POINT ( 'NONE',  ( 35.41132485994280898, 142.2402378747194405, -9.270509831248439525 ) ) ;
#2913 = VECTOR ( 'NONE', #28866, 1000.000000000000000 ) ;
#2914 = CARTESIAN_POINT ( 'NONE',  ( 115.4999999999999858, 51.09158283380784837, 28.95509836041906482 ) ) ;
#2915 = CARTESIAN_POINT ( 'NONE',  ( 64.50000000000000000, 0.000000000000000000, -30.00000000000000000 ) ) ;
#2916 = CARTESIAN_POINT ( 'NONE',  ( 58.29999999453762172, 167.3344367211045096, -8.961492836873482304 ) ) ;
#2917 = ORIENTED_EDGE ( 'NONE', *, *, #1, .T. ) ;
#2918 = CARTESIAN_POINT ( 'NONE',  ( 0.05014649552807549926, 219.6175466908591716, 43.25113791807856245 ) ) ;
#2919 = FACE_OUTER_BOUND ( 'NONE', #7301, .T. ) ;
#2920 = UNCERTAINTY_MEASURE_WITH_UNIT (LENGTH_MEASURE( 1.000000000000000082E-05 ), #133, 'distance_accuracy_value', 'NONE');
#2921 = CARTESIAN_POINT ( 'NONE',  ( -0.05014649552828403384, 217.5146222423826714, 21.24886208192143400 ) ) ;
#2922 =( REPRESENTATION_RELATIONSHIP ('NONE','NONE', #25663, #30243 ) REPRESENTATION_RELATIONSHIP_WITH_TRANSFORMATION ( #27903 )SHAPE_REPRESENTATION_RELATIONSHIP( ) );
#2923 = CARTESIAN_POINT ( 'NONE',  ( 59.11132485994280472, 140.7341522555726669, 4.635254915624211769 ) ) ;
#2924 = ORIENTED_EDGE ( 'NONE', *, *, #13743, .T. ) ;
#2925 = CARTESIAN_POINT ( 'NONE',  ( -0.05014649552810635652, 196.4853777576173002, 71.75113791807858377 ) ) ;
#2926 = AXIS2_PLACEMENT_3D ( 'NONE', #28536, #33639, #10810 ) ;
#2927 = VERTEX_POINT ( 'NONE', #4733 ) ;
#2928 = AXIS2_PLACEMENT_3D ( 'NONE', #11132, #27792, #4457 ) ;
#2929 = DIRECTION ( 'NONE',  ( -0.9891821073486152249, -0.1466927349985424900, -2.962715634069391535E-17 ) ) ;
#2930 = CARTESIAN_POINT ( 'NONE',  ( 64.50000000000000000, 0.000000000000000000, -30.00000000000000000 ) ) ;
#2931 = ORIENTED_EDGE ( 'NONE', *, *, #25842, .T. ) ;
#2932 = CARTESIAN_POINT ( 'NONE',  ( 2.517493886308900919, 214.5937144450984420, 13.40113791807856636 ) ) ;
#2933 = CARTESIAN_POINT ( 'NONE',  ( 9.736236675708031640, 199.9851607334238963, 100.2988620819214276 ) ) ;
#2934 = CARTESIAN_POINT ( 'NONE',  ( 45.67499999726881299, 168.2552932293087906, -9.630534252274387086 ) ) ;
#2935 = ORIENTED_EDGE ( 'NONE', *, *, #16237, .F. ) ;
#2936 = CARTESIAN_POINT ( 'NONE',  ( 50.32499999726881157, 145.8408176439707802, 12.60653300113718345 ) ) ;
#2937 = DIRECTION ( 'NONE',  ( -0.000000000000000000, -0.000000000000000000, -1.000000000000000000 ) ) ;
#2938 = CARTESIAN_POINT ( 'NONE',  ( -0.05014649552810635652, 196.4853777576173002, 8.751137918078562450 ) ) ;
#2939 = COLOUR_RGB ( '', 0.66274510, 0.83137255, 0.94901961) ;
#2940 = CARTESIAN_POINT ( 'NONE',  ( -6.220909254589682469, 215.4770327129946850, 80.94886208192143329 ) ) ;
#2941 = CARTESIAN_POINT ( 'NONE',  ( 51.57499999726881157, 164.1591823560292198, -12.60653300113719766 ) ) ;
#2942 = DIRECTION ( 'NONE',  ( -0.1045284632676468234, 0.000000000000000000, 0.9945218953682740670 ) ) ;
#2943 = CARTESIAN_POINT ( 'NONE',  ( -3.135527875058821579, 197.5041725223112223, 8.901137918078566358 ) ) ;
#2944 = CARTESIAN_POINT ( 'NONE',  ( 44.48867513459482126, 142.2402378747194405, -9.270509831248439525 ) ) ;
#2945 = EDGE_CURVE ( 'NONE', #21593, #29444, #28334, .T. ) ;
#2946 = EDGE_CURVE ( 'NONE', #18729, #27759, #24526, .T. ) ;
#2947 = CIRCLE ( 'NONE', #10031, 3.299999999999999822 ) ;
#2948 = CARTESIAN_POINT ( 'NONE',  ( 72.39999999999999147, 150.2886644046228639, -14.50000000000000888 ) ) ;
#2949 = CARTESIAN_POINT ( 'NONE',  ( 9.984503880673470277, 203.7031108863295401, 95.15113791807854682 ) ) ;
#2950 = DIRECTION ( 'NONE',  ( 0.000000000000000000, -0.000000000000000000, 1.000000000000000000 ) ) ;
#2951 = CARTESIAN_POINT ( 'NONE',  ( -6.220909254589537696, 198.5229672870051161, 84.05113791807855250 ) ) ;
#2952 = CARTESIAN_POINT ( 'NONE',  ( 86.58867513459482268, 146.1832212156128890, -12.13525491562423042 ) ) ;
#2953 = CIRCLE ( 'NONE', #13273, 2.149999999999999023 ) ;
#2954 = CARTESIAN_POINT ( 'NONE',  ( 35.47499999726880304, 160.0630714827496206, -15.58253175000000823 ) ) ;
#2955 = EDGE_CURVE ( 'NONE', #30489, #15562, #3291, .T. ) ;
#2956 = CARTESIAN_POINT ( 'NONE',  ( 0.05014649552828288198, 194.3824533091408000, 97.74886208192141623 ) ) ;
#2957 = CARTESIAN_POINT ( 'NONE',  ( 70.72499999726881015, 140.1801316387863778, -4.815267126137194431 ) ) ;
#2958 = EDGE_LOOP ( 'NONE', ( #10194, #3130, #13798 ) ) ;
#2959 = DIRECTION ( 'NONE',  ( -0.000000000000000000, 0.000000000000000000, -1.000000000000000000 ) ) ;
#2960 = CARTESIAN_POINT ( 'NONE',  ( 43.99999999453763166, 155.0000000000000000, -14.50000000000000711 ) ) ;
#2961 = CARTESIAN_POINT ( 'NONE',  ( 11.98450388067341876, 210.9467285061363953, 3.848862081921433642 ) ) ;
#2962 = CARTESIAN_POINT ( 'NONE',  ( 97.30927364589244632, 155.0000000000000000, 0.000000000000000000 ) ) ;
#2963 = ORIENTED_EDGE ( 'NONE', *, *, #18143, .F. ) ;
#2964 = COLOUR_RGB ( '', 0.08235294, 0.09019608, 0.10196078) ;
#2965 = CARTESIAN_POINT ( 'NONE',  ( -6.220909254589682469, 215.4770327129947134, 92.94886208192143329 ) ) ;
#2966 = CARTESIAN_POINT ( 'NONE',  ( 0.05014649552828288198, 194.3824533091408000, 31.74886208192143755 ) ) ;
#2967 = CARTESIAN_POINT ( 'NONE',  ( 0.3999999999999975797, 0.000000000000000000, 6.500000000000000000 ) ) ;
#2968 = CARTESIAN_POINT ( 'NONE',  ( 3.044812012440130555, 197.4746971517856764, 41.60113791807857808 ) ) ;
#2969 = VERTEX_POINT ( 'NONE', #25344 ) ;
#2970 = CARTESIAN_POINT ( 'NONE',  ( 4.984841277089891776, 200.2242689037093726, 4.448862081921435063 ) ) ;
#2971 = DIRECTION ( 'NONE',  ( 1.000000000000000000, 0.000000000000000000, 0.000000000000000000 ) ) ;
#2972 = VECTOR ( 'NONE', #3685, 1000.000000000000000 ) ;
#2973 = ORIENTED_EDGE ( 'NONE', *, *, #2722, .T. ) ;
#2974 = CARTESIAN_POINT ( 'NONE',  ( 4.984841277089891776, 200.2242689037093726, 94.44886208192143329 ) ) ;
#2975 = CARTESIAN_POINT ( 'NONE',  ( 8.000000000000008882, 206.9523078486586485, 32.00113791807856956 ) ) ;
#2976 = DIRECTION ( 'NONE',  ( -1.000000000000000000, 0.000000000000000000, 0.000000000000000000 ) ) ;
#2977 = EDGE_LOOP ( 'NONE', ( #23465, #13032, #17791, #8041 ) ) ;
#2978 = CARTESIAN_POINT ( 'NONE',  ( 33.82499999726880446, 168.2552932293087906, 9.630534252274372875 ) ) ;
#2979 = CARTESIAN_POINT ( 'NONE',  ( 35.87499999726881583, 171.3844434931184253, -7.942151717890132712E-15 ) ) ;
#2980 = CARTESIAN_POINT ( 'NONE',  ( 5.000000000000001776, 6.123233995736768255E-16, -9.974600000000000577 ) ) ;
#2981 = CARTESIAN_POINT ( 'NONE',  ( -4.903702542908602524, 213.8346818373418898, 87.95113791807857240 ) ) ;
#2982 = CARTESIAN_POINT ( 'NONE',  ( 45.90000000000000568, 141.2096805137202580, 4.480746418436733158 ) ) ;
#2983 = CARTESIAN_POINT ( 'NONE',  ( 2.426778023690075337, 214.6231898156240447, 63.39886208192144323 ) ) ;
#2984 = CARTESIAN_POINT ( 'NONE',  ( 84.61132485994284025, 159.8737954434934920, 15.00000000000010836 ) ) ;
#2985 = CARTESIAN_POINT ( 'NONE',  ( 49.82499999726881157, 168.2552932293087906, 9.630534252274372875 ) ) ;
#2986 = CARTESIAN_POINT ( 'NONE',  ( -3.135527875058821579, 197.5041725223112223, 8.901137918078566358 ) ) ;
#2987 = CARTESIAN_POINT ( 'NONE',  ( -63.49999999999884892, 215.0000000000000000, 2.500000000000000000 ) ) ;
#2988 = CARTESIAN_POINT ( 'NONE',  ( 63.42499999726880588, 168.2552932293087906, -9.630534252274387086 ) ) ;
#2989 = CARTESIAN_POINT ( 'NONE',  ( 74.87499999726880162, 138.6155565068815463, -3.929120461958505118E-15 ) ) ;
#2990 = CARTESIAN_POINT ( 'NONE',  ( -3.662846001190052991, 218.4274158808045740, 76.10113791807854966 ) ) ;
#2991 = PLANE ( 'NONE',  #32035 ) ;
#2992 = B_SPLINE_CURVE_WITH_KNOTS ( 'NONE', 3,
 ( #1353, #30143, #6800, #11575, #1179, #29974 ),
 .UNSPECIFIED., .F., .F.,
 ( 4, 2, 4 ),
 ( 0.002044882221487580483, 0.003063384235218526239, 0.004081886248949471996 ),
 .UNSPECIFIED. ) ;
#2993 = CARTESIAN_POINT ( 'NONE',  ( 9.984503880673473830, 203.7031108863295401, 86.15113791807857524 ) ) ;
#2994 = CARTESIAN_POINT ( 'NONE',  ( 54.28867513459483973, 139.2280666364260071, -4.041636747397287284E-15 ) ) ;
#2995 = ORIENTED_EDGE ( 'NONE', *, *, #16665, .F. ) ;
#2996 = CARTESIAN_POINT ( 'NONE',  ( -3.662846001189865142, 195.5725841191952838, 55.89886208192143613 ) ) ;
#2997 = CARTESIAN_POINT ( 'NONE',  ( 8.118202686958138514, 201.1607312380088501, 64.29886208192144181 ) ) ;
#2998 = CARTESIAN_POINT ( 'NONE',  ( 11.98450388067348271, 203.0532714938637753, 95.15113791807856103 ) ) ;
#2999 = CARTESIAN_POINT ( 'NONE',  ( 34.38867513459481273, 140.7341522555726669, -4.635254915624220651 ) ) ;
#3000 = CARTESIAN_POINT ( 'NONE',  ( -8.118202686958039038, 201.1607312380087080, 15.20113791807856884 ) ) ;
#3001 = CARTESIAN_POINT ( 'NONE',  ( -0.05014649552828403384, 217.5146222423826714, 81.24886208192140202 ) ) ;
#3002 = ORIENTED_EDGE ( 'NONE', *, *, #15223, .F. ) ;
#3003 = CARTESIAN_POINT ( 'NONE',  ( -6.220909254589537696, 198.5229672870051161, 96.05113791807858092 ) ) ;
#3004 = EDGE_LOOP ( 'NONE', ( #12042, #25746, #10651, #21637 ) ) ;
#3005 = DIRECTION ( 'NONE',  ( 1.000000000000000000, 0.000000000000000000, 0.000000000000000000 ) ) ;
#3006 = CARTESIAN_POINT ( 'NONE',  ( 2.426778023690075337, 214.6231898156240447, 66.39886208192143613 ) ) ;
#3007 = ORIENTED_EDGE ( 'NONE', *, *, #21235, .T. ) ;
#3008 = PRODUCT_DEFINITION_SHAPE ( 'NONE', 'NONE',  #33713 ) ;
#3009 = CARTESIAN_POINT ( 'NONE',  ( 80.02499999726880731, 160.0630714827496206, 15.58253174999999224 ) ) ;
#3010 = DIRECTION ( 'NONE',  ( -1.000000000000000000, -0.000000000000000000, -0.000000000000000000 ) ) ;
#3011 = CARTESIAN_POINT ( 'NONE',  ( 66.92499999726881299, 145.8408176439707802, -12.60653300113719588 ) ) ;
#3012 = CARTESIAN_POINT ( 'NONE',  ( 0.05014649552807626948, 215.4116977939061144, 58.25113791807857666 ) ) ;
#3013 = DIRECTION ( 'NONE',  ( 0.000000000000000000, -1.000000000000000000, 0.000000000000000000 ) ) ;
#3014 = DIRECTION ( 'NONE',  ( -0.000000000000000000, -0.000000000000000000, -1.000000000000000000 ) ) ;
#3015 = FACE_OUTER_BOUND ( 'NONE', #1776, .T. ) ;
#3016 = CARTESIAN_POINT ( 'NONE',  ( 6.500168698208244500, 202.3363017425938324, 37.29886208192144181 ) ) ;
#3017 = CARTESIAN_POINT ( 'NONE',  ( -9.984503880673473830, 210.2968891136704315, 78.65113791807854682 ) ) ;
#3018 = DIRECTION ( 'NONE',  ( 0.000000000000000000, 0.000000000000000000, -1.000000000000000000 ) ) ;
#3019 = CARTESIAN_POINT ( 'NONE',  ( -3.044812012440131443, 216.5253028482142952, 67.10113791807857808 ) ) ;
#3020 = CARTESIAN_POINT ( 'NONE',  ( -10.01549611932653860, 203.7984951890123284, 30.35113791807856742 ) ) ;
#3021 = CARTESIAN_POINT ( 'NONE',  ( 4.984841277089725686, 213.7757310962907411, 10.55113791807856671 ) ) ;
#3022 = CARTESIAN_POINT ( 'NONE',  ( 46.68867513459483121, 150.1262045565065364, -15.00000000000012434 ) ) ;
#3023 = DIRECTION ( 'NONE',  ( 5.620504062164857944E-16, -0.9988620819214347746, 0.04769215134146256169 ) ) ;
#3024 = CARTESIAN_POINT ( 'NONE',  ( 47.12499999726880873, 155.0000000000000000, -15.58253175000000823 ) ) ;
#3025 = CARTESIAN_POINT ( 'NONE',  ( 3.662846001190051659, 195.5725841191953691, 41.60113791807857098 ) ) ;
#3026 = DIRECTION ( 'NONE',  ( 1.000000000000000000, 0.000000000000000000, 0.000000000000000000 ) ) ;
#3027 = CARTESIAN_POINT ( 'NONE',  ( 10.00000000000000711, 206.9523078486586201, 92.00113791807858377 ) ) ;
#3028 = ADVANCED_FACE ( 'NONE', ( #2013 ), #6784, .F. ) ;
#3029 = CARTESIAN_POINT ( 'NONE',  ( 6.220909254589536808, 215.4770327129947987, 61.55113791807857382 ) ) ;
#3030 = CARTESIAN_POINT ( 'NONE',  ( 12.00000000000000711, 207.0476921513415220, 21.99886208192143400 ) ) ;
#3031 = CARTESIAN_POINT ( 'NONE',  ( -8.062137200540822946, 201.0835637161416400, 41.19886208192144039 ) ) ;
#3032 = CARTESIAN_POINT ( 'NONE',  ( 80.29999999453761461, 167.3344367211045096, -8.961492836873482304 ) ) ;
#3033 = CARTESIAN_POINT ( 'NONE',  ( 7.375838497908181246, 196.7627149292499666, 68.45113791807857240 ) ) ;
#3034 = CARTESIAN_POINT ( 'NONE',  ( 4.984841277089725686, 213.7757310962907411, 91.55113791807858092 ) ) ;
#3035 =( BOUNDED_CURVE ( )  B_SPLINE_CURVE ( 3, ( #15301, #5081, #30646, #23476 ),
 .UNSPECIFIED., .F., .T. ) 
 B_SPLINE_CURVE_WITH_KNOTS ( ( 4, 4 ),
 ( 5.758306373677911871, 6.283185307179586232 ),
 .UNSPECIFIED. ) 
 CURVE ( )  GEOMETRIC_REPRESENTATION_ITEM ( )  RATIONAL_B_SPLINE_CURVE ( ( 1.000000000000000000, 0.9771733092046011038, 0.9771733092046011038, 1.000000000000000000 ) ) 
 REPRESENTATION_ITEM ( '' )  );
#3036 = CARTESIAN_POINT ( 'NONE',  ( 10.00000000000000711, 207.0476921513415220, 54.99886208192143755 ) ) ;
#3037 = CARTESIAN_POINT ( 'NONE',  ( 49.78867513459482552, 155.0000000000000000, 15.00000000000001243 ) ) ;
#3038 = ORIENTED_EDGE ( 'NONE', *, *, #2261, .F. ) ;
#3039 = CARTESIAN_POINT ( 'NONE',  ( 7.456977232089471386, 196.8216656703012006, 55.44886208192143329 ) ) ;
#3040 = ORIENTED_EDGE ( 'NONE', *, *, #16988, .T. ) ;
#3041 = B_SPLINE_CURVE_WITH_KNOTS ( 'NONE', 3,
 ( #12955, #2742, #28293, #28951, #17899, #13279, #23175, #26223, #23671, #331 ),
 .UNSPECIFIED., .F., .F.,
 ( 4, 2, 2, 2, 4 ),
 ( 0.000000000000000000, 0.002305503304226489900, 0.004611006608452982401, 0.006916509912679474036, 0.009222013216905966537 ),
 .UNSPECIFIED. ) ;
#3042 = ORIENTED_EDGE ( 'NONE', *, *, #9485, .F. ) ;
#3043 = CARTESIAN_POINT ( 'NONE',  ( 74.37499999726881583, 155.0000000000000000, 15.58253174999999402 ) ) ;
#3044 = CARTESIAN_POINT ( 'NONE',  ( 87.44295828238632851, 168.4482970619196465, 7.151417191984575261 ) ) ;
#3045 = CARTESIAN_POINT ( 'NONE',  ( 58.88867513459481984, 159.8737954434936057, -15.00000000000002665 ) ) ;
#3046 = CARTESIAN_POINT ( 'NONE',  ( -8.015496119326531499, 204.4483345814780364, 39.35113791807857098 ) ) ;
#3047 = CARTESIAN_POINT ( 'NONE',  ( -6.139770520408224463, 198.4640165459539389, 20.04886208192142760 ) ) ;
#3048 = CARTESIAN_POINT ( 'NONE',  ( 65.77499999726880731, 169.8198683612136222, -4.815267126137197984 ) ) ;
#3049 = EDGE_LOOP ( 'NONE', ( #9531, #9267, #20394 ) ) ;
#3050 = CARTESIAN_POINT ( 'NONE',  ( 32.50000000000000000, 155.0000000000000000, -15.00000000000002487 ) ) ;
#3051 = DIRECTION ( 'NONE',  ( 0.000000000000000000, 1.000000000000000000, -1.295896757998781572E-15 ) ) ;
#3052 = CARTESIAN_POINT ( 'NONE',  ( 8.015496119326595448, 204.4483345814782638, 7.148862081921435241 ) ) ;
#3053 = EDGE_CURVE ( 'NONE', #17895, #28642, #26860, .T. ) ;
#3054 = CARTESIAN_POINT ( 'NONE',  ( 3.135527875058820690, 216.4958274776887492, 49.40113791807857524 ) ) ;
#3055 = CARTESIAN_POINT ( 'NONE',  ( 80.41132485994282320, 167.7597621252805880, 9.270509831248428867 ) ) ;
#3056 = CARTESIAN_POINT ( 'NONE',  ( 3.135527875058820690, 216.4958274776887492, 25.40113791807856813 ) ) ;
#3057 = CARTESIAN_POINT ( 'NONE',  ( 86.87499999726880162, 138.6155565068815463, -3.929120461958505118E-15 ) ) ;
#3058 = PRODUCT_CONTEXT ( 'NONE', #7246, 'mechanical' ) ;
#3059 = CARTESIAN_POINT ( 'NONE',  ( 2.517493886309087436, 199.4062855549015865, 94.59886208192145318 ) ) ;
#3060 = CARTESIAN_POINT ( 'NONE',  ( 37.52499999726881441, 169.8198683612136222, -4.815267126137197984 ) ) ;
#3061 = CARTESIAN_POINT ( 'NONE',  ( 81.08867513459485110, 167.7597621252805880, -9.270509831248443078 ) ) ;
#3062 = DIRECTION ( 'NONE',  ( 5.170793409489829447E-18, -0.9988620819214357738, 0.04769215134144141888 ) ) ;
#3063 = CARTESIAN_POINT ( 'NONE',  ( -9.736236675707914401, 199.9851607334237542, 9.201137918078563516 ) ) ;
#3064 = DIRECTION ( 'NONE',  ( 1.000000000000000000, 0.000000000000000000, 0.000000000000000000 ) ) ;
#3065 = CARTESIAN_POINT ( 'NONE',  ( 58.67499999726882010, 141.7447067706911810, 9.630534252274376428 ) ) ;
#3066 = CARTESIAN_POINT ( 'NONE',  ( 8.118202686958039038, 212.8392687619912635, 58.70113791807857240 ) ) ;
#3067 = ADVANCED_FACE ( 'NONE', ( #32501 ), #2258, .T. ) ;
#3068 = CARTESIAN_POINT ( 'NONE',  ( 3.135527875058820690, 216.4958274776887492, 28.40113791807856813 ) ) ;
#3069 = CONICAL_SURFACE ( 'NONE', #17218, 37.00000000000000711, 0.7853981633974482790 ) ;
#3070 = LINE ( 'NONE', #13792, #17568 ) ;
#3071 = AXIS2_PLACEMENT_3D ( 'NONE', #32779, #32953, #27674 ) ;
#3072 = CARTESIAN_POINT ( 'NONE',  ( -64.50000000000000000, -95.00000000000000000, -20.00000000000000000 ) ) ;
#3073 = CARTESIAN_POINT ( 'NONE',  ( 65.71132485994280614, 155.0000000000000000, -15.00000000000002487 ) ) ;
#3074 = CARTESIAN_POINT ( 'NONE',  ( 59.59999999453763309, 141.2096805137202580, -4.480746418436742040 ) ) ;
#3075 = ORIENTED_EDGE ( 'NONE', *, *, #3497, .T. ) ;
#3076 = CARTESIAN_POINT ( 'NONE',  ( 3.662846001190051659, 195.5725841191953691, 35.60113791807855677 ) ) ;
#3077 = LINE ( 'NONE', #13465, #20258 ) ;
#3078 = CARTESIAN_POINT ( 'NONE',  ( -9.984503880673420539, 203.7031108863293980, 20.34886208192143187 ) ) ;
#3079 = CARTESIAN_POINT ( 'NONE',  ( 71.81132485994281467, 159.8737954434934920, -15.00000000000012434 ) ) ;
#3080 = AXIS2_PLACEMENT_3D ( 'NONE', #20994, #31391, #8061 ) ;
#3081 = EDGE_LOOP ( 'NONE', ( #11713, #8377, #3706, #13143 ) ) ;
#3082 = EDGE_CURVE ( 'NONE', #10769, #27181, #18017, .T. ) ;
#3083 = CARTESIAN_POINT ( 'NONE',  ( 6.139770520408368348, 198.4640165459539674, 80.45113791807857240 ) ) ;
#3084 = EDGE_LOOP ( 'NONE', ( #29396, #6006, #4591, #24966, #16927, #3331, #5268 ) ) ;
#3085 = CARTESIAN_POINT ( 'NONE',  ( 0.000000000000000000, 0.000000000000000000, -7.974599999999998801 ) ) ;
#3086 = CARTESIAN_POINT ( 'NONE',  ( 43.91132485994281609, 163.8167787843871110, -12.13525491562423397 ) ) ;
#3087 = ORIENTED_EDGE ( 'NONE', *, *, #23945, .F. ) ;
#3088 = CARTESIAN_POINT ( 'NONE',  ( -6.444103211791042618, 211.7408657792732356, 12.80113791807856849 ) ) ;
#3089 = EDGE_CURVE ( 'NONE', #29773, #2221, #25646, .T. ) ;
#3090 = CARTESIAN_POINT ( 'NONE',  ( -3.662846001189865142, 195.5725841191952838, 94.89886208192145034 ) ) ;
#3091 = CARTESIAN_POINT ( 'NONE',  ( 46.67499999726881299, 141.7447067706911810, 9.630534252274376428 ) ) ;
#3092 = VERTEX_POINT ( 'NONE', #17508 ) ;
#3093 = CARTESIAN_POINT ( 'NONE',  ( 48.42499999726881299, 141.7447067706911810, 9.630534252274376428 ) ) ;
#3094 = DIRECTION ( 'NONE',  ( 0.000000000000000000, 0.000000000000000000, 1.000000000000000000 ) ) ;
#3095 = CARTESIAN_POINT ( 'NONE',  ( 61.78867513459482552, 155.0000000000000000, 15.00000000000001243 ) ) ;
#3096 = TOROIDAL_SURFACE ( 'NONE', #2574, 2.200000000000001066, 0.2000000000000000111 ) ;
#3097 = CARTESIAN_POINT ( 'NONE',  ( 3.044812012439969795, 216.5253028482143520, 84.39886208192143613 ) ) ;
#3098 = ADVANCED_FACE ( 'NONE', ( #30466 ), #7305, .T. ) ;
#3099 = CARTESIAN_POINT ( 'NONE',  ( 53.97499999726881015, 169.8198683612136222, 4.815267126137181997 ) ) ;
#3100 = CARTESIAN_POINT ( 'NONE',  ( -3.135527875058821579, 197.5041725223112223, 20.90113791807856813 ) ) ;
#3101 = CARTESIAN_POINT ( 'NONE',  ( 81.71132485994280614, 155.0000000000000000, -15.00000000000002487 ) ) ;
#3102 = TOROIDAL_SURFACE ( 'NONE', #23771, 8.331345277524542681, 0.6186547224754559426 ) ;
#3103 = CARTESIAN_POINT ( 'NONE',  ( 76.30000000000001137, 146.4771138417591203, -11.73074641843674470 ) ) ;
#3104 = CARTESIAN_POINT ( 'NONE',  ( 40.38867513459481984, 140.7341522555726669, -4.635254915624220651 ) ) ;
#3105 = CARTESIAN_POINT ( 'NONE',  ( 32.50000000000000000, 155.0000000000000000, -6.938893903907228378E-15 ) ) ;
#3106 = CARTESIAN_POINT ( 'NONE',  ( -6.139770520408369237, 215.5359834540460042, 84.95113791807858661 ) ) ;
#3107 = CARTESIAN_POINT ( 'NONE',  ( 86.38867513459483405, 140.7341522555726669, -4.635254915624220651 ) ) ;
#3108 = CARTESIAN_POINT ( 'NONE',  ( 41.07499999726881157, 141.7447067706911810, -9.630534252274385310 ) ) ;
#3109 = CARTESIAN_POINT ( 'NONE',  ( -7.456977232089471386, 217.1783343296987709, 95.94886208192144750 ) ) ;
#3110 = CARTESIAN_POINT ( 'NONE',  ( 80.02499999726882152, 160.0630714827496206, 15.58253174999999402 ) ) ;
#3111 = ORIENTED_EDGE ( 'NONE', *, *, #30533, .F. ) ;
#3112 = DIRECTION ( 'NONE',  ( 1.000000000000000000, 0.000000000000000000, 0.000000000000000000 ) ) ;
#3113 = CARTESIAN_POINT ( 'NONE',  ( 39.19999999453763451, 146.4771138417591203, 11.73074641843673227 ) ) ;
#3114 = AXIS2_PLACEMENT_3D ( 'NONE', #16595, #21713, #11668 ) ;
#3115 = CARTESIAN_POINT ( 'NONE',  ( 1.750000000000014211, 3.031088913245526317, -2.899999999999999911 ) ) ;
#3116 =( GEOMETRIC_REPRESENTATION_CONTEXT ( 3 ) GLOBAL_UNCERTAINTY_ASSIGNED_CONTEXT ( ( #127 ) ) GLOBAL_UNIT_ASSIGNED_CONTEXT ( ( #13064, #26667, #19009 ) ) REPRESENTATION_CONTEXT ( 'NONE', 'WORKASPACE' ) );
#3117 = LINE ( 'NONE', #30021, #19378 ) ;
#3118 = ORIENTED_EDGE ( 'NONE', *, *, #17655, .F. ) ;
#3119 = CIRCLE ( 'NONE', #22153, 15.00000000000001776 ) ;
#3120 = CARTESIAN_POINT ( 'NONE',  ( 6.220909254589680693, 198.5229672870052582, 94.44886208192141908 ) ) ;
#3121 = CARTESIAN_POINT ( 'NONE',  ( -7.456977232089471386, 217.1783343296987709, 35.94886208192142618 ) ) ;
#3122 = CARTESIAN_POINT ( 'NONE',  ( 32.50000000000000000, 155.0000000000000000, -6.938893903907228378E-15 ) ) ;
#3123 = CARTESIAN_POINT ( 'NONE',  ( 10.01549611932653860, 210.2015048109876716, 37.85113791807854966 ) ) ;
#3124 = ORIENTED_EDGE ( 'NONE', *, *, #17926, .F. ) ;
#3125 = CARTESIAN_POINT ( 'NONE',  ( 7.984503880673422316, 209.6470497212048372, 6.848862081921435419 ) ) ;
#3126 = EDGE_CURVE ( 'NONE', #11257, #1148, #10416, .T. ) ;
#3127 = EDGE_CURVE ( 'NONE', #31781, #25951, #1668, .T. ) ;
#3128 = AXIS2_PLACEMENT_3D ( 'NONE', #20706, #25988, #29042 ) ;
#3129 = LINE ( 'NONE', #21346, #19229 ) ;
#3130 = ORIENTED_EDGE ( 'NONE', *, *, #21594, .F. ) ;
#3131 = CARTESIAN_POINT ( 'NONE',  ( -2.426778023690076225, 199.3768101843759553, 94.89886208192145034 ) ) ;
#3132 = PRODUCT_DEFINITION ( 'UNKNOWN', '', #13711, #29523 ) ;
#3133 = EDGE_CURVE ( 'NONE', #22909, #30882, #1841, .T. ) ;
#3134 = CARTESIAN_POINT ( 'NONE',  ( 6.500168698208129925, 211.6636982574063381, 28.70113791807857240 ) ) ;
#3135 = DIRECTION ( 'NONE',  ( -0.000000000000000000, -0.000000000000000000, -1.000000000000000000 ) ) ;
#3136 = VERTEX_POINT ( 'NONE', #33006 ) ;
#3137 = CARTESIAN_POINT ( 'NONE',  ( -52.50000000000002132, 155.0000000000000000, -16.99999999999999645 ) ) ;
#3138 = VECTOR ( 'NONE', #1838, 1000.000000000000000 ) ;
#3139 = EDGE_CURVE ( 'NONE', #24872, #5170, #30289, .T. ) ;
#3140 = CARTESIAN_POINT ( 'NONE',  ( 33.57499999726881157, 164.1591823560292198, -12.60653300113719766 ) ) ;
#3141 = FACE_OUTER_BOUND ( 'NONE', #18059, .T. ) ;
#3142 = CARTESIAN_POINT ( 'NONE',  ( 7.984503880673485376, 204.3529502787953902, 101.1511379180785895 ) ) ;
#3143 = CARTESIAN_POINT ( 'NONE',  ( 52.50000000000000711, 155.0000000000000000, -14.50000000000000711 ) ) ;
#3144 = CARTESIAN_POINT ( 'NONE',  ( -8.015496119326597224, 209.5516654185217362, 74.64886208192143613 ) ) ;
#3145 = DIRECTION ( 'NONE',  ( 1.000000000000000000, 0.000000000000000000, 0.000000000000000000 ) ) ;
#3146 = VECTOR ( 'NONE', #32555, 1000.000000000000000 ) ;
#3147 = CARTESIAN_POINT ( 'NONE',  ( 52.62499999726880162, 138.6155565068815463, -3.929120461958505118E-15 ) ) ;
#3149 = EDGE_LOOP ( 'NONE', ( #21685, #21772, #23410, #22654 ) ) ;
#3148 = CARTESIAN_POINT ( 'NONE',  ( -8.062137200540920645, 212.9164362838581894, 9.801137918078566713 ) ) ;
#3150 = DIRECTION ( 'NONE',  ( 1.000000000000000000, -0.000000000000000000, -0.000000000000000000 ) ) ;
#3151 = CARTESIAN_POINT ( 'NONE',  ( 65.52499999726880731, 169.8198683612136222, -4.815267126137197984 ) ) ;
#3152 = CARTESIAN_POINT ( 'NONE',  ( 75.57499999726881867, 164.1591823560292198, -12.60653300113719766 ) ) ;
#3153 = CARTESIAN_POINT ( 'NONE',  ( -7.456977232089304408, 196.8216656703010301, 78.05113791807858092 ) ) ;
#3154 = DIRECTION ( 'NONE',  ( 1.000000000000000000, -0.000000000000000000, -0.000000000000000000 ) ) ;
#3155 = CARTESIAN_POINT ( 'NONE',  ( -10.00000000000000711, 207.0476921513413515, 99.50113791807856956 ) ) ;
#3156 = CARTESIAN_POINT ( 'NONE',  ( 83.78867513459482552, 155.0000000000000000, 15.00000000000001243 ) ) ;
#3157 = VERTEX_POINT ( 'NONE', #27733 ) ;
#3158 = CARTESIAN_POINT ( 'NONE',  ( -0.05014649552828442242, 219.6175466908591716, 66.24886208192143044 ) ) ;
#3159 = CARTESIAN_POINT ( 'NONE',  ( -8.118202686958138514, 212.8392687619910930, 68.79886208192144181 ) ) ;
#3160 = CARTESIAN_POINT ( 'NONE',  ( 0.05014649552828288198, 194.3824533091408000, 4.748862081921433109 ) ) ;
#3161 = CARTESIAN_POINT ( 'NONE',  ( -67.50001199999999812, 157.2252672838932597, -16.89041650604970357 ) ) ;
#3162 = AXIS2_PLACEMENT_3D ( 'NONE', #6462, #4579, #19574 ) ;
#3163 = CARTESIAN_POINT ( 'NONE',  ( 3.044812012440130555, 197.4746971517856764, 17.60113791807856742 ) ) ;
#3164 = CARTESIAN_POINT ( 'NONE',  ( -3.044812012439970683, 197.4746971517856196, 82.89886208192145034 ) ) ;
#3165 = CIRCLE ( 'NONE', #23308, 2.500000000000000000 ) ;
#3166 = ORIENTED_EDGE ( 'NONE', *, *, #26579, .T. ) ;
#3167 = CARTESIAN_POINT ( 'NONE',  ( -3.135527875058821579, 197.5041725223112223, 101.9011379180785752 ) ) ;
#3168 = VERTEX_POINT ( 'NONE', #4394 ) ;
#3169 = CARTESIAN_POINT ( 'NONE',  ( -2.249192934210769784E-14, 9.016154170237596688, -7.999534413642735764 ) ) ;
#3170 = CARTESIAN_POINT ( 'NONE',  ( 8.000000000000008882, 207.0476921513415220, 57.99886208192144466 ) ) ;
#3171 = ORIENTED_EDGE ( 'NONE', *, *, #30012, .F. ) ;
#3172 = CIRCLE ( 'NONE', #26045, 3.999999999999996003 ) ;
#3173 = CARTESIAN_POINT ( 'NONE',  ( 78.32499999726881867, 145.8408176439707802, 12.60653300113718345 ) ) ;
#3174 = CARTESIAN_POINT ( 'NONE',  ( 33.68749999590321664, 155.0000000000000000, -15.04126587500000767 ) ) ;
#3175 = DIRECTION ( 'NONE',  ( -1.000000000000000000, -0.000000000000000000, -0.000000000000000000 ) ) ;
#3176 = UNCERTAINTY_MEASURE_WITH_UNIT (LENGTH_MEASURE( 1.000000000000000082E-05 ), #18194, 'distance_accuracy_value', 'NONE');
#3177 = CARTESIAN_POINT ( 'NONE',  ( 69.22499999726881015, 160.0630714827496206, -15.58253175000000823 ) ) ;
#3178 = CARTESIAN_POINT ( 'NONE',  ( 2.426778023690261410, 199.3768101843759837, 59.60113791807857808 ) ) ;
#3179 = CARTESIAN_POINT ( 'NONE',  ( -9.000000000000001776, 206.9999999999998863, 103.5000000000000426 ) ) ;
#3180 = CARTESIAN_POINT ( 'NONE',  ( 38.60000000000000853, 159.7113355953771077, -14.50000000000000888 ) ) ;
#3181 = CARTESIAN_POINT ( 'NONE',  ( -6.444103211790928043, 202.2591342207265939, 41.19886208192144750 ) ) ;
#3182 = AXIS2_PLACEMENT_3D ( 'NONE', #6530, #30205, #32410 ) ;
#3183 = CARTESIAN_POINT ( 'NONE',  ( -10.00000000000000711, 207.0476921513413515, 81.50113791807856956 ) ) ;
#3184 = CARTESIAN_POINT ( 'NONE',  ( 125.5000000000000000, 229.9533188057739039, -74.95331880577418815 ) ) ;
#3185 = CARTESIAN_POINT ( 'NONE',  ( 8.062137200540920645, 201.0835637161417822, 65.30113791807858092 ) ) ;
#3186 = AXIS2_PLACEMENT_3D ( 'NONE', #31302, #21229, #5400 ) ;
#3187 = AXIS2_PLACEMENT_3D ( 'NONE', #9813, #33313, #23093 ) ;
#3188 = CARTESIAN_POINT ( 'NONE',  ( 98.19869130599479945, 155.0000000000000000, -32.10452846326769816 ) ) ;
#3189 = CARTESIAN_POINT ( 'NONE',  ( 2.517493886308900919, 214.5937144450984420, 19.40113791807856813 ) ) ;
#3190 = CARTESIAN_POINT ( 'NONE',  ( 3.750000000000005329, 6.495190528383288253, 0.000000000000000000 ) ) ;
#3191 = CARTESIAN_POINT ( 'NONE',  ( -1.098735407080685844, 7.248058225761802476, -6.326622577871337860 ) ) ;
#3192 = CARTESIAN_POINT ( 'NONE',  ( 44.32499999726881157, 145.8408176439707802, 12.60653300113718345 ) ) ;
#3193 = CARTESIAN_POINT ( 'NONE',  ( 12.01549611932652972, 210.8513442034534933, 43.85113791807856387 ) ) ;
#3194 = CARTESIAN_POINT ( 'NONE',  ( 7.897825807688775512, 1.532833846124499910, -7.633607627188418121 ) ) ;
#3195 = CARTESIAN_POINT ( 'NONE',  ( 9.984503880673470277, 203.7031108863295401, 92.15113791807856103 ) ) ;
#3196 = CARTESIAN_POINT ( 'NONE',  ( -6.220909254589537696, 198.5229672870051445, 66.05113791807858092 ) ) ;
#3197 = VECTOR ( 'NONE', #28640, 1000.000000000000000 ) ;
#3198 = CARTESIAN_POINT ( 'NONE',  ( -9.736236675708031640, 214.0148392665760753, 29.79886208192143826 ) ) ;
#3199 = CARTESIAN_POINT ( 'NONE',  ( -6.139770520408224463, 198.4640165459539105, 41.04886208192143471 ) ) ;
#3200 = CARTESIAN_POINT ( 'NONE',  ( 78.19999999453763451, 163.5228861582408797, -11.73074641843674470 ) ) ;
#3201 = CARTESIAN_POINT ( 'NONE',  ( -0.05014649552807705357, 194.3824533091408000, 74.75113791807856956 ) ) ;
#3202 = CARTESIAN_POINT ( 'NONE',  ( 4.984841277089725686, 213.7757310962907411, 85.55113791807858092 ) ) ;
#3203 = CARTESIAN_POINT ( 'NONE',  ( -9.984503880673420539, 203.7031108863293980, 47.34886208192143187 ) ) ;
#3204 = CARTESIAN_POINT ( 'NONE',  ( -14.99999999999998934, -1.734723475976807094E-15, 0.000000000000000000 ) ) ;
#3205 = ORIENTED_EDGE ( 'NONE', *, *, #31790, .F. ) ;
#3206 = CARTESIAN_POINT ( 'NONE',  ( 12.00000000000000711, 207.0476921513415220, 51.99886208192143044 ) ) ;
#3207 = ORIENTED_EDGE ( 'NONE', *, *, #767, .T. ) ;
#3208 = ORIENTED_EDGE ( 'NONE', *, *, #24249, .F. ) ;
#3209 = CARTESIAN_POINT ( 'NONE',  ( 79.07499999726881867, 141.7447067706911810, -9.630534252274387086 ) ) ;
#3210 = CARTESIAN_POINT ( 'NONE',  ( 52.81132485994281467, 150.1262045565065364, 15.00000000000011191 ) ) ;
#3211 = ORIENTED_EDGE ( 'NONE', *, *, #18761, .F. ) ;
#3212 = DIRECTION ( 'NONE',  ( 1.000000000000000000, 1.804112415015879378E-16, 0.000000000000000000 ) ) ;
#3213 = CARTESIAN_POINT ( 'NONE',  ( 8.000000000000008882, 206.9523078486586485, 56.00113791807857666 ) ) ;
#3214 = EDGE_CURVE ( 'NONE', #18911, #30462, #12231, .T. ) ;
#3215 = CARTESIAN_POINT ( 'NONE',  ( -0.05014649552828403384, 217.5146222423826714, 33.24886208192142334 ) ) ;
#3216 = CARTESIAN_POINT ( 'NONE',  ( 66.77499999726880731, 140.1801316387863778, 4.815267126137185549 ) ) ;
#3217 = ORIENTED_EDGE ( 'NONE', *, *, #28326, .T. ) ;
#3218 = CARTESIAN_POINT ( 'NONE',  ( 115.4999999999999858, 155.0000000000000000, -6.938893903907228378E-15 ) ) ;
#3219 = FACE_OUTER_BOUND ( 'NONE', #30584, .T. ) ;
#3220 = CARTESIAN_POINT ( 'NONE',  ( -2.426778023690076225, 199.3768101843759553, 1.898862081921434797 ) ) ;
#3221 = CARTESIAN_POINT ( 'NONE',  ( -8.062137200540920645, 212.9164362838581894, 54.80113791807857382 ) ) ;
#3222 = DIRECTION ( 'NONE',  ( 0.000000000000000000, 0.000000000000000000, 1.000000000000000000 ) ) ;
#3223 = CARTESIAN_POINT ( 'NONE',  ( 0.05014649552810505201, 217.5146222423826714, 40.25113791807856956 ) ) ;
#3224 = CARTESIAN_POINT ( 'NONE',  ( 82.07499999726880446, 168.2552932293087906, 9.630534252274372875 ) ) ;
#3225 = CARTESIAN_POINT ( 'NONE',  ( -4.903702542908436435, 200.1653181626580249, 89.04886208192142760 ) ) ;
#3226 = CARTESIAN_POINT ( 'NONE',  ( 36.52499999726881441, 140.1801316387863778, 4.815267126137185549 ) ) ;
#3227 = CARTESIAN_POINT ( 'NONE',  ( 115.4999999999999858, 126.0449016395812691, -103.9084171661922369 ) ) ;
#3228 = LINE ( 'NONE', #10911, #14173 ) ;
#3229 = CARTESIAN_POINT ( 'NONE',  ( -9.736236675707914401, 199.9851607334237542, 24.20113791807856529 ) ) ;
#3230 = VECTOR ( 'NONE', #6116, 1000.000000000000000 ) ;
#3231 = CARTESIAN_POINT ( 'NONE',  ( 7.970070017554212960, -4.546953124339766283, -8.057670357645358550 ) ) ;
#3232 = CARTESIAN_POINT ( 'NONE',  ( 56.57499999726881157, 145.8408176439707802, 12.60653300113718345 ) ) ;
#3233 = CARTESIAN_POINT ( 'NONE',  ( 3.135527875058820690, 216.4958274776887492, 67.40113791807857524 ) ) ;
#3234 = CARTESIAN_POINT ( 'NONE',  ( -3.135527875058821579, 197.5041725223112223, 29.90113791807856813 ) ) ;
#3235 = CARTESIAN_POINT ( 'NONE',  ( 0.3999999999999975797, 0.000000000000000000, 6.099999999999999645 ) ) ;
#3236 = DIRECTION ( 'NONE',  ( 0.000000000000000000, 0.000000000000000000, 1.000000000000000000 ) ) ;
#3237 = CARTESIAN_POINT ( 'NONE',  ( -6.220909254589682469, 215.4770327129947134, 11.94886208192143684 ) ) ;
#3238 = CARTESIAN_POINT ( 'NONE',  ( 60.19999999453762740, 163.5228861582408797, -11.73074641843674470 ) ) ;
#3239 = EDGE_LOOP ( 'NONE', ( #11599, #32199, #15689, #23418, #19046, #29609 ) ) ;
#3240 = CARTESIAN_POINT ( 'NONE',  ( -3.753561863808691168, 195.6020594897209435, 38.90113791807856813 ) ) ;
#3241 = CARTESIAN_POINT ( 'NONE',  ( 36.78867513459482552, 155.0000000000000000, -15.00000000000002487 ) ) ;
#3242 = CARTESIAN_POINT ( 'NONE',  ( 6.139770520408223575, 215.5359834540460611, 18.54886208192143826 ) ) ;
#3243 = CARTESIAN_POINT ( 'NONE',  ( 0.000000000000000000, 4.685197434473814759, -5.637851296924623057E-15 ) ) ;
#3244 = ORIENTED_EDGE ( 'NONE', *, *, #2528, .F. ) ;
#3245 = CARTESIAN_POINT ( 'NONE',  ( -3.135527875058821579, 197.5041725223112223, 83.90113791807857524 ) ) ;
#3246 = ORIENTED_EDGE ( 'NONE', *, *, #26650, .T. ) ;
#3247 = CARTESIAN_POINT ( 'NONE',  ( -67.50000000000000000, 155.0000000000000000, 6.938893903907228378E-15 ) ) ;
#3248 = DIRECTION ( 'NONE',  ( -1.000000000000000000, -0.000000000000000000, -0.000000000000000000 ) ) ;
#3249 = ORIENTED_EDGE ( 'NONE', *, *, #12805, .F. ) ;
#3250 = CARTESIAN_POINT ( 'NONE',  ( -8.000000000000008882, 207.0476921513413515, 27.50113791807856956 ) ) ;
#3251 = CARTESIAN_POINT ( 'NONE',  ( -64.50000000000000000, 155.0000000000000000, -40.00000000000000000 ) ) ;
#3252 = EDGE_CURVE ( 'NONE', #5646, #15657, #33360, .T. ) ;
#3253 = CARTESIAN_POINT ( 'NONE',  ( 9.984503880673420539, 210.2968891136705167, 6.848862081921434530 ) ) ;
#3254 = CARTESIAN_POINT ( 'NONE',  ( 40.77499999726881441, 140.1801316387863778, 4.815267126137185549 ) ) ;
#3255 = VERTEX_POINT ( 'NONE', #10033 ) ;
#3256 = CARTESIAN_POINT ( 'NONE',  ( 49.92499999726881299, 164.1591823560292198, 12.60653300113718167 ) ) ;
#3257 = DIRECTION ( 'NONE',  ( 0.000000000000000000, 0.000000000000000000, 1.000000000000000000 ) ) ;
#3258 = FACE_OUTER_BOUND ( 'NONE', #3573, .T. ) ;
#3259 = CARTESIAN_POINT ( 'NONE',  ( 92.60208470531341618, 155.0000000000000000, 0.000000000000000000 ) ) ;
#3260 = CARTESIAN_POINT ( 'NONE',  ( 6.139770520408223575, 215.5359834540460611, 78.54886208192144181 ) ) ;
#3261 = CARTESIAN_POINT ( 'NONE',  ( 55.07499999726879736, 141.7447067706911810, -9.630534252274385310 ) ) ;
#3262 = CARTESIAN_POINT ( 'NONE',  ( -0.05014649552810635652, 196.4853777576173002, 23.75113791807855890 ) ) ;
#3263 = DIRECTION ( 'NONE',  ( -0.000000000000000000, -0.000000000000000000, -1.000000000000000000 ) ) ;
#3264 = CARTESIAN_POINT ( 'NONE',  ( 0.05014649552828288198, 194.3824533091408000, 82.74886208192144466 ) ) ;
#3265 = ADVANCED_FACE ( 'NONE', ( #28250 ), #4414, .T. ) ;
#3266 = CARTESIAN_POINT ( 'NONE',  ( 76.50000000000001421, 155.0000000000000000, -14.50000000000000711 ) ) ;
#3267 = CARTESIAN_POINT ( 'NONE',  ( -7.549004593702462351, -4.358419834287841965, -7.700121441565841884 ) ) ;
#3268 = DIRECTION ( 'NONE',  ( 1.000000000000000000, 0.000000000000000000, 0.000000000000000000 ) ) ;
#3269 = CARTESIAN_POINT ( 'NONE',  ( -10.00000000000000711, 207.0476921513413515, 81.50113791807856956 ) ) ;
#3270 = CARTESIAN_POINT ( 'NONE',  ( 6.826425371444817536, -2.641426549045776451, -6.344843397090116355 ) ) ;
#3271 = CARTESIAN_POINT ( 'NONE',  ( 38.57499999726881157, 145.8408176439707802, 12.60653300113718345 ) ) ;
#3272 = CARTESIAN_POINT ( 'NONE',  ( -10.01549611932653860, 203.7984951890123284, 39.35113791807857098 ) ) ;
#3273 = CARTESIAN_POINT ( 'NONE',  ( 77.22499999726881015, 160.0630714827496206, -15.58253175000000823 ) ) ;
#3274 = ORIENTED_EDGE ( 'NONE', *, *, #5485, .F. ) ;
#3275 = CARTESIAN_POINT ( 'NONE',  ( -125.0000000000000000, 0.000000000000000000, -35.00000000000000000 ) ) ;
#3276 = CARTESIAN_POINT ( 'NONE',  ( 40.19999999453763451, 163.5228861582408797, -11.73074641843674470 ) ) ;
#3277 = CARTESIAN_POINT ( 'NONE',  ( -7.456977232089304408, 196.8216656703010301, 6.051137918078566713 ) ) ;
#3279 = ADVANCED_FACE ( 'NONE', ( #4905 ), #25518, .T. ) ;
#3278 = PRODUCT_DEFINITION_SHAPE ( 'NONE', 'NONE',  #33703 ) ;
#3280 = DIRECTION ( 'NONE',  ( -1.000000000000000000, 0.000000000000000000, -0.000000000000000000 ) ) ;
#3281 = CARTESIAN_POINT ( 'NONE',  ( 54.74999999999999289, 7.990820364436481039E-15, 35.00000000000000000 ) ) ;
#3282 = VERTEX_POINT ( 'NONE', #28418 ) ;
#3283 = CARTESIAN_POINT ( 'NONE',  ( 3.044812012439969795, 216.5253028482143520, 96.39886208192145034 ) ) ;
#3284 = CARTESIAN_POINT ( 'NONE',  ( 12.01549611932659367, 203.1486557965466773, 31.14886208192143968 ) ) ;
#3285 = FACE_BOUND ( 'NONE', #4851, .T. ) ;
#3286 = CARTESIAN_POINT ( 'NONE',  ( -0.05014649552810635652, 196.4853777576173002, 53.75113791807857666 ) ) ;
#3287 = ADVANCED_FACE ( 'NONE', ( #15293 ), #30809, .T. ) ;
#3288 = ORIENTED_EDGE ( 'NONE', *, *, #2694, .T. ) ;
#3289 = CARTESIAN_POINT ( 'NONE',  ( 6.444103211790928043, 211.7408657792734061, 15.69886208192143684 ) ) ;
#3290 = CARTESIAN_POINT ( 'NONE',  ( -18.40782811468576341, -21.12650028821926185, -17.71727689882191470 ) ) ;
#3291 = CIRCLE ( 'NONE', #14188, 6.099999999999999645 ) ;
#3292 = ORIENTED_EDGE ( 'NONE', *, *, #16187, .T. ) ;
#3293 = CARTESIAN_POINT ( 'NONE',  ( -4.903702542908436435, 200.1653181626580249, 89.04886208192142760 ) ) ;
#3294 = CARTESIAN_POINT ( 'NONE',  ( 2.426778023690261410, 199.3768101843759837, 26.60113791807856742 ) ) ;
#3295 = PLANE ( 'NONE',  #6420 ) ;
#3296 = ORIENTED_EDGE ( 'NONE', *, *, #9534, .T. ) ;
#3297 = CARTESIAN_POINT ( 'NONE',  ( 3.080866544135574259, 6.881514909250401324, -7.026396753507782478 ) ) ;
#3298 = CARTESIAN_POINT ( 'NONE',  ( 37.27499999726880020, 149.9369285172503510, -15.58253175000000823 ) ) ;
#3299 = FACE_OUTER_BOUND ( 'NONE', #22987, .T. ) ;
#3300 = CARTESIAN_POINT ( 'NONE',  ( 4.984841277089725686, 213.7757310962907411, 100.5511379180785809 ) ) ;
#3301 = DIRECTION ( 'NONE',  ( 1.000000000000000000, 0.000000000000000000, 0.000000000000000000 ) ) ;
#3302 = CARTESIAN_POINT ( 'NONE',  ( 53.90000000000000568, 141.2096805137202580, 4.480746418436733158 ) ) ;
#3303 = CARTESIAN_POINT ( 'NONE',  ( 6.500168698208244500, 202.3363017425938324, 76.29886208192142760 ) ) ;
#3304 = DIRECTION ( 'NONE',  ( -1.000000000000000000, 0.000000000000000000, 0.000000000000000000 ) ) ;
#3305 = ADVANCED_FACE ( 'NONE', ( #15472 ), #9294, .T. ) ;
#3306 = CARTESIAN_POINT ( 'NONE',  ( 54.82499999726879736, 141.7447067706911810, -9.630534252274385310 ) ) ;
#3307 = CARTESIAN_POINT ( 'NONE',  ( -3.044812012440131443, 216.5253028482142952, 7.101137918078566535 ) ) ;
#3308 = DIRECTION ( 'NONE',  ( -0.9945218953682772867, 1.280104479604772081E-17, -0.1045284632676156678 ) ) ;
#3309 = AXIS2_PLACEMENT_3D ( 'NONE', #30637, #14619, #6614 ) ;
#3310 = CARTESIAN_POINT ( 'NONE',  ( 65.42499999726881299, 168.2552932293087906, -9.630534252274387086 ) ) ;
#3311 = CARTESIAN_POINT ( 'NONE',  ( 76.37499999726881583, 155.0000000000000000, 15.58253174999999402 ) ) ;
#3312 = CARTESIAN_POINT ( 'NONE',  ( -9.736236675707914401, 199.9851607334237542, 75.20113791807857240 ) ) ;
#3313 = CARTESIAN_POINT ( 'NONE',  ( 4.000000000000000000, 0.000000000000000000, 0.000000000000000000 ) ) ;
#3314 = EDGE_CURVE ( 'NONE', #10897, #33645, #17856, .T. ) ;
#3315 = CARTESIAN_POINT ( 'NONE',  ( 0.05014649552810506589, 217.5146222423826714, 100.2511379180785696 ) ) ;
#3316 = CARTESIAN_POINT ( 'NONE',  ( 100.4058500716420781, 155.0000000000000000, -12.99999999999998401 ) ) ;
#3317 = EDGE_LOOP ( 'NONE', ( #12594, #14639, #9064 ) ) ;
#3318 = CARTESIAN_POINT ( 'NONE',  ( 0.05014649552828288198, 194.3824533091408000, 103.7488620819214304 ) ) ;
#3319 = CARTESIAN_POINT ( 'NONE',  ( 9.736236675708031640, 199.9851607334238963, 58.29886208192143471 ) ) ;
#3320 = CARTESIAN_POINT ( 'NONE',  ( 9.984503880673420539, 210.2968891136705736, 69.84886208192143897 ) ) ;
#3321 = CARTESIAN_POINT ( 'NONE',  ( -12.01549611932652972, 203.1486557965464499, 102.3511379180785639 ) ) ;
#3322 = CARTESIAN_POINT ( 'NONE',  ( -65.24999999999998579, -6.704941225331758828E-15, 35.00000000000000000 ) ) ;
#3323 = CARTESIAN_POINT ( 'NONE',  ( 10.01549611932653860, 210.2015048109876716, 25.85113791807856742 ) ) ;
#3324 = ADVANCED_FACE ( 'NONE', ( #15125 ), #7471, .T. ) ;
#3325 = CARTESIAN_POINT ( 'NONE',  ( 10.00000000000000711, 207.0476921513415220, 75.99886208192144466 ) ) ;
#3326 = ORIENTED_EDGE ( 'NONE', *, *, #17837, .F. ) ;
#3327 = CARTESIAN_POINT ( 'NONE',  ( -10.01549611932653860, 203.7984951890123284, 99.35113791807857808 ) ) ;
#3328 = EDGE_LOOP ( 'NONE', ( #4132, #17295 ) ) ;
#3329 = CARTESIAN_POINT ( 'NONE',  ( -6.127431526422343306E-17, 9.147862274876549904, -8.047472243342932430 ) ) ;
#3330 = CARTESIAN_POINT ( 'NONE',  ( -6.500168698208244500, 211.6636982574061676, 59.79886208192143471 ) ) ;
#3331 = ORIENTED_EDGE ( 'NONE', *, *, #15173, .T. ) ;
#3332 = CARTESIAN_POINT ( 'NONE',  ( 76.02499999726880731, 160.0630714827496206, 15.58253174999999224 ) ) ;
#3333 = EDGE_LOOP ( 'NONE', ( #162, #13018, #29872, #22354, #4251, #17416 ) ) ;
#3334 = CYLINDRICAL_SURFACE ( 'NONE', #3651, 1.000000000000000222 ) ;
#3335 = AXIS2_PLACEMENT_3D ( 'NONE', #12117, #27449, #14495 ) ;
#3336 = B_SPLINE_CURVE_WITH_KNOTS ( 'NONE', 3,
 ( #16706, #32047, #8710, #16537, #24549, #26934 ),
 .UNSPECIFIED., .F., .F.,
 ( 4, 2, 4 ),
 ( 0.000000000000000000, 0.0004189869898914161677, 0.0008379739797828302753 ),
 .UNSPECIFIED. ) ;
#3337 = CARTESIAN_POINT ( 'NONE',  ( 68.02499999726882152, 160.0630714827496206, 15.58253174999999402 ) ) ;
#3338 = CARTESIAN_POINT ( 'NONE',  ( 6.500168698208129925, 211.6636982574063381, 73.70113791807857240 ) ) ;
#3339 = CARTESIAN_POINT ( 'NONE',  ( 16.00000000000000000, 0.000000000000000000, 0.000000000000000000 ) ) ;
#3340 = CARTESIAN_POINT ( 'NONE',  ( 4.515071337844623223, 29.14748715311447924, -1.088725517910807294 ) ) ;
#3341 = CARTESIAN_POINT ( 'NONE',  ( 36.00000000000000711, 139.7537977485451393, -4.138211985947621020E-15 ) ) ;
#3342 = CARTESIAN_POINT ( 'NONE',  ( 7.984503880673422316, 209.6470497212048372, 42.84886208192143897 ) ) ;
#3343 = CARTESIAN_POINT ( 'NONE',  ( -6.139770520408369237, 215.5359834540460042, 75.95113791807857240 ) ) ;
#3344 = CARTESIAN_POINT ( 'NONE',  ( 10.00000000000000711, 206.9523078486586201, 65.00113791807856956 ) ) ;
#3345 = EDGE_CURVE ( 'NONE', #27265, #28748, #10942, .T. ) ;
#3346 = FACE_OUTER_BOUND ( 'NONE', #29316, .T. ) ;
#3347 = CARTESIAN_POINT ( 'NONE',  ( 0.05014649552807626948, 215.4116977939061144, 22.25113791807856956 ) ) ;
#3348 = CARTESIAN_POINT ( 'NONE',  ( -27.50000000000000711, 10.70896984529285767, -16.90208611084169732 ) ) ;
#3349 = CARTESIAN_POINT ( 'NONE',  ( -2.241046694639089232, 6.576374040525770681, -6.171384342982497273 ) ) ;
#3350 = CARTESIAN_POINT ( 'NONE',  ( 43.52499999726881441, 169.8198683612136222, -4.815267126137197984 ) ) ;
#3351 = CARTESIAN_POINT ( 'NONE',  ( -3.753561863808691168, 195.6020594897209435, 50.90113791807858235 ) ) ;
#3352 = LINE ( 'NONE', #24476, #16227 ) ;
#3353 = CARTESIAN_POINT ( 'NONE',  ( -8.118202686958039038, 201.1607312380087080, 93.20113791807857240 ) ) ;
#3354 = ADVANCED_FACE ( 'NONE', ( #10372 ), #10201, .F. ) ;
#3355 = CARTESIAN_POINT ( 'NONE',  ( 8.118202686958039038, 212.8392687619912635, 67.70113791807858661 ) ) ;
#3356 = CARTESIAN_POINT ( 'NONE',  ( 12.01549611932659367, 203.1486557965466773, 31.14886208192143968 ) ) ;
#3357 = CARTESIAN_POINT ( 'NONE',  ( 10.00000000000000711, 207.0476921513415220, 33.99886208192143044 ) ) ;
#3358 = CONICAL_SURFACE ( 'NONE', #11467, 32.10452846326769816, 1.466076571675243523 ) ;
#3359 = CARTESIAN_POINT ( 'NONE',  ( 77.19999999453763451, 146.4771138417591203, 11.73074641843673227 ) ) ;
#3360 = CARTESIAN_POINT ( 'NONE',  ( 3.753561863808689836, 218.3979405102790565, 73.40113791807856103 ) ) ;
#3361 = CARTESIAN_POINT ( 'NONE',  ( -2.426778023690262742, 214.6231898156240163, 88.10113791807857808 ) ) ;
#3362 = CARTESIAN_POINT ( 'NONE',  ( 8.118202686958138514, 201.1607312380088501, 52.29886208192143471 ) ) ;
#3363 = DIRECTION ( 'NONE',  ( 0.000000000000000000, 0.000000000000000000, 1.000000000000000000 ) ) ;
#3364 = EDGE_LOOP ( 'NONE', ( #33433, #32436, #8382, #28584, #8212, #13173, #31098 ) ) ;
#3365 = CARTESIAN_POINT ( 'NONE',  ( -7.456977232089471386, 217.1783343296987709, 59.94886208192143329 ) ) ;
#3366 = AXIS2_PLACEMENT_3D ( 'NONE', #30771, #20379, #27859 ) ;
#3367 = ORIENTED_EDGE ( 'NONE', *, *, #21211, .T. ) ;
#3368 = CARTESIAN_POINT ( 'NONE',  ( 4.984841277089891776, 200.2242689037093726, 37.44886208192144039 ) ) ;
#3369 = ORIENTED_EDGE ( 'NONE', *, *, #9298, .F. ) ;
#3370 = CARTESIAN_POINT ( 'NONE',  ( 76.77499999726880731, 140.1801316387863778, 4.815267126137185549 ) ) ;
#3371 = DIRECTION ( 'NONE',  ( 0.000000000000000000, 0.000000000000000000, -1.000000000000000000 ) ) ;
#3372 = CARTESIAN_POINT ( 'NONE',  ( 0.000000000000000000, 0.000000000000000000, -0.4201245229258211977 ) ) ;
#3373 = CARTESIAN_POINT ( 'NONE',  ( 8.015496119326531499, 209.5516654185219636, 52.85113791807857098 ) ) ;
#3374 = CARTESIAN_POINT ( 'NONE',  ( 8.399999999999998579, 5.388445916248354999E-16, 4.400000000000001243 ) ) ;
#3375 = CARTESIAN_POINT ( 'NONE',  ( -8.118202686958138514, 212.8392687619910930, 35.79886208192143471 ) ) ;
#3376 = CARTESIAN_POINT ( 'NONE',  ( 66.87499999726880162, 138.6155565068815747, -3.929120461958505118E-15 ) ) ;
#3377 = VERTEX_POINT ( 'NONE', #10037 ) ;
#3378 = CARTESIAN_POINT ( 'NONE',  ( 65.25000000000000000, 7.347880794884118356E-15, 35.00000000000000000 ) ) ;
#3379 = PRODUCT_DEFINITION_FORMATION_WITH_SPECIFIED_SOURCE ( 'ANY', '', #25205, .NOT_KNOWN. ) ;
#3380 = CARTESIAN_POINT ( 'NONE',  ( 32.50000000000000000, 155.0000000000000000, -6.938893903907228378E-15 ) ) ;
#3381 = CARTESIAN_POINT ( 'NONE',  ( 8.015496119326595448, 204.4483345814782638, 13.14886208192143613 ) ) ;
#3382 = CARTESIAN_POINT ( 'NONE',  ( 10.01549611932653860, 210.2015048109876716, 49.85113791807857808 ) ) ;
#3383 = CARTESIAN_POINT ( 'NONE',  ( 6.601567268551444378, -5.319966374295973743, -7.792327460285856766 ) ) ;
#3384 = CARTESIAN_POINT ( 'NONE',  ( 8.118202686958039038, 212.8392687619912635, 40.70113791807857240 ) ) ;
#3385 = CARTESIAN_POINT ( 'NONE',  ( 86.47499999726879594, 149.9369285172503510, 15.58253174999999580 ) ) ;
#3386 = SHAPE_DEFINITION_REPRESENTATION ( #33668, #2185 ) ;
#3387 = CARTESIAN_POINT ( 'NONE',  ( 2.426778023690075337, 214.6231898156240447, 102.3988620819214361 ) ) ;
#3388 = CIRCLE ( 'NONE', #6656, 4.199999999999988631 ) ;
#3389 = CARTESIAN_POINT ( 'NONE',  ( 38.72499999726881015, 140.1801316387863778, -4.815267126137194431 ) ) ;
#3390 = CARTESIAN_POINT ( 'NONE',  ( 80.98867513459481415, 163.8167787843871110, -12.13525491562423397 ) ) ;
#3391 = CARTESIAN_POINT ( 'NONE',  ( 145.0000000000000000, 3.306546357697854049E-14, 35.00200000000000244 ) ) ;
#3392 = CARTESIAN_POINT ( 'NONE',  ( 3.662846001190051659, 195.5725841191953691, 20.60113791807856742 ) ) ;
#3393 = CARTESIAN_POINT ( 'NONE',  ( -1.049032378834002577, -6.899894373156699068, -0.3607371497494579748 ) ) ;
#3394 = CARTESIAN_POINT ( 'NONE',  ( 61.87499999726881583, 171.3844434931184253, -7.942151717890132712E-15 ) ) ;
#3395 = AXIS2_PLACEMENT_3D ( 'NONE', #27713, #7444, #17660 ) ;
#3396 = CARTESIAN_POINT ( 'NONE',  ( -8.118202686958039038, 201.1607312380087080, 63.20113791807857240 ) ) ;
#3397 = CARTESIAN_POINT ( 'NONE',  ( -0.05014649552810635652, 196.4853777576173002, 35.75113791807857666 ) ) ;
#3398 = DIRECTION ( 'NONE',  ( -1.000000000000000000, 0.000000000000000000, 0.000000000000000000 ) ) ;
#3399 = CARTESIAN_POINT ( 'NONE',  ( -10.83124253962820305, 25.50084400951695329, -17.88577775926227886 ) ) ;
#3400 = CARTESIAN_POINT ( 'NONE',  ( -6.220909254589682469, 215.4770327129947134, 8.948862081921435063 ) ) ;
#3401 = CARTESIAN_POINT ( 'NONE',  ( 61.39999999453763024, 141.2096805137202580, 4.480746418436733158 ) ) ;
#3402 = ORIENTED_EDGE ( 'NONE', *, *, #11389, .T. ) ;
#3403 = CARTESIAN_POINT ( 'NONE',  ( -11.98450388067348804, 210.9467285061362247, 51.65113791807857524 ) ) ;
#3404 = CARTESIAN_POINT ( 'NONE',  ( 76.91132485994280898, 146.1832212156128890, 12.13525491562421976 ) ) ;
#3405 = CARTESIAN_POINT ( 'NONE',  ( -6.220909254589682469, 215.4770327129946850, 17.94886208192143684 ) ) ;
#3406 = CARTESIAN_POINT ( 'NONE',  ( 72.11132485994281183, 169.2658477444273331, -4.635254915624224203 ) ) ;
#3407 = EDGE_LOOP ( 'NONE', ( #13104, #13972, #13638, #27288, #10278 ) ) ;
#3408 = CARTESIAN_POINT ( 'NONE',  ( 10.01549611932653860, 210.2015048109876716, 79.85113791807853545 ) ) ;
#3409 = ORIENTED_EDGE ( 'NONE', *, *, #14549, .F. ) ;
#3410 = DIRECTION ( 'NONE',  ( 0.000000000000000000, 0.000000000000000000, -1.000000000000000000 ) ) ;
#3411 = DIRECTION ( 'NONE',  ( 0.000000000000000000, -1.000000000000000000, 0.000000000000000000 ) ) ;
#3412 = ORIENTED_EDGE ( 'NONE', *, *, #18364, .F. ) ;
#3413 = VECTOR ( 'NONE', #32433, 1000.000000000000000 ) ;
#3414 = CARTESIAN_POINT ( 'NONE',  ( -4.984841277089726574, 200.2242689037092305, 24.05113791807857027 ) ) ;
#3415 = VECTOR ( 'NONE', #9617, 1000.000000000000000 ) ;
#3416 = CARTESIAN_POINT ( 'NONE',  ( -60.02418147676856108, 194.9506531851598936, 1.988357156115594826 ) ) ;
#3417 = CARTESIAN_POINT ( 'NONE',  ( 3.135527875058981895, 197.5041725223112792, 1.598862081921434530 ) ) ;
#3418 = CIRCLE ( 'NONE', #12698, 2.149999999999985256 ) ;
#3419 = CARTESIAN_POINT ( 'NONE',  ( 47.87499999726880162, 171.3844434931184253, -7.942151717890134290E-15 ) ) ;
#3420 = ORIENTED_EDGE ( 'NONE', *, *, #23975, .T. ) ;
#3421 = CARTESIAN_POINT ( 'NONE',  ( 58.22499999726881015, 149.9369285172503510, 15.58253174999999580 ) ) ;
#3422 = CARTESIAN_POINT ( 'NONE',  ( 7.500000000000007105, -4.330127018922196314, -7.564338275809341816 ) ) ;
#3423 = LINE ( 'NONE', #13985, #15074 ) ;
#3424 = CARTESIAN_POINT ( 'NONE',  ( 77.71132485994280614, 155.0000000000000000, -15.00000000000002487 ) ) ;
#3425 = CARTESIAN_POINT ( 'NONE',  ( -0.05014649552828403384, 217.5146222423826714, 87.24886208192143044 ) ) ;
#3426 = CARTESIAN_POINT ( 'NONE',  ( 57.07499999726879736, 141.7447067706911810, -9.630534252274385310 ) ) ;
#3427 = CARTESIAN_POINT ( 'NONE',  ( 10.00000000000000711, 206.9523078486586201, 20.00113791807856600 ) ) ;
#3428 = CARTESIAN_POINT ( 'NONE',  ( 47.58867513459481557, 163.8167787843871110, 12.13525491562421621 ) ) ;
#3429 = CARTESIAN_POINT ( 'NONE',  ( -0.05014649552828442242, 219.6175466908591716, 75.24886208192143044 ) ) ;
#3430 = CIRCLE ( 'NONE', #18161, 2.428571428571428381 ) ;
#3431 = CARTESIAN_POINT ( 'NONE',  ( 71.50000000000001421, 155.0000000000000000, 14.49999999999999467 ) ) ;
#3432 = CARTESIAN_POINT ( 'NONE',  ( 64.78867513459482552, 155.0000000000000000, -15.00000000000002487 ) ) ;
#3433 = CARTESIAN_POINT ( 'NONE',  ( 117.5000000000000000, 155.0000000000000000, -6.938893903907228378E-15 ) ) ;
#3434 = CARTESIAN_POINT ( 'NONE',  ( 0.05014649552810505201, 217.5146222423826714, 91.25113791807858377 ) ) ;
#3435 = CARTESIAN_POINT ( 'NONE',  ( 33.58867513459482268, 163.8167787843871110, 12.13525491562421621 ) ) ;
#3436 = CARTESIAN_POINT ( 'NONE',  ( 37.77499999726881441, 169.8198683612136222, -4.815267126137197984 ) ) ;
#3437 = CARTESIAN_POINT ( 'NONE',  ( 6.220909254589536808, 215.4770327129947702, 34.55113791807855250 ) ) ;
#3438 = CARTESIAN_POINT ( 'NONE',  ( 78.32499999726881867, 145.8408176439707802, 12.60653300113718345 ) ) ;
#3439 = EDGE_LOOP ( 'NONE', ( #32526, #8742, #29770 ) ) ;
#3440 = CARTESIAN_POINT ( 'NONE',  ( 100.2066581602377653, 155.0000000000000000, 0.000000000000000000 ) ) ;
#3441 = CARTESIAN_POINT ( 'NONE',  ( 39.99999999453762456, 155.0000000000000000, -14.50000000000000711 ) ) ;
#3442 = CARTESIAN_POINT ( 'NONE',  ( -9.680171189290831535, 214.0920067884431148, 15.80113791807856849 ) ) ;
#3443 = AXIS2_PLACEMENT_3D ( 'NONE', #27976, #32741, #17244 ) ;
#3444 = LINE ( 'NONE', #396, #14264 ) ;
#3445 = EDGE_CURVE ( 'NONE', #889, #23658, #5075, .T. ) ;
#3446 = VECTOR ( 'NONE', #9745, 1000.000000000000000 ) ;
#3447 = CARTESIAN_POINT ( 'NONE',  ( 0.000000000000000000, 0.000000000000000000, 0.000000000000000000 ) ) ;
#3448 = ORIENTED_EDGE ( 'NONE', *, *, #24308, .F. ) ;
#3449 = CARTESIAN_POINT ( 'NONE',  ( -10.01549611932659545, 210.2015048109875011, 98.64886208192145034 ) ) ;
#3450 = CARTESIAN_POINT ( 'NONE',  ( -3.662846001189865142, 195.5725841191952838, 34.89886208192143613 ) ) ;
#3451 = DIRECTION ( 'NONE',  ( 1.000000000000000000, 0.000000000000000000, 0.000000000000000000 ) ) ;
#3452 = CARTESIAN_POINT ( 'NONE',  ( -8.118202686958039038, 201.1607312380087080, 48.20113791807857950 ) ) ;
#3453 = ORIENTED_EDGE ( 'NONE', *, *, #20858, .T. ) ;
#3454 = CARTESIAN_POINT ( 'NONE',  ( 8.015496119326595448, 204.4483345814782638, 16.14886208192143968 ) ) ;
#3455 = CARTESIAN_POINT ( 'NONE',  ( 50.08867513459482268, 142.2402378747194405, 9.270509831248432420 ) ) ;
#3456 = ORIENTED_EDGE ( 'NONE', *, *, #16863, .T. ) ;
#3458 = CARTESIAN_POINT ( 'NONE',  ( -6.444103211790928043, 202.2591342207265939, 98.19886208192144750 ) ) ;
#3457 = STYLED_ITEM ( 'NONE', ( #27352 ), #33198 ) ;
#3459 = CARTESIAN_POINT ( 'NONE',  ( 2.426778023690261410, 199.3768101843759837, 35.60113791807857098 ) ) ;
#3460 = CARTESIAN_POINT ( 'NONE',  ( 33.47499999726881015, 160.0630714827496206, -15.58253175000000823 ) ) ;
#3461 = VERTEX_POINT ( 'NONE', #30987 ) ;
#3462 = CARTESIAN_POINT ( 'NONE',  ( 37.82499999726881157, 168.2552932293087906, 9.630534252274372875 ) ) ;
#3463 = STYLED_ITEM ( 'NONE', ( #15005 ), #12506 ) ;
#3464 = CARTESIAN_POINT ( 'NONE',  ( -8.062137200540822946, 201.0835637161416400, 62.19886208192143329 ) ) ;
#3465 = AXIS2_PLACEMENT_3D ( 'NONE', #8332, #16653, #29615 ) ;
#3466 = CARTESIAN_POINT ( 'NONE',  ( 35.97499999726881015, 169.8198683612136222, 4.815267126137181997 ) ) ;
#3467 = DIRECTION ( 'NONE',  ( -1.000000000000000000, -0.000000000000000000, -0.000000000000000000 ) ) ;
#3468 = CARTESIAN_POINT ( 'NONE',  ( 6.444103211791042618, 202.2591342207267644, 101.3011379180785951 ) ) ;
#3469 = B_SPLINE_CURVE_WITH_KNOTS ( 'NONE', 3,
 ( #28829, #26110, #12821, #23043, #20318, #5319, #33439, #25769, #8057, #15209 ),
 .UNSPECIFIED., .F., .F.,
 ( 4, 2, 2, 2, 4 ),
 ( 0.01051144076094935251, 0.01162027323572611265, 0.01272910571050287452, 0.01383793818527963640, 0.01494677066005639827 ),
 .UNSPECIFIED. ) ;
#3470 = CARTESIAN_POINT ( 'NONE',  ( 132.3999999999999773, 229.9533188057739039, -74.95331880577418815 ) ) ;
#3471 = CARTESIAN_POINT ( 'NONE',  ( 52.80000000000000426, 167.3344367211045096, -8.961492836873482304 ) ) ;
#3472 = CARTESIAN_POINT ( 'NONE',  ( -6.444103211790928043, 202.2591342207265939, 71.19886208192144750 ) ) ;
#3473 = DIRECTION ( 'NONE',  ( -0.000000000000000000, -0.000000000000000000, 1.000000000000000000 ) ) ;
#3474 = EDGE_CURVE ( 'NONE', #5597, #4891, #5508, .T. ) ;
#3475 = CARTESIAN_POINT ( 'NONE',  ( 56.12499999726880873, 155.0000000000000000, 15.58253174999999402 ) ) ;
#3476 =( GEOMETRIC_REPRESENTATION_CONTEXT ( 3 ) GLOBAL_UNCERTAINTY_ASSIGNED_CONTEXT ( ( #16111 ) ) GLOBAL_UNIT_ASSIGNED_CONTEXT ( ( #32711, #27439, #10407 ) ) REPRESENTATION_CONTEXT ( 'NONE', 'WORKASPACE' ) );
#3478 = ORIENTED_EDGE ( 'NONE', *, *, #28138, .F. ) ;
#3477 = CARTESIAN_POINT ( 'NONE',  ( -10.00000000000000711, 207.0476921513413515, 12.50113791807856778 ) ) ;
#3479 = CARTESIAN_POINT ( 'NONE',  ( 92.60208470531341618, 155.0000000000000000, -31.00000000000000000 ) ) ;
#3480 = CARTESIAN_POINT ( 'NONE',  ( 64.52499999726882152, 140.1801316387863778, 4.815267126137185549 ) ) ;
#3481 = CARTESIAN_POINT ( 'NONE',  ( 77.17499999726881299, 145.8408176439707802, -12.60653300113719588 ) ) ;
#3482 = CARTESIAN_POINT ( 'NONE',  ( -3.753561863808691168, 195.6020594897209435, 80.90113791807858945 ) ) ;
#3483 = CARTESIAN_POINT ( 'NONE',  ( -0.05014649552810635652, 196.4853777576173002, 101.7511379180785696 ) ) ;
#3484 = ADVANCED_FACE ( 'NONE', ( #2704 ), #25862, .F. ) ;
#3485 = CARTESIAN_POINT ( 'NONE',  ( 83.88867513459483405, 150.1262045565062238, 14.99999999999988454 ) ) ;
#3486 = VERTEX_POINT ( 'NONE', #18026 ) ;
#3487 = CARTESIAN_POINT ( 'NONE',  ( 8.118202686958138514, 201.1607312380088501, 1.298862081921434486 ) ) ;
#3488 = CARTESIAN_POINT ( 'NONE',  ( -9.680171189290716072, 199.9079932115567146, 65.19886208192143329 ) ) ;
#3489 = CARTESIAN_POINT ( 'NONE',  ( 8.118202686958138514, 201.1607312380088501, 70.29886208192142760 ) ) ;
#3490 = AXIS2_PLACEMENT_3D ( 'NONE', #3890, #6624, #19900 ) ;
#3491 = CARTESIAN_POINT ( 'NONE',  ( 11.98450388067341876, 210.9467285061363953, 6.848862081921435419 ) ) ;
#3492 = LINE ( 'NONE', #13883, #33347 ) ;
#3493 = CARTESIAN_POINT ( 'NONE',  ( 9.984503880673470277, 203.7031108863295401, 20.15113791807856813 ) ) ;
#3494 = CIRCLE ( 'NONE', #11124, 6.500000000000000888 ) ;
#3495 = CARTESIAN_POINT ( 'NONE',  ( -6.220909254589682469, 215.4770327129946850, 86.94886208192141908 ) ) ;
#3496 = ORIENTED_EDGE ( 'NONE', *, *, #6032, .T. ) ;
#3497 = EDGE_CURVE ( 'NONE', #8044, #608, #15529, .T. ) ;
#3498 = CARTESIAN_POINT ( 'NONE',  ( 39.11132485994280472, 140.7341522555726669, 4.635254915624211769 ) ) ;
#3499 = ORIENTED_EDGE ( 'NONE', *, *, #3139, .T. ) ;
#3500 = FACE_OUTER_BOUND ( 'NONE', #21099, .T. ) ;
#3501 = CARTESIAN_POINT ( 'NONE',  ( -8.000000000000008882, 206.9523078486584780, 68.49886208192144466 ) ) ;
#3502 = VERTEX_POINT ( 'NONE', #28590 ) ;
#3503 = CARTESIAN_POINT ( 'NONE',  ( 79.02499999726879309, 149.9369285172503510, -15.58253175000000823 ) ) ;
#3504 = ORIENTED_EDGE ( 'NONE', *, *, #3552, .F. ) ;
#3505 = CARTESIAN_POINT ( 'NONE',  ( 6.838249506730350369, 3.995160516047499222, -6.573190279698081895 ) ) ;
#3506 = CARTESIAN_POINT ( 'NONE',  ( 70.72499999726881015, 140.1801316387863778, -4.815267126137194431 ) ) ;
#3507 = ADVANCED_FACE ( 'NONE', ( #4574 ), #14960, .T. ) ;
#3508 = CARTESIAN_POINT ( 'NONE',  ( -7.984503880673488041, 209.6470497212046098, 69.65113791807856103 ) ) ;
#3509 = CARTESIAN_POINT ( 'NONE',  ( 3.499999999999996891, 0.000000000000000000, 9.480888224575629408 ) ) ;
#3510 = CARTESIAN_POINT ( 'NONE',  ( 57.71132485994280614, 155.0000000000000000, -15.00000000000002487 ) ) ;
#3511 = CARTESIAN_POINT ( 'NONE',  ( 33.30000000000000426, 163.5228861582408797, 11.73074641843673049 ) ) ;
#3512 = CARTESIAN_POINT ( 'NONE',  ( 6.444103211790928043, 211.7408657792734061, 39.69886208192144750 ) ) ;
#3513 = CARTESIAN_POINT ( 'NONE',  ( 3.044812012440130555, 197.4746971517856764, 83.60113791807857808 ) ) ;
#3514 = CARTESIAN_POINT ( 'NONE',  ( -10.01549611932653860, 203.7984951890123284, 63.35113791807857098 ) ) ;
#3515 = DIRECTION ( 'NONE',  ( -0.000000000000000000, -0.000000000000000000, 1.000000000000000000 ) ) ;
#3516 = CARTESIAN_POINT ( 'NONE',  ( -8.000000000000008882, 207.0476921513413515, 24.50113791807856600 ) ) ;
#3517 = CARTESIAN_POINT ( 'NONE',  ( 128.2263702798683198, -4.198250922590419876, 35.00001199999999812 ) ) ;
#3518 = CARTESIAN_POINT ( 'NONE',  ( 59.98867513459482836, 146.1832212156128890, 12.13525491562421976 ) ) ;
#3519 = CARTESIAN_POINT ( 'NONE',  ( 41.52499999726881441, 169.8198683612136222, -4.815267126137197984 ) ) ;
#3520 = CARTESIAN_POINT ( 'NONE',  ( -7.456977232089304408, 196.8216656703010301, 48.05113791807856671 ) ) ;
#3521 = CARTESIAN_POINT ( 'NONE',  ( 7.499999999999999112, -1.614186302720606481, -7.450236204328171574 ) ) ;
#3522 = CARTESIAN_POINT ( 'NONE',  ( 8.062137200540920645, 201.0835637161417822, 92.30113791807858092 ) ) ;
#3523 = CARTESIAN_POINT ( 'NONE',  ( 8.118202686958039038, 212.8392687619912635, 64.70113791807857240 ) ) ;
#3524 = CARTESIAN_POINT ( 'NONE',  ( 7.375838497908012492, 217.2372850707501186, 36.54886208192144181 ) ) ;
#3525 = CARTESIAN_POINT ( 'NONE',  ( 6.139770520408223575, 215.5359834540460611, 36.54886208192142760 ) ) ;
#3526 = CARTESIAN_POINT ( 'NONE',  ( 84.89999999453762314, 159.7113355953771077, 14.49999999999999289 ) ) ;
#3527 = CARTESIAN_POINT ( 'NONE',  ( -3.753561863808691168, 195.6020594897209435, 80.90113791807858945 ) ) ;
#3528 = CARTESIAN_POINT ( 'NONE',  ( 0.05014649552807626948, 215.4116977939061144, 100.2511379180785696 ) ) ;
#3529 = CARTESIAN_POINT ( 'NONE',  ( -10.00000000000000711, 206.9523078486584495, 56.49886208192143755 ) ) ;
#3530 = FILL_AREA_STYLE ('',( #9315 ) ) ;
#3531 = ORIENTED_EDGE ( 'NONE', *, *, #28929, .T. ) ;
#3532 = CARTESIAN_POINT ( 'NONE',  ( -12.00000000000000711, 206.9523078486584780, 62.49886208192143044 ) ) ;
#3533 = ORIENTED_EDGE ( 'NONE', *, *, #31790, .T. ) ;
#3534 = CARTESIAN_POINT ( 'NONE',  ( -6.500168698208244500, 211.6636982574061676, 35.79886208192144181 ) ) ;
#3535 = EDGE_LOOP ( 'NONE', ( #12348, #25217, #30285, #15246 ) ) ;
#3536 = ADVANCED_FACE ( 'NONE', ( #2016 ), #12405, .T. ) ;
#3537 = EDGE_CURVE ( 'NONE', #20010, #29148, #19314, .T. ) ;
#3538 = CARTESIAN_POINT ( 'NONE',  ( 79.87499999726880162, 171.3844434931184253, -7.942151717890134290E-15 ) ) ;
#3539 = CARTESIAN_POINT ( 'NONE',  ( 64.50000000000000000, -73.00000000000000000, -20.00000000000000000 ) ) ;
#3540 = DIRECTION ( 'NONE',  ( 0.000000000000000000, -0.7071067811865475727, -0.7071067811865475727 ) ) ;
#3541 = CARTESIAN_POINT ( 'NONE',  ( 6.444103211791042618, 202.2591342207267644, 50.30113791807858092 ) ) ;
#3542 = ADVANCED_FACE ( 'NONE', ( #22038 ), #24430, .T. ) ;
#3543 = CARTESIAN_POINT ( 'NONE',  ( 5.000000000000000000, 2.342598717236900718, -4.057500000000001883 ) ) ;
#3544 =( REPRESENTATION_RELATIONSHIP ('NONE','NONE', #25663, #30243 ) REPRESENTATION_RELATIONSHIP_WITH_TRANSFORMATION ( #10040 )SHAPE_REPRESENTATION_RELATIONSHIP( ) );
#3545 = CARTESIAN_POINT ( 'NONE',  ( -8.118202686958138514, 212.8392687619910930, 32.79886208192143471 ) ) ;
#3546 = CARTESIAN_POINT ( 'NONE',  ( 67.17499999726881299, 145.8408176439707802, -12.60653300113719588 ) ) ;
#3547 = EDGE_LOOP ( 'NONE', ( #31464, #2889, #14472, #25548 ) ) ;
#3548 = CARTESIAN_POINT ( 'NONE',  ( 36.11132485994280472, 169.2658477444273331, -4.635254915624224203 ) ) ;
#3549 = CARTESIAN_POINT ( 'NONE',  ( 52.48867513459483547, 142.2402378747194405, -9.270509831248439525 ) ) ;
#3550 = CARTESIAN_POINT ( 'NONE',  ( 43.28867513459483263, 170.7719333635740497, -7.904646289410545231E-15 ) ) ;
#3551 = CARTESIAN_POINT ( 'NONE',  ( 4.903702542908435547, 213.8346818373419751, 12.54886208192143826 ) ) ;
#3552 = EDGE_CURVE ( 'NONE', #20942, #5021, #26704, .T. ) ;
#3553 = CARTESIAN_POINT ( 'NONE',  ( -6.220909254589537696, 198.5229672870051161, 51.05113791807856671 ) ) ;
#3554 = CARTESIAN_POINT ( 'NONE',  ( 83.08867513459485110, 167.7597621252805880, -9.270509831248443078 ) ) ;
#3555 = PRODUCT_DEFINITION_SHAPE ( 'NONE', 'NONE',  #33711 ) ;
#3556 = CARTESIAN_POINT ( 'NONE',  ( 0.05014649552810505201, 217.5146222423826714, 37.25113791807855534 ) ) ;
#3557 = CARTESIAN_POINT ( 'NONE',  ( 82.87499999726878741, 138.6155565068815463, -3.929120461958505118E-15 ) ) ;
#3558 = SHAPE_DEFINITION_REPRESENTATION ( #12711, #19592 ) ;
#3559 = CARTESIAN_POINT ( 'NONE',  ( 0.05014649552828262524, 198.5883022060938572, 100.7488620819214304 ) ) ;
#3560 = CARTESIAN_POINT ( 'NONE',  ( 35.72499999726881015, 169.8198683612136222, 4.815267126137181997 ) ) ;
#3561 = CARTESIAN_POINT ( 'NONE',  ( 0.000000000000000000, 3.518949890710768802, -4.770489558936219510E-15 ) ) ;
#3562 = CARTESIAN_POINT ( 'NONE',  ( -4.000000000000000000, 4.898587196589412829E-16, -8.000000000000000000 ) ) ;
#3563 = CARTESIAN_POINT ( 'NONE',  ( -9.680171189290831535, 214.0920067884431148, 21.80113791807856671 ) ) ;
#3564 = CARTESIAN_POINT ( 'NONE',  ( 2.325424218458714165, -7.317669739337183898, -7.030005583191490715 ) ) ;
#3565 = CARTESIAN_POINT ( 'NONE',  ( 61.37499999726880873, 155.0000000000000000, -15.58253175000000823 ) ) ;
#3566 = CARTESIAN_POINT ( 'NONE',  ( 10.00000000000000711, 206.9523078486586201, 68.00113791807856956 ) ) ;
#3567 = CARTESIAN_POINT ( 'NONE',  ( 10.00000000000000711, 206.9523078486586201, 41.00113791807856956 ) ) ;
#3568 = DIRECTION ( 'NONE',  ( -1.000000000000000000, -0.000000000000000000, -0.000000000000000000 ) ) ;
#3569 = DIRECTION ( 'NONE',  ( -1.000000000000000000, 0.000000000000000000, -0.000000000000000000 ) ) ;
#3570 = CARTESIAN_POINT ( 'NONE',  ( -12.00000000000000711, 207.0476921513413515, 102.5011379180785696 ) ) ;
#3571 = CARTESIAN_POINT ( 'NONE',  ( -8.062137200540822946, 201.0835637161416400, 11.19886208192143506 ) ) ;
#3572 = CARTESIAN_POINT ( 'NONE',  ( 65.59999999453764019, 141.2096805137202580, -4.480746418436742040 ) ) ;
#3573 = EDGE_LOOP ( 'NONE', ( #31224, #24700, #29102 ) ) ;
#3574 = CARTESIAN_POINT ( 'NONE',  ( -7.375838497908182134, 217.2372850707499765, 45.95113791807857950 ) ) ;
#3575 = CARTESIAN_POINT ( 'NONE',  ( 2.426778023690261410, 199.3768101843759837, 65.60113791807857808 ) ) ;
#3576 = DIRECTION ( 'NONE',  ( 0.000000000000000000, 0.4999999999999993339, -0.8660254037844389297 ) ) ;
#3577 = CARTESIAN_POINT ( 'NONE',  ( 6.220909254589681581, 198.5229672870052582, 25.44886208192143684 ) ) ;
#3578 = CARTESIAN_POINT ( 'NONE',  ( 125.0000000000000000, 25.00000000000004619, -35.00000000000000000 ) ) ;
#3579 = EDGE_LOOP ( 'NONE', ( #32085, #32235, #28616 ) ) ;
#3580 = CARTESIAN_POINT ( 'NONE',  ( 3.044812012440130555, 197.4746971517856764, 83.60113791807857808 ) ) ;
#3581 = EDGE_LOOP ( 'NONE', ( #11425, #8446, #24878, #14814 ) ) ;
#3582 = DIRECTION ( 'NONE',  ( 1.000000000000000000, 0.000000000000000000, 0.000000000000000000 ) ) ;
#3583 = CYLINDRICAL_SURFACE ( 'NONE', #25243, 4.200000000000001954 ) ;
#3584 = ORIENTED_EDGE ( 'NONE', *, *, #29596, .T. ) ;
#3585 = CARTESIAN_POINT ( 'NONE',  ( 8.015496119326531499, 209.5516654185219636, 19.85113791807856387 ) ) ;
#3586 = CARTESIAN_POINT ( 'NONE',  ( -60.15281075484971041, 194.9558321103198466, 1.882765505879504309 ) ) ;
#3587 = CARTESIAN_POINT ( 'NONE',  ( -8.062137200540822946, 201.0835637161416400, 2.198862081921434175 ) ) ;
#3588 = CARTESIAN_POINT ( 'NONE',  ( 50.27499999726880731, 160.0630714827496206, 15.58253174999999224 ) ) ;
#3589 = ORIENTED_EDGE ( 'NONE', *, *, #6380, .F. ) ;
#3590 = CARTESIAN_POINT ( 'NONE',  ( 55.32499999726881157, 164.1591823560292198, -12.60653300113719766 ) ) ;
#3591 = CARTESIAN_POINT ( 'NONE',  ( 7.549006887134069643, -4.358421158401204032, -7.700127545397312367 ) ) ;
#3592 = CYLINDRICAL_SURFACE ( 'NONE', #4743, 5.000000000000000888 ) ;
#3593 = DIRECTION ( 'NONE',  ( 1.000000000000000000, 0.000000000000000000, 0.000000000000000000 ) ) ;
#3594 = CARTESIAN_POINT ( 'NONE',  ( -6.139770520408224463, 198.4640165459539389, 89.04886208192139918 ) ) ;
#3595 = CARTESIAN_POINT ( 'NONE',  ( 56.97499999726881015, 140.1801316387863778, -4.815267126137194431 ) ) ;
#3596 = CARTESIAN_POINT ( 'NONE',  ( -8.118202686958039038, 201.1607312380087080, 27.20113791807856884 ) ) ;
#3597 = DIRECTION ( 'NONE',  ( 0.000000000000000000, -1.000000000000000000, 0.000000000000000000 ) ) ;
#3598 = CARTESIAN_POINT ( 'NONE',  ( -9.680171189290716072, 199.9079932115567146, 77.19886208192143329 ) ) ;
#3599 = CIRCLE ( 'NONE', #21614, 97.99999999999997158 ) ;
#3600 = CARTESIAN_POINT ( 'NONE',  ( 72.20000000000001705, 142.6655632788954620, -8.961492836873480528 ) ) ;
#3601 = CARTESIAN_POINT ( 'NONE',  ( 62.41132485994282320, 167.7597621252805880, 9.270509831248428867 ) ) ;
#3602 = DIRECTION ( 'NONE',  ( 0.000000000000000000, 0.000000000000000000, -1.000000000000000000 ) ) ;
#3603 = CARTESIAN_POINT ( 'NONE',  ( -10.01549611932653860, 203.7984951890123284, 96.35113791807853545 ) ) ;
#3604 = CARTESIAN_POINT ( 'NONE',  ( 32.88867513459483405, 159.8737954434936057, -15.00000000000002665 ) ) ;
#3605 = CARTESIAN_POINT ( 'NONE',  ( 44.57499999726881157, 145.8408176439707802, 12.60653300113718345 ) ) ;
#3606 = CARTESIAN_POINT ( 'NONE',  ( -10.01549611932653860, 203.7984951890123284, 33.35113791807855677 ) ) ;
#3607 = AXIS2_PLACEMENT_3D ( 'NONE', #8665, #19390, #14111 ) ;
#3608 = CARTESIAN_POINT ( 'NONE',  ( 79.12499999726881583, 155.0000000000000000, -15.58253175000000823 ) ) ;
#3609 = ORIENTED_EDGE ( 'NONE', *, *, #9534, .F. ) ;
#3610 = CARTESIAN_POINT ( 'NONE',  ( 38.71132485994280614, 155.0000000000000000, 15.00000000000001243 ) ) ;
#3611 = CARTESIAN_POINT ( 'NONE',  ( 41.29999999453762172, 142.6655632788954620, 8.961492836873471646 ) ) ;
#3612 = CARTESIAN_POINT ( 'NONE',  ( 9.680171189290831535, 199.9079932115568852, 17.30113791807856671 ) ) ;
#3613 = DIRECTION ( 'NONE',  ( -1.000000000000000000, 0.000000000000000000, 0.000000000000000000 ) ) ;
#3614 = CARTESIAN_POINT ( 'NONE',  ( 3.749999999999999112, -6.495190528383302464, -6.991905250253757309 ) ) ;
#3615 = VERTEX_POINT ( 'NONE', #24599 ) ;
#3616 = CARTESIAN_POINT ( 'NONE',  ( 7.375838497908012492, 217.2372850707501186, 30.54886208192144181 ) ) ;
#3617 = CARTESIAN_POINT ( 'NONE',  ( -10.16981089642701974, 207.8187771357854103, 102.5476305063704814 ) ) ;
#3618 = CARTESIAN_POINT ( 'NONE',  ( -8.118202686958039038, 201.1607312380087080, 51.20113791807857240 ) ) ;
#3619 = ORIENTED_EDGE ( 'NONE', *, *, #23140, .T. ) ;
#3620 = CARTESIAN_POINT ( 'NONE',  ( 2.426778023690075337, 214.6231898156240447, 15.39886208192143613 ) ) ;
#3621 = AXIS2_PLACEMENT_3D ( 'NONE', #11749, #27088, #9530 ) ;
#3622 = UNCERTAINTY_MEASURE_WITH_UNIT (LENGTH_MEASURE( 1.000000000000000082E-05 ), #9632, 'distance_accuracy_value', 'NONE');
#3623 = CARTESIAN_POINT ( 'NONE',  ( 78.88867513459481984, 159.8737954434934636, -15.00000000000014566 ) ) ;
#3624 = VERTEX_POINT ( 'NONE', #21241 ) ;
#3625 = CARTESIAN_POINT ( 'NONE',  ( 2.517493886309087436, 199.4062855549015865, 100.5988620819214532 ) ) ;
#3626 = CARTESIAN_POINT ( 'NONE',  ( -2.426778023690262742, 214.6231898156240163, 43.10113791807857808 ) ) ;
#3627 = DIRECTION ( 'NONE',  ( 0.000000000000000000, 0.000000000000000000, 1.000000000000000000 ) ) ;
#3629 = EDGE_LOOP ( 'NONE', ( #398, #22472, #28449, #10571 ) ) ;
#3628 = AXIS2_PLACEMENT_3D ( 'NONE', #25975, #2812, #31427 ) ;
#3630 = CARTESIAN_POINT ( 'NONE',  ( 40.22499999726880304, 149.9369285172503510, 15.58253174999999580 ) ) ;
#3631 = CARTESIAN_POINT ( 'NONE',  ( 8.118202686958138514, 201.1607312380088501, 58.29886208192143471 ) ) ;
#3632 = CARTESIAN_POINT ( 'NONE',  ( 40.97499999726881725, 140.1801316387863778, -4.815267126137194431 ) ) ;
#3633 = DIRECTION ( 'NONE',  ( -0.000000000000000000, -0.000000000000000000, 1.000000000000000000 ) ) ;
#3634 = CARTESIAN_POINT ( 'NONE',  ( -6.500168698208129925, 202.3363017425936050, 99.20113791807858661 ) ) ;
#3635 = EDGE_CURVE ( 'NONE', #22495, #26131, #8923, .T. ) ;
#3636 = CARTESIAN_POINT ( 'NONE',  ( 56.39999999999999858, 150.2886644046228639, -14.50000000000000888 ) ) ;
#3637 = CARTESIAN_POINT ( 'NONE',  ( 7.984503880673422316, 209.6470497212048372, 75.84886208192143897 ) ) ;
#3638 = VECTOR ( 'NONE', #26653, 1000.000000000000000 ) ;
#3639 = DIRECTION ( 'NONE',  ( 0.000000000000000000, 0.000000000000000000, 1.000000000000000000 ) ) ;
#3640 = CARTESIAN_POINT ( 'NONE',  ( -10.00000000000000178, 206.7692714347156198, 108.3323677711372000 ) ) ;
#3641 = MECHANICAL_DESIGN_GEOMETRIC_PRESENTATION_REPRESENTATION (  '', ( #11264 ), #6367 ) ;
#3642 = CARTESIAN_POINT ( 'NONE',  ( 57.42499999726880588, 168.2552932293087906, -9.630534252274385310 ) ) ;
#3643 = STYLED_ITEM ( 'NONE', ( #24499 ), #672 ) ;
#3644 = CARTESIAN_POINT ( 'NONE',  ( 8.118202686958039038, 212.8392687619912635, 10.70113791807856529 ) ) ;
#3645 = CARTESIAN_POINT ( 'NONE',  ( 37.71132485994279904, 155.0000000000000000, -15.00000000000002487 ) ) ;
#3646 = CARTESIAN_POINT ( 'NONE',  ( 67.22499999726879594, 160.0630714827496206, -15.58253175000000823 ) ) ;
#3647 = CARTESIAN_POINT ( 'NONE',  ( 78.47499999726881015, 149.9369285172503510, 15.58253174999999580 ) ) ;
#3648 = CARTESIAN_POINT ( 'NONE',  ( -3.753561863808691168, 195.6020594897209435, 74.90113791807856103 ) ) ;
#3649 = CARTESIAN_POINT ( 'NONE',  ( -8.118202686958039038, 201.1607312380087080, 93.20113791807857240 ) ) ;
#3650 = FACE_OUTER_BOUND ( 'NONE', #25283, .T. ) ;
#3651 = AXIS2_PLACEMENT_3D ( 'NONE', #13719, #16614, #32294 ) ;
#3652 = ORIENTED_EDGE ( 'NONE', *, *, #30577, .T. ) ;
#3653 = CARTESIAN_POINT ( 'NONE',  ( -8.118202686958138514, 212.8392687619910930, 2.798862081921434708 ) ) ;
#3654 = CARTESIAN_POINT ( 'NONE',  ( 3.662846001189864698, 218.4274158808046593, 66.39886208192143613 ) ) ;
#3655 = CARTESIAN_POINT ( 'NONE',  ( -6.220909254589682469, 215.4770327129947134, 65.94886208192143329 ) ) ;
#3656 = CARTESIAN_POINT ( 'NONE',  ( 9.736236675708031640, 199.9851607334238963, 4.298862081921434708 ) ) ;
#3657 = CARTESIAN_POINT ( 'NONE',  ( -3.809068165403726614, -5.306386968807666804, -4.619717694324952472E-15 ) ) ;
#3658 = CARTESIAN_POINT ( 'NONE',  ( -10.00000000000000711, 207.0476921513413515, 24.50113791807856600 ) ) ;
#3659 = CARTESIAN_POINT ( 'NONE',  ( 8.062137200540822946, 212.9164362838583315, 90.69886208192143329 ) ) ;
#3660 = ORIENTED_EDGE ( 'NONE', *, *, #2325, .T. ) ;
#3661 = LINE ( 'NONE', #7590, #25185 ) ;
#3662 = ORIENTED_EDGE ( 'NONE', *, *, #2875, .T. ) ;
#3663 = CARTESIAN_POINT ( 'NONE',  ( -125.0000000000000000, -25.00000000000000000, 35.00000000000000000 ) ) ;
#3664 = CARTESIAN_POINT ( 'NONE',  ( 7.984503880673422316, 209.6470497212048372, 66.84886208192143897 ) ) ;
#3665 = CONICAL_SURFACE ( 'NONE', #8043, 31.00000000000000000, 1.466076571675243967 ) ;
#3666 = VERTEX_POINT ( 'NONE', #19484 ) ;
#3667 = CIRCLE ( 'NONE', #23258, 31.00000000000000000 ) ;
#3668 = CARTESIAN_POINT ( 'NONE',  ( 84.02499999726880731, 160.0630714827496206, 15.58253174999999224 ) ) ;
#3669 = VERTEX_POINT ( 'NONE', #15964 ) ;
#3670 = DIRECTION ( 'NONE',  ( 0.000000000000000000, 0.000000000000000000, -1.000000000000000000 ) ) ;
#3671 = CIRCLE ( 'NONE', #25983, 17.00000000000000355 ) ;
#3672 = CARTESIAN_POINT ( 'NONE',  ( 78.42499999726882720, 141.7447067706911810, 9.630534252274376428 ) ) ;
#3673 = CARTESIAN_POINT ( 'NONE',  ( 6.444103211791042618, 202.2591342207267644, 65.30113791807858092 ) ) ;
#3674 = DIRECTION ( 'NONE',  ( 0.000000000000000000, 0.000000000000000000, 1.000000000000000000 ) ) ;
#3675 = EDGE_CURVE ( 'NONE', #258, #20656, #18573, .T. ) ;
#3676 = VECTOR ( 'NONE', #7219, 1000.000000000000114 ) ;
#3677 = CARTESIAN_POINT ( 'NONE',  ( 35.59999999999998721, 150.2886644046228639, 14.49999999999999645 ) ) ;
#3678 = CARTESIAN_POINT ( 'NONE',  ( -8.000000000000008882, 206.9523078486584780, 47.49886208192144466 ) ) ;
#3679 = CARTESIAN_POINT ( 'NONE',  ( 0.05014649552810505201, 217.5146222423826714, 88.25113791807858377 ) ) ;
#3680 = CARTESIAN_POINT ( 'NONE',  ( -10.01549611932653860, 203.7984951890123284, 66.35113791807853545 ) ) ;
#3681 = EDGE_CURVE ( 'NONE', #320, #29326, #29049, .T. ) ;
#3682 = DIRECTION ( 'NONE',  ( 1.000000000000000000, 0.000000000000000000, 0.000000000000000000 ) ) ;
#3683 = CARTESIAN_POINT ( 'NONE',  ( 7.984503880673485376, 204.3529502787953902, 20.15113791807856458 ) ) ;
#3684 = CARTESIAN_POINT ( 'NONE',  ( -2.352990130084580066E-16, 8.660254037844390851, -7.422398894150034288 ) ) ;
#3685 = DIRECTION ( 'NONE',  ( 1.000000000000000000, 0.000000000000000000, 0.000000000000000000 ) ) ;
#3686 = CARTESIAN_POINT ( 'NONE',  ( 48.72499999726881725, 140.1801316387863778, -4.815267126137194431 ) ) ;
#3687 = CARTESIAN_POINT ( 'NONE',  ( 3.753561863808689836, 218.3979405102790565, 52.40113791807858235 ) ) ;
#3688 = LINE ( 'NONE', #31967, #11346 ) ;
#3689 = TOROIDAL_SURFACE ( 'NONE', #22746, 6.099999999999999645, 0.4000000000000000222 ) ;
#3690 = PRODUCT ( 'pad arm left_left', 'pad arm left_left', '', ( #9901 ) ) ;
#3691 = CARTESIAN_POINT ( 'NONE',  ( -9.984503880673473830, 210.2968891136704315, 93.65113791807857524 ) ) ;
#3692 = CARTESIAN_POINT ( 'NONE',  ( -10.01549611932653860, 203.7984951890123000, 66.35113791807856387 ) ) ;
#3693 = VECTOR ( 'NONE', #4424, 1000.000000000000000 ) ;
#3694 = VECTOR ( 'NONE', #17304, 1000.000000000000227 ) ;
#3695 = CARTESIAN_POINT ( 'NONE',  ( 12.01549611932659367, 203.1486557965466773, 37.14886208192143613 ) ) ;
#3696 = CARTESIAN_POINT ( 'NONE',  ( -10.01549611932659545, 210.2015048109875011, 41.64886208192144323 ) ) ;
#3697 = LINE ( 'NONE', #14254, #29237 ) ;
#3698 = CARTESIAN_POINT ( 'NONE',  ( -12.01549611932652972, 203.1486557965464499, 81.35113791807857808 ) ) ;
#3699 = CARTESIAN_POINT ( 'NONE',  ( 2.517493886308900919, 214.5937144450984420, 97.40113791807858945 ) ) ;
#3700 = ADVANCED_FACE ( 'NONE', ( #24769 ), #6027, .T. ) ;
#3701 = CARTESIAN_POINT ( 'NONE',  ( -8.118202686958138514, 212.8392687619910930, 59.79886208192143471 ) ) ;
#3702 = PRESENTATION_STYLE_ASSIGNMENT (( #6594 ) ) ;
#3703 = CIRCLE ( 'NONE', #5858, 6.500000000000000888 ) ;
#3704 = ORIENTED_EDGE ( 'NONE', *, *, #20300, .T. ) ;
#3705 = CARTESIAN_POINT ( 'NONE',  ( 7.456977232089471386, 196.8216656703012006, 64.44886208192143329 ) ) ;
#3706 = ORIENTED_EDGE ( 'NONE', *, *, #7107, .T. ) ;
#3707 = CARTESIAN_POINT ( 'NONE',  ( 73.47499999726878173, 160.0630714827496206, -15.58253175000000823 ) ) ;
#3708 = CARTESIAN_POINT ( 'NONE',  ( -4.984841277089891776, 213.7757310962905990, 44.94886208192144039 ) ) ;
#3709 = EDGE_CURVE ( 'NONE', #5646, #31059, #20736, .T. ) ;
#3710 = ORIENTED_EDGE ( 'NONE', *, *, #10798, .F. ) ;
#3711 = CARTESIAN_POINT ( 'NONE',  ( 83.27499999726880731, 149.9369285172503510, -15.58253175000000823 ) ) ;
#3712 = FACE_OUTER_BOUND ( 'NONE', #22728, .T. ) ;
#3713 = CARTESIAN_POINT ( 'NONE',  ( 107.0104235265664556, 155.0000000000000000, -11.99999999999998224 ) ) ;
#3714 = CARTESIAN_POINT ( 'NONE',  ( 6.444103211791042618, 202.2591342207267644, 53.30113791807858092 ) ) ;
#3715 = DIRECTION ( 'NONE',  ( 0.000000000000000000, 0.000000000000000000, -1.000000000000000000 ) ) ;
#3716 = AXIS2_PLACEMENT_3D ( 'NONE', #23498, #2731, #10399 ) ;
#3717 = CARTESIAN_POINT ( 'NONE',  ( 6.220909254589681581, 198.5229672870052582, 28.44886208192143684 ) ) ;
#3718 = CARTESIAN_POINT ( 'NONE',  ( 68.27499999726879309, 160.0630714827496206, 15.58253174999999224 ) ) ;
#3719 = VERTEX_POINT ( 'NONE', #23798 ) ;
#3720 = CARTESIAN_POINT ( 'NONE',  ( 41.48867513459482836, 167.7597621252805880, 9.270509831248428867 ) ) ;
#3721 =( NAMED_UNIT ( * ) SI_UNIT ( $, .STERADIAN. ) SOLID_ANGLE_UNIT ( ) );
#3722 = CARTESIAN_POINT ( 'NONE',  ( 2.000000000000000000, 0.8865213383406687075, -1.535500000000000975 ) ) ;
#3723 = FACE_OUTER_BOUND ( 'NONE', #11345, .T. ) ;
#3724 = CARTESIAN_POINT ( 'NONE',  ( -8.015496119326597224, 209.5516654185217362, 17.64886208192143968 ) ) ;
#3725 = CARTESIAN_POINT ( 'NONE',  ( 10.00000000000000711, 206.9523078486586201, 62.00113791807856956 ) ) ;
#3726 = CARTESIAN_POINT ( 'NONE',  ( -6.220909254589537696, 198.5229672870051161, 33.05113791807857382 ) ) ;
#3727 = CARTESIAN_POINT ( 'NONE',  ( 84.27499999726879309, 160.0630714827496206, 15.58253174999999402 ) ) ;
#3728 = VECTOR ( 'NONE', #6069, 1000.000000000000114 ) ;
#3729 = CARTESIAN_POINT ( 'NONE',  ( 4.903702542908601636, 200.1653181626581102, -0.5488620819214340418 ) ) ;
#3730 = CARTESIAN_POINT ( 'NONE',  ( 42.32499999726881157, 145.8408176439707802, 12.60653300113718345 ) ) ;
#3731 = CARTESIAN_POINT ( 'NONE',  ( 36.18867513459482410, 140.7341522555726669, 4.635254915624211769 ) ) ;
#3732 = DIRECTION ( 'NONE',  ( 1.000000000000000000, 0.000000000000000000, 0.000000000000000000 ) ) ;
#3733 = CARTESIAN_POINT ( 'NONE',  ( 11.98450388067348271, 203.0532714938637753, 20.15113791807856458 ) ) ;
#3734 = CARTESIAN_POINT ( 'NONE',  ( 6.486836893983020325, -4.915077010914103539, -7.231838333420563814 ) ) ;
#3735 = EDGE_CURVE ( 'NONE', #23334, #3461, #16406, .T. ) ;
#3736 = CARTESIAN_POINT ( 'NONE',  ( 6.220909254589536808, 215.4770327129947702, 67.55113791807853829 ) ) ;
#3737 = EDGE_CURVE ( 'NONE', #7925, #10430, #29432, .T. ) ;
#3738 = CARTESIAN_POINT ( 'NONE',  ( -6.139770520408368348, 215.5359834540460042, 42.95113791807856529 ) ) ;
#3739 = DIRECTION ( 'NONE',  ( -1.000000000000000000, -0.000000000000000000, -0.000000000000000000 ) ) ;
#3740 = CARTESIAN_POINT ( 'NONE',  ( 11.40740920524441115, 25.16819403002534727, -18.00000000000000000 ) ) ;
#3741 = CARTESIAN_POINT ( 'NONE',  ( 3.662846001189864698, 218.4274158808046593, 3.398862081921433909 ) ) ;
#3742 = CARTESIAN_POINT ( 'NONE',  ( 10.00000000000000711, 207.0476921513415220, 9.998862081921435774 ) ) ;
#3743 = CARTESIAN_POINT ( 'NONE',  ( 66.89999999453763735, 159.7113355953771077, 14.49999999999999289 ) ) ;
#3744 = ORIENTED_EDGE ( 'NONE', *, *, #8275, .T. ) ;
#3745 = CARTESIAN_POINT ( 'NONE',  ( 7.456977232089302632, 217.1783343296989131, 49.55113791807856671 ) ) ;
#3746 = AXIS2_PLACEMENT_3D ( 'NONE', #31280, #33662, #7940 ) ;
#3747 = CARTESIAN_POINT ( 'NONE',  ( -2.426778023690262742, 214.6231898156240163, 70.10113791807857808 ) ) ;
#3748 = EDGE_CURVE ( 'NONE', #6526, #30462, #26178, .T. ) ;
#3749 = CARTESIAN_POINT ( 'NONE',  ( 73.78867513459483973, 155.0000000000000000, 15.00000000000001243 ) ) ;
#3750 = CARTESIAN_POINT ( 'NONE',  ( 10.01549611932659545, 203.7984951890123853, 28.14886208192143613 ) ) ;
#3751 = CARTESIAN_POINT ( 'NONE',  ( 4.639619758716984954, -4.826867782832383824, -0.1499059597315342829 ) ) ;
#3752 = ORIENTED_EDGE ( 'NONE', *, *, #13352, .F. ) ;
#3753 = VECTOR ( 'NONE', #32543, 1000.000000000000000 ) ;
#3754 = CARTESIAN_POINT ( 'NONE',  ( 0.05014649552810505201, 217.5146222423826714, 79.25113791807856956 ) ) ;
#3755 = ADVANCED_FACE ( 'NONE', ( #21863, #5412, #3980, #32256, #298, #28753, #27155, #26188, #23639, #21076 ), #8146, .F. ) ;
#3756 = ORIENTED_EDGE ( 'NONE', *, *, #13315, .T. ) ;
#3757 = APPLICATION_CONTEXT ( 'automotive_design' ) ;
#3758 = CARTESIAN_POINT ( 'NONE',  ( 49.71132485994280614, 155.0000000000000000, -15.00000000000002487 ) ) ;
#3759 = CARTESIAN_POINT ( 'NONE',  ( 0.5725525826504702653, 3.710888496608923059, -2.778243469714884117 ) ) ;
#3760 = ORIENTED_EDGE ( 'NONE', *, *, #1899, .F. ) ;
#3761 = CARTESIAN_POINT ( 'NONE',  ( 8.000000000000008882, 206.9523078486586485, 26.00113791807856600 ) ) ;
#3762 = CARTESIAN_POINT ( 'NONE',  ( -67.50000000000000000, 0.000000000000000000, -17.00000000000001421 ) ) ;
#3763 = CARTESIAN_POINT ( 'NONE',  ( -6.220909254589682469, 215.4770327129946850, 8.948862081921435063 ) ) ;
#3764 = CARTESIAN_POINT ( 'NONE',  ( 49.37499999726880873, 155.0000000000000000, -15.58253175000000823 ) ) ;
#3765 = ORIENTED_EDGE ( 'NONE', *, *, #2478, .F. ) ;
#3766 = CARTESIAN_POINT ( 'NONE',  ( 56.22499999726881015, 149.9369285172503510, 15.58253174999999580 ) ) ;
#3767 = CARTESIAN_POINT ( 'NONE',  ( 8.015496119326531499, 209.5516654185219636, 52.85113791807857098 ) ) ;
#3768 = PLANE ( 'NONE',  #6907 ) ;
#3769 = FILL_AREA_STYLE ('',( #27108 ) ) ;
#3770 = CARTESIAN_POINT ( 'NONE',  ( -25.25067902531499442, 17.17577847294295523, -1.706427272390161454 ) ) ;
#3771 = AXIS2_PLACEMENT_3D ( 'NONE', #1393, #29678, #11783 ) ;
#3772 = CARTESIAN_POINT ( 'NONE',  ( -3.135527875058982783, 216.4958274776886924, 90.09886208192143897 ) ) ;
#3773 = CARTESIAN_POINT ( 'NONE',  ( 60.57499999726881157, 145.8408176439707802, 12.60653300113718345 ) ) ;
#3774 = CARTESIAN_POINT ( 'NONE',  ( 9.984503880673470277, 203.7031108863295401, 20.15113791807856813 ) ) ;
#3775 = CARTESIAN_POINT ( 'NONE',  ( 73.48867513459482836, 167.7597621252805880, 9.270509831248428867 ) ) ;
#3776 = CARTESIAN_POINT ( 'NONE',  ( 7.375838497908012492, 217.2372850707501186, 78.54886208192142760 ) ) ;
#3777 = CARTESIAN_POINT ( 'NONE',  ( 82.69999999999998863, 163.5228861582408797, -11.73074641843674470 ) ) ;
#3778 = DIRECTION ( 'NONE',  ( 1.000000000000000000, -0.000000000000000000, -0.000000000000000000 ) ) ;
#3779 = CARTESIAN_POINT ( 'NONE',  ( -5.416666666666670515, 4.378239541354659536, -5.848636054922036642 ) ) ;
#3780 = CARTESIAN_POINT ( 'NONE',  ( -10.01549611932653860, 203.7984951890123284, 93.35113791807857808 ) ) ;
#3781 = CARTESIAN_POINT ( 'NONE',  ( 60.00000000000000000, 7.347880794884118356E-15, 35.00000000000000000 ) ) ;
#3782 = CARTESIAN_POINT ( 'NONE',  ( 46.57499999726881157, 145.8408176439707802, 12.60653300113718345 ) ) ;
#3783 = CARTESIAN_POINT ( 'NONE',  ( -9.984503880673473830, 210.2968891136704315, 39.65113791807857524 ) ) ;
#3784 = EDGE_CURVE ( 'NONE', #4076, #18960, #30535, .T. ) ;
#3785 = CARTESIAN_POINT ( 'NONE',  ( 75.72499999726881015, 169.8198683612136222, 4.815267126137181997 ) ) ;
#3786 = EDGE_LOOP ( 'NONE', ( #21693, #360, #32034, #18428 ) ) ;
#3787 = CARTESIAN_POINT ( 'NONE',  ( 51.91132485994280898, 163.8167787843871110, -12.13525491562423397 ) ) ;
#3788 = CARTESIAN_POINT ( 'NONE',  ( 49.19999999453762740, 146.4771138417591203, 11.73074641843673227 ) ) ;
#3789 =( BOUNDED_CURVE ( )  B_SPLINE_CURVE ( 2, ( #28884, #23443, #10670, #6975, #108, #18500, #7322, #12419, #4749, #22813, #17362 ),
 .UNSPECIFIED., .F., .F. ) 
 B_SPLINE_CURVE_WITH_KNOTS ( ( 3, 2, 2, 2, 2, 3 ),
 ( 0.9285714285714283811, 0.9321428571428569398, 0.9357142857142856096, 0.9392857142857141683, 0.9428571428571427271, 0.9464285714285712858 ),
 .UNSPECIFIED. ) 
 CURVE ( )  GEOMETRIC_REPRESENTATION_ITEM ( )  RATIONAL_B_SPLINE_CURVE ( ( 1.000000000000001554, 0.9510565162951518658, 1.000000000000000000, 0.9510565162951534202, 1.000000000000000000, 0.9510565162951534202, 1.000000000000000000, 0.9510565162951534202, 1.000000000000000000, 0.9510565162951549745, 0.9999999999999984457 ) ) 
 REPRESENTATION_ITEM ( '' )  );
#3790 = CARTESIAN_POINT ( 'NONE',  ( -7.375838497908182134, 217.2372850707499765, 18.95113791807856529 ) ) ;
#3791 = CARTESIAN_POINT ( 'NONE',  ( -11.00000000000000355, 206.9999999999998863, 103.5000000000000142 ) ) ;
#3792 = CARTESIAN_POINT ( 'NONE',  ( -65.50384660342780307, 120.9385549553365706, 18.99615339657220758 ) ) ;
#3793 = EDGE_LOOP ( 'NONE', ( #21926, #28936 ) ) ;
#3794 = CARTESIAN_POINT ( 'NONE',  ( -3.662846001189865142, 195.5725841191952838, 46.89886208192143613 ) ) ;
#3795 = CARTESIAN_POINT ( 'NONE',  ( -7.897836333153808397, -1.530409084195006653, -7.633857274177628938 ) ) ;
#3796 = AXIS2_PLACEMENT_3D ( 'NONE', #21965, #24857, #19908 ) ;
#3797 = CARTESIAN_POINT ( 'NONE',  ( 0.05014649552810505201, 217.5146222423826714, 49.25113791807857666 ) ) ;
#3798 = CARTESIAN_POINT ( 'NONE',  ( -2.426778023690076225, 199.3768101843759553, 13.89886208192143613 ) ) ;
#3799 = DIRECTION ( 'NONE',  ( 0.000000000000000000, 0.000000000000000000, 1.000000000000000000 ) ) ;
#3800 = ORIENTED_EDGE ( 'NONE', *, *, #20647, .T. ) ;
#3801 = CARTESIAN_POINT ( 'NONE',  ( -7.984503880673422316, 204.3529502787951628, 104.3488620819214532 ) ) ;
#3802 = DIRECTION ( 'NONE',  ( 0.000000000000000000, 0.000000000000000000, -1.000000000000000000 ) ) ;
#3803 = CARTESIAN_POINT ( 'NONE',  ( -7.984503880673488041, 209.6470497212046098, 36.65113791807856103 ) ) ;
#3804 = DIRECTION ( 'NONE',  ( 1.000000000000000000, 0.000000000000000000, 0.000000000000000000 ) ) ;
#3805 = ORIENTED_EDGE ( 'NONE', *, *, #29067, .T. ) ;
#3806 = CARTESIAN_POINT ( 'NONE',  ( 40.92499999726881299, 145.8408176439707802, -12.60653300113719588 ) ) ;
#3807 = CARTESIAN_POINT ( 'NONE',  ( -3.135527875058982783, 216.4958274776886924, 57.09886208192143187 ) ) ;
#3808 = CARTESIAN_POINT ( 'NONE',  ( 43.27499999726880020, 149.9369285172503510, -15.58253175000000823 ) ) ;
#3809 = DIRECTION ( 'NONE',  ( 0.000000000000000000, 0.000000000000000000, 1.000000000000000000 ) ) ;
#3810 = CARTESIAN_POINT ( 'NONE',  ( 8.015496119326531499, 209.5516654185219636, 97.85113791807857808 ) ) ;
#3811 = CARTESIAN_POINT ( 'NONE',  ( 57.30000000000000426, 163.5228861582408797, 11.73074641843673049 ) ) ;
#3812 = CARTESIAN_POINT ( 'NONE',  ( 4.984841277089891776, 200.2242689037093726, 73.44886208192143329 ) ) ;
#3813 = CARTESIAN_POINT ( 'NONE',  ( -125.0000000000000000, -95.00000000000000000, -20.00000000000000000 ) ) ;
#3814 = DIRECTION ( 'NONE',  ( 0.000000000000000000, 0.000000000000000000, 1.000000000000000000 ) ) ;
#3815 = CARTESIAN_POINT ( 'NONE',  ( 59.22499999726879594, 160.0630714827496206, -15.58253175000000823 ) ) ;
#3817 = EDGE_LOOP ( 'NONE', ( #15149, #11920, #30667 ) ) ;
#3816 = CARTESIAN_POINT ( 'NONE',  ( 8.118202686958039038, 212.8392687619912635, 22.70113791807856884 ) ) ;
#3818 = DIRECTION ( 'NONE',  ( 0.000000000000000000, -0.04769215134144031559, 0.9988620819214357738 ) ) ;
#3819 = CARTESIAN_POINT ( 'NONE',  ( 82.27499999726880731, 160.0630714827496206, 15.58253174999999402 ) ) ;
#3820 = CARTESIAN_POINT ( 'NONE',  ( -12.01549611932652972, 203.1486557965464499, 84.35113791807857808 ) ) ;
#3821 = CARTESIAN_POINT ( 'NONE',  ( -3.135527875058821579, 197.5041725223112223, 92.90113791807857524 ) ) ;
#3822 = DIRECTION ( 'NONE',  ( 0.000000000000000000, 0.000000000000000000, 1.000000000000000000 ) ) ;
#3823 = VERTEX_POINT ( 'NONE', #30731 ) ;
#3824 = CARTESIAN_POINT ( 'NONE',  ( -0.05014649552828442242, 219.6175466908591716, 102.2488620819214447 ) ) ;
#3825 = CARTESIAN_POINT ( 'NONE',  ( 7.375838497908012492, 217.2372850707501186, 63.54886208192144181 ) ) ;
#3826 = CARTESIAN_POINT ( 'NONE',  ( -10.01549611932659545, 210.2015048109875011, 80.64886208192145034 ) ) ;
#3827 = CARTESIAN_POINT ( 'NONE',  ( -9.736236675708031640, 214.0148392665760753, 5.798862081921434708 ) ) ;
#3828 = DIRECTION ( 'NONE',  ( -0.000000000000000000, -0.000000000000000000, 1.000000000000000000 ) ) ;
#3829 = CARTESIAN_POINT ( 'NONE',  ( 8.118202686958039038, 212.8392687619912635, 22.70113791807856884 ) ) ;
#3830 = CARTESIAN_POINT ( 'NONE',  ( 10.01549611932659545, 203.7984951890123853, 85.14886208192143613 ) ) ;
#3831 = ADVANCED_FACE ( 'NONE', ( #4828 ), #1595, .T. ) ;
#3832 = VERTEX_POINT ( 'NONE', #1757 ) ;
#3833 = CARTESIAN_POINT ( 'NONE',  ( -67.50000599999999906, 155.0000000000000000, -17.00000000000000711 ) ) ;
#3834 = VERTEX_POINT ( 'NONE', #30389 ) ;
#3835 = CARTESIAN_POINT ( 'NONE',  ( -1.083333333333333037, -6.880090707843053544, -5.848636054922041083 ) ) ;
#3836 = CARTESIAN_POINT ( 'NONE',  ( -7.984503880673422316, 204.3529502787951628, 74.34886208192142476 ) ) ;
#3837 = ORIENTED_EDGE ( 'NONE', *, *, #3748, .T. ) ;
#3838 = PRODUCT_DEFINITION_SHAPE ( 'NONE', 'NONE',  #33719 ) ;
#3839 = CARTESIAN_POINT ( 'NONE',  ( 84.72499999726882436, 140.1801316387863778, -4.815267126137194431 ) ) ;
#3840 = ORIENTED_EDGE ( 'NONE', *, *, #17060, .T. ) ;
#3841 = CARTESIAN_POINT ( 'NONE',  ( -125.0000000000000000, 0.000000000000000000, 20.00000000000000000 ) ) ;
#3842 = CARTESIAN_POINT ( 'NONE',  ( 75.72499999726881015, 169.8198683612136222, 4.815267126137181997 ) ) ;
#3843 = CARTESIAN_POINT ( 'NONE',  ( 8.015496119326531499, 209.5516654185219636, 70.85113791807857808 ) ) ;
#3844 = CARTESIAN_POINT ( 'NONE',  ( 3.750000000000004441, -6.495190528383289141, 0.000000000000000000 ) ) ;
#3845 = AXIS2_PLACEMENT_3D ( 'NONE', #20780, #31179, #18234 ) ;
#3846 = CARTESIAN_POINT ( 'NONE',  ( 33.40000000000000568, 159.7113355953771077, 14.49999999999999289 ) ) ;
#3847 = CARTESIAN_POINT ( 'NONE',  ( -2.517493886309087880, 214.5937144450984135, 48.09886208192143897 ) ) ;
#3848 = CARTESIAN_POINT ( 'NONE',  ( 10.00000000000000711, 206.9523078486586201, 92.00113791807858377 ) ) ;
#3849 = CARTESIAN_POINT ( 'NONE',  ( -8.118202686958039038, 201.1607312380087080, 72.20113791807857240 ) ) ;
#3850 = CARTESIAN_POINT ( 'NONE',  ( 77.50000000000000000, 155.0000000000000000, -6.938893903907228378E-15 ) ) ;
#3851 = PLANE ( 'NONE',  #6445 ) ;
#3852 = DIRECTION ( 'NONE',  ( -1.000000000000000000, 3.552713678800500929E-15, 0.000000000000000000 ) ) ;
#3853 = CARTESIAN_POINT ( 'NONE',  ( 50.82499999726880446, 141.7447067706911810, -9.630534252274387086 ) ) ;
#3854 = CARTESIAN_POINT ( 'NONE',  ( 7.456977232089302632, 217.1783343296989131, 46.55113791807856671 ) ) ;
#3855 = CARTESIAN_POINT ( 'NONE',  ( 41.31132485994280756, 140.7341522555726669, -4.635254915624220651 ) ) ;
#3856 = CARTESIAN_POINT ( 'NONE',  ( -3.753561863808691168, 195.6020594897209435, -0.09886208192143448870 ) ) ;
#3857 = CARTESIAN_POINT ( 'NONE',  ( -8.118202686958039038, 201.1607312380087080, 72.20113791807857240 ) ) ;
#3858 = CARTESIAN_POINT ( 'NONE',  ( -3.662846001189865142, 195.5725841191952838, 28.89886208192143613 ) ) ;
#3859 = CARTESIAN_POINT ( 'NONE',  ( 3.135527875058981895, 197.5041725223112792, 43.59886208192143897 ) ) ;
#3860 = CARTESIAN_POINT ( 'NONE',  ( 88.89999999453763735, 159.7113355953771077, 14.49999999999999289 ) ) ;
#3861 = CARTESIAN_POINT ( 'NONE',  ( 0.05014649552807549926, 219.6175466908591716, 79.25113791807856956 ) ) ;
#3862 = CARTESIAN_POINT ( 'NONE',  ( -4.984841277089726574, 200.2242689037092305, 102.0511379180785809 ) ) ;
#3863 = CARTESIAN_POINT ( 'NONE',  ( 8.118202686958138514, 201.1607312380088501, 64.29886208192144181 ) ) ;
#3864 = EDGE_CURVE ( 'NONE', #16396, #33645, #19927, .T. ) ;
#3865 = CARTESIAN_POINT ( 'NONE',  ( 2.000000000000000000, -0.8865213383406721492, -1.535499999999998977 ) ) ;
#3866 = ORIENTED_EDGE ( 'NONE', *, *, #15173, .F. ) ;
#3867 = CARTESIAN_POINT ( 'NONE',  ( -9.736236675708031640, 214.0148392665760753, 62.79886208192144892 ) ) ;
#3868 = AXIS2_PLACEMENT_3D ( 'NONE', #14876, #17772, #6874 ) ;
#3869 = EDGE_LOOP ( 'NONE', ( #22538, #19080, #7962, #23492 ) ) ;
#3870 = CARTESIAN_POINT ( 'NONE',  ( 74.57499999726881867, 145.8408176439707802, 12.60653300113718345 ) ) ;
#3871 = CARTESIAN_POINT ( 'NONE',  ( 6.444103211790928043, 211.7408657792734061, 45.69886208192144750 ) ) ;
#3872 = VERTEX_POINT ( 'NONE', #33108 ) ;
#3873 = CARTESIAN_POINT ( 'NONE',  ( 80.67499999726882720, 141.7447067706911810, 9.630534252274376428 ) ) ;
#3874 = DIRECTION ( 'NONE',  ( 0.000000000000000000, 0.000000000000000000, -1.000000000000000000 ) ) ;
#3875 = EDGE_CURVE ( 'NONE', #2728, #26702, #9594, .T. ) ;
#3876 = CARTESIAN_POINT ( 'NONE',  ( -9.000000000000001776, 206.9999999999998863, 103.5000000000000426 ) ) ;
#3877 = CARTESIAN_POINT ( 'NONE',  ( 2.517493886308900919, 214.5937144450984420, 55.40113791807858235 ) ) ;
#3878 = CARTESIAN_POINT ( 'NONE',  ( -6.139770520408224463, 198.4640165459539389, 29.04886208192143471 ) ) ;
#3879 = CARTESIAN_POINT ( 'NONE',  ( 68.07499999726881867, 168.2552932293087906, 9.630534252274372875 ) ) ;
#3880 = ORIENTED_EDGE ( 'NONE', *, *, #574, .F. ) ;
#3881 = CARTESIAN_POINT ( 'NONE',  ( 105.0134430565187387, 155.0000000000000000, 0.000000000000000000 ) ) ;
#3882 = EDGE_CURVE ( 'NONE', #33037, #25104, #13144, .T. ) ;
#3883 = FACE_OUTER_BOUND ( 'NONE', #31828, .T. ) ;
#3884 = CARTESIAN_POINT ( 'NONE',  ( -6.500168698208244500, 211.6636982574061676, 14.79886208192143471 ) ) ;
#3885 = CARTESIAN_POINT ( 'NONE',  ( -3.044812012440131443, 216.5253028482142952, 61.10113791807857098 ) ) ;
#3886 = CARTESIAN_POINT ( 'NONE',  ( 9.984503880673470277, 203.7031108863295401, 35.15113791807856813 ) ) ;
#3887 = DIRECTION ( 'NONE',  ( -0.5773502691896268413, 0.5773502691896268413, -0.5773502691896235106 ) ) ;
#3888 = CARTESIAN_POINT ( 'NONE',  ( -4.903702542908436435, 200.1653181626580249, 98.04886208192144181 ) ) ;
#3889 = CARTESIAN_POINT ( 'NONE',  ( 46.32499999726881157, 145.8408176439707802, 12.60653300113718345 ) ) ;
#3890 = CARTESIAN_POINT ( 'NONE',  ( 95.59906517536109050, 155.0000000000000000, 0.000000000000000000 ) ) ;
#3891 = CARTESIAN_POINT ( 'NONE',  ( 33.52499999726880731, 169.8198683612136222, -4.815267126137197984 ) ) ;
#3892 = CARTESIAN_POINT ( 'NONE',  ( 9.680171189290831535, 199.9079932115568852, 20.30113791807857027 ) ) ;
#3893 = LINE ( 'NONE', #22628, #30394 ) ;
#3894 = EDGE_CURVE ( 'NONE', #10681, #3823, #25105, .T. ) ;
#3895 = CARTESIAN_POINT ( 'NONE',  ( -10.00000000000000711, 207.0476921513413515, 63.50113791807856956 ) ) ;
#3896 = CARTESIAN_POINT ( 'NONE',  ( -6.220909254589537696, 198.5229672870051445, 42.05113791807857382 ) ) ;
#3897 = DIRECTION ( 'NONE',  ( 1.000000000000000000, 0.000000000000000000, 0.000000000000000000 ) ) ;
#3898 = DIRECTION ( 'NONE',  ( -0.000000000000000000, -0.000000000000000000, 1.000000000000000000 ) ) ;
#3899 = CARTESIAN_POINT ( 'NONE',  ( 3.753561863808876797, 195.6020594897209719, 4.598862081921434530 ) ) ;
#3900 = CARTESIAN_POINT ( 'NONE',  ( 6.139770520408223575, 215.5359834540460611, 12.54886208192143648 ) ) ;
#3901 = CARTESIAN_POINT ( 'NONE',  ( 69.89999999453762314, 150.2886644046228639, -14.50000000000000888 ) ) ;
#3902 = VECTOR ( 'NONE', #17593, 1000.000000000000114 ) ;
#3903 = ORIENTED_EDGE ( 'NONE', *, *, #15621, .F. ) ;
#3904 = CARTESIAN_POINT ( 'NONE',  ( 7.456977232089302632, 217.1783343296989131, 46.55113791807856671 ) ) ;
#3905 = CARTESIAN_POINT ( 'NONE',  ( -8.000000000000008882, 207.0476921513413515, 72.50113791807856956 ) ) ;
#3906 = CARTESIAN_POINT ( 'NONE',  ( 0.05014649552828275708, 196.4853777576173002, 34.74886208192143044 ) ) ;
#3907 = ADVANCED_FACE ( 'NONE', ( #2275 ), #26203, .T. ) ;
#3908 = CARTESIAN_POINT ( 'NONE',  ( -64.50000000000000000, 2.605762844159070557, 20.00000000000000000 ) ) ;
#3909 = EDGE_LOOP ( 'NONE', ( #27508, #11386, #9455, #19595 ) ) ;
#3910 = CARTESIAN_POINT ( 'NONE',  ( -3.044812012440131443, 216.5253028482142952, 88.10113791807857808 ) ) ;
#3911 = ORIENTED_EDGE ( 'NONE', *, *, #9591, .F. ) ;
#3912 = CARTESIAN_POINT ( 'NONE',  ( 41.98867513459482126, 146.1832212156128890, 12.13525491562421976 ) ) ;
#3913 = FACE_OUTER_BOUND ( 'NONE', #13666, .T. ) ;
#3914 = VECTOR ( 'NONE', #5288, 1000.000000000000114 ) ;
#3915 = EDGE_LOOP ( 'NONE', ( #2246, #28577, #22269, #2127, #652 ) ) ;
#3916 = CARTESIAN_POINT ( 'NONE',  ( -2.517493886308901807, 199.4062855549015012, 23.90113791807857169 ) ) ;
#3917 =( BOUNDED_CURVE ( )  B_SPLINE_CURVE ( 2, ( #16547, #21826, #26942, #31883, #8392, #27116, #8550, #3601, #16882, #13655, #11447 ),
 .UNSPECIFIED., .F., .T. ) 
 B_SPLINE_CURVE_WITH_KNOTS ( ( 3, 2, 2, 2, 2, 3 ),
 ( 0.5000000000000000000, 0.5035714285714285587, 0.5071428571428571175, 0.5107142857142856762, 0.5142857142857142350, 0.5178571428571429047 ),
 .UNSPECIFIED. ) 
 CURVE ( )  GEOMETRIC_REPRESENTATION_ITEM ( )  RATIONAL_B_SPLINE_CURVE ( ( 1.000000000000000000, 0.9510565162951534202, 1.000000000000000000, 0.9510565162951534202, 1.000000000000000000, 0.9510565162951534202, 1.000000000000000000, 0.9510565162951534202, 1.000000000000000000, 0.9510565162951534202, 1.000000000000000000 ) ) 
 REPRESENTATION_ITEM ( '' )  );
#3918 = EDGE_CURVE ( 'NONE', #29444, #8938, #22718, .T. ) ;
#3919 = CARTESIAN_POINT ( 'NONE',  ( 125.5000000000000000, 48.99999999999998579, -2.149999999999999023 ) ) ;
#3920 = CARTESIAN_POINT ( 'NONE',  ( 3.753561863808876797, 195.6020594897209719, 103.5988620819214532 ) ) ;
#3921 = CARTESIAN_POINT ( 'NONE',  ( 52.87499999726880162, 138.6155565068815747, -3.929120461958505118E-15 ) ) ;
#3922 = ORIENTED_EDGE ( 'NONE', *, *, #405, .F. ) ;
#3923 = CARTESIAN_POINT ( 'NONE',  ( 6.500168698208129925, 211.6636982574063381, 46.70113791807857240 ) ) ;
#3924 = CARTESIAN_POINT ( 'NONE',  ( 67.31132485994281467, 140.7341522555726669, -4.635254915624220651 ) ) ;
#3925 = CIRCLE ( 'NONE', #14822, 31.00000000000000000 ) ;
#3926 =( LENGTH_UNIT ( ) NAMED_UNIT ( * ) SI_UNIT ( .MILLI., .METRE. ) );
#3927 = DIRECTION ( 'NONE',  ( 1.000000000000000000, 0.000000000000000000, 0.000000000000000000 ) ) ;
#3928 = CARTESIAN_POINT ( 'NONE',  ( -6.139770520408224463, 198.4640165459539389, 95.04886208192144181 ) ) ;
#3929 = AXIS2_PLACEMENT_3D ( 'NONE', #14507, #29858, #32733 ) ;
#3930 = CARTESIAN_POINT ( 'NONE',  ( 59.37499999726881583, 155.0000000000000000, -15.58253175000000823 ) ) ;
#3931 = CARTESIAN_POINT ( 'NONE',  ( -9.984503880673473830, 210.2968891136704315, 33.65113791807856813 ) ) ;
#3932 = CARTESIAN_POINT ( 'NONE',  ( -60.00000000000000000, -7.347880794884118356E-15, 35.00000000000000000 ) ) ;
#3933 = ADVANCED_FACE ( 'NONE', ( #15045 ), #19988, .T. ) ;
#3934 = CARTESIAN_POINT ( 'NONE',  ( 9.736236675708031640, 199.9851607334238963, 82.29886208192144181 ) ) ;
#3935 = CARTESIAN_POINT ( 'NONE',  ( 83.40000000000000568, 159.7113355953771077, 14.49999999999999289 ) ) ;
#3936 = CARTESIAN_POINT ( 'NONE',  ( -60.00000000000000000, -7.347880794884118356E-15, 35.00000000000000000 ) ) ;
#3937 = CARTESIAN_POINT ( 'NONE',  ( 115.4999999999999858, 155.0000000000000000, -6.938893903907228378E-15 ) ) ;
#3938 = CARTESIAN_POINT ( 'NONE',  ( -10.01549611932653860, 203.7984951890123284, 99.35113791807857808 ) ) ;
#3939 = CYLINDRICAL_SURFACE ( 'NONE', #8080, 2.149999999999994138 ) ;
#3940 = CARTESIAN_POINT ( 'NONE',  ( 45.97499999726881015, 169.8198683612136222, 4.815267126137181997 ) ) ;
#3941 = CARTESIAN_POINT ( 'NONE',  ( 9.984503880673470277, 203.7031108863295401, 38.15113791807856813 ) ) ;
#3942 = CARTESIAN_POINT ( 'NONE',  ( 85.32499999726880446, 164.1591823560292198, -12.60653300113719766 ) ) ;
#3943 = EDGE_LOOP ( 'NONE', ( #17067, #28863, #22437, #15523, #24825, #17233 ) ) ;
#3944 =( GEOMETRIC_REPRESENTATION_CONTEXT ( 3 ) GLOBAL_UNCERTAINTY_ASSIGNED_CONTEXT ( ( #11468 ) ) GLOBAL_UNIT_ASSIGNED_CONTEXT ( ( #13039, #264, #33654 ) ) REPRESENTATION_CONTEXT ( 'NONE', 'WORKASPACE' ) );
#3945 = CARTESIAN_POINT ( 'NONE',  ( -64.50000000000000000, -2.605762844159085212, -20.00000000000000000 ) ) ;
#3946 = DIRECTION ( 'NONE',  ( 1.000000000000000000, 0.000000000000000000, 0.000000000000000000 ) ) ;
#3947 = CARTESIAN_POINT ( 'NONE',  ( 47.49999999453763166, 139.7537977485451393, -4.138211985947621020E-15 ) ) ;
#3948 = CARTESIAN_POINT ( 'NONE',  ( 7.456977232089302632, 217.1783343296989131, 19.55113791807856671 ) ) ;
#3949 = DIRECTION ( 'NONE',  ( -0.8660254037844382635, -0.5000000000000006661, 0.000000000000000000 ) ) ;
#3950 = CARTESIAN_POINT ( 'NONE',  ( -9.826090958526812358, 208.0352956435529563, 102.7846294209004441 ) ) ;
#3951 = VERTEX_POINT ( 'NONE', #12156 ) ;
#3952 = CIRCLE ( 'NONE', #23003, 13.00000000000003908 ) ;
#3953 = CARTESIAN_POINT ( 'NONE',  ( -9.736236675708031640, 214.0148392665760753, 44.79886208192143471 ) ) ;
#3954 = CARTESIAN_POINT ( 'NONE',  ( 6.139770520408368348, 198.4640165459539674, 5.451137918078567068 ) ) ;
#3955 = CARTESIAN_POINT ( 'NONE',  ( 9.984503880673470277, 203.7031108863295401, 56.15113791807856103 ) ) ;
#3956 = VECTOR ( 'NONE', #13183, 1000.000000000000000 ) ;
#3957 = CARTESIAN_POINT ( 'NONE',  ( 4.984841277089891776, 200.2242689037093726, 10.44886208192143506 ) ) ;
#3958 = B_SPLINE_CURVE_WITH_KNOTS ( 'NONE', 3,
 ( #12618, #33410, #23359, #31192, #18243, #28632 ),
 .UNSPECIFIED., .F., .F.,
 ( 4, 2, 4 ),
 ( 2.475503369207376426E-07, 0.002222330217055627170, 0.004444412883774334112 ),
 .UNSPECIFIED. ) ;
#3959 = PRODUCT_DEFINITION_CONTEXT ( 'detailed design', #25297, 'design' ) ;
#3960 = CARTESIAN_POINT ( 'NONE',  ( 50.91132485994280188, 146.1832212156128890, 12.13525491562421976 ) ) ;
#3961 = ORIENTED_EDGE ( 'NONE', *, *, #7063, .T. ) ;
#3962 = CARTESIAN_POINT ( 'NONE',  ( 7.984503880673422316, 209.6470497212048372, 102.8488620819214390 ) ) ;
#3963 = EDGE_CURVE ( 'NONE', #23163, #18293, #22550, .T. ) ;
#3964 = ADVANCED_FACE ( 'NONE', ( #7052, #17102 ), #4485, .F. ) ;
#3965 = FACE_BOUND ( 'NONE', #23733, .T. ) ;
#3966 = CARTESIAN_POINT ( 'NONE',  ( 4.984841277089725686, 213.7757310962907411, 37.55113791807855961 ) ) ;
#3967 = DIRECTION ( 'NONE',  ( 0.000000000000000000, -1.000000000000000000, 9.859324684083082301E-16 ) ) ;
#3968 = ORIENTED_EDGE ( 'NONE', *, *, #33516, .F. ) ;
#3969 = CARTESIAN_POINT ( 'NONE',  ( 36.42499999726879878, 141.7447067706911810, 9.630534252274376428 ) ) ;
#3970 = CARTESIAN_POINT ( 'NONE',  ( 39.38867513459481984, 169.2658477444273331, 4.635254915624208216 ) ) ;
#3972 = EDGE_CURVE ( 'NONE', #12567, #1785, #23202, .T. ) ;
#3971 = CARTESIAN_POINT ( 'NONE',  ( -8.118202686958138514, 212.8392687619910930, 65.79886208192144181 ) ) ;
#3973 = CARTESIAN_POINT ( 'NONE',  ( 39.37499999726880873, 155.0000000000000000, -15.58253175000000823 ) ) ;
#3974 = CARTESIAN_POINT ( 'NONE',  ( -125.0000000000000000, 0.000000000000000000, 20.00000000000000000 ) ) ;
#3975 = CARTESIAN_POINT ( 'NONE',  ( 8.118202686958039038, 212.8392687619912635, 1.701137918078565736 ) ) ;
#3976 = EDGE_CURVE ( 'NONE', #5752, #5188, #32933, .T. ) ;
#3977 = AXIS2_PLACEMENT_3D ( 'NONE', #10455, #380, #25940 ) ;
#3978 = CARTESIAN_POINT ( 'NONE',  ( 61.30000000000000426, 163.5228861582408797, 11.73074641843673049 ) ) ;
#3979 =( BOUNDED_CURVE ( )  B_SPLINE_CURVE ( 2, ( #26987, #29386, #16425, #5705, #16093, #26821, #26487, #19156, #32103, #3485, #3156 ),
 .UNSPECIFIED., .F., .F. ) 
 B_SPLINE_CURVE_WITH_KNOTS ( ( 3, 2, 2, 2, 2, 3 ),
 ( 0.05357142857142836723, 0.05714285714285691903, 0.06071428571428558185, 0.06428571428571414059, 0.06785714285714269933, 0.07142857142857124420 ),
 .UNSPECIFIED. ) 
 CURVE ( )  GEOMETRIC_REPRESENTATION_ITEM ( )  RATIONAL_B_SPLINE_CURVE ( ( 1.000000000000001776, 0.9510565162951518658, 1.000000000000000000, 0.9510565162951534202, 1.000000000000000000, 0.9510565162951534202, 1.000000000000000000, 0.9510565162951534202, 1.000000000000000000, 0.9510565162951555296, 0.9999999999999978906 ) ) 
 REPRESENTATION_ITEM ( '' )  );
#3980 = FACE_BOUND ( 'NONE', #32570, .T. ) ;
#3981 = CARTESIAN_POINT ( 'NONE',  ( -4.984841277089891776, 213.7757310962905990, 83.94886208192144750 ) ) ;
#3982 = DIRECTION ( 'NONE',  ( 1.000000000000000000, -0.000000000000000000, -0.000000000000000000 ) ) ;
#3983 = AXIS2_PLACEMENT_3D ( 'NONE', #32618, #27001, #19510 ) ;
#3984 = CARTESIAN_POINT ( 'NONE',  ( 107.5000000000000000, 155.0000000000000000, 69.99999999999998579 ) ) ;
#3985 = VECTOR ( 'NONE', #12306, 1000.000000000000000 ) ;
#3986 = CARTESIAN_POINT ( 'NONE',  ( 63.52499999726880731, 169.8198683612136222, -4.815267126137197984 ) ) ;
#3988 = ORIENTED_EDGE ( 'NONE', *, *, #4099, .T. ) ;
#3987 = CARTESIAN_POINT ( 'NONE',  ( 8.062137200540920645, 201.0835637161417822, 20.30113791807856671 ) ) ;
#3989 = CARTESIAN_POINT ( 'NONE',  ( -11.41286821541921626, 25.16504226903141372, -0.07154745401828305207 ) ) ;
#3990 = CARTESIAN_POINT ( 'NONE',  ( 84.87499999726881583, 138.6155565068815463, -3.929120461958505118E-15 ) ) ;
#3991 = CARTESIAN_POINT ( 'NONE',  ( 12.01549611932652972, 210.8513442034534933, 85.85113791807857808 ) ) ;
#3992 = CARTESIAN_POINT ( 'NONE',  ( 72.08867513459482268, 142.2402378747194405, 9.270509831248432420 ) ) ;
#3993 = CARTESIAN_POINT ( 'NONE',  ( 52.98867513459482126, 163.8167787843871110, -12.13525491562423397 ) ) ;
#3994 = ORIENTED_EDGE ( 'NONE', *, *, #574, .T. ) ;
#3995 = CARTESIAN_POINT ( 'NONE',  ( 3.753561863808876797, 195.6020594897209719, 70.59886208192142476 ) ) ;
#3996 = CIRCLE ( 'NONE', #31200, 4.199999999999988631 ) ;
#3997 = CARTESIAN_POINT ( 'NONE',  ( -6.220909254589682469, 215.4770327129947134, 77.94886208192141908 ) ) ;
#3998 = CARTESIAN_POINT ( 'NONE',  ( 0.05014649552828288198, 194.3824533091408000, 10.74886208192143577 ) ) ;
#3999 = PRESENTATION_LAYER_ASSIGNMENT (  '', '', ( #25276 ) ) ;
#4000 = DIRECTION ( 'NONE',  ( 0.000000000000000000, -0.7071067811865346942, 0.7071067811865604513 ) ) ;
#4001 = CARTESIAN_POINT ( 'NONE',  ( -3.135527875058821579, 197.5041725223112223, 23.90113791807856813 ) ) ;
#4002 = CARTESIAN_POINT ( 'NONE',  ( 6.139770520408223575, 215.5359834540460611, 93.54886208192139918 ) ) ;
#4003 = CARTESIAN_POINT ( 'NONE',  ( 39.41132485994281609, 142.2402378747194405, -9.270509831248439525 ) ) ;
#4004 = AXIS2_PLACEMENT_3D ( 'NONE', #13608, #6100, #18734 ) ;
#4005 = ORIENTED_EDGE ( 'NONE', *, *, #26473, .T. ) ;
#4006 = DIRECTION ( 'NONE',  ( 0.000000000000000000, 0.000000000000000000, -1.000000000000000000 ) ) ;
#4007 = CARTESIAN_POINT ( 'NONE',  ( -4.984841277089891776, 213.7757310962905990, 71.94886208192144750 ) ) ;
#4008 = TOROIDAL_SURFACE ( 'NONE', #10009, 69.99999999999998579, 30.00000000000000000 ) ;
#4009 = ORIENTED_EDGE ( 'NONE', *, *, #23927, .T. ) ;
#4010 = AXIS2_PLACEMENT_3D ( 'NONE', #22014, #22687, #29681 ) ;
#4011 = CARTESIAN_POINT ( 'NONE',  ( 85.92499999726881299, 164.1591823560292198, 12.60653300113718167 ) ) ;
#4012 = ORIENTED_EDGE ( 'NONE', *, *, #12277, .F. ) ;
#4013 = CARTESIAN_POINT ( 'NONE',  ( 69.18867513459483121, 169.2658477444273331, -4.635254915624224203 ) ) ;
#4014 = CARTESIAN_POINT ( 'NONE',  ( 73.82499999726879025, 168.2552932293087906, 9.630534252274372875 ) ) ;
#4015 = DIRECTION ( 'NONE',  ( -0.000000000000000000, -0.000000000000000000, -1.000000000000000000 ) ) ;
#4016 = CARTESIAN_POINT ( 'NONE',  ( 0.05014649552807626948, 215.4116977939061144, 70.25113791807856956 ) ) ;
#4017 = CARTESIAN_POINT ( 'NONE',  ( 87.50000000000005684, 169.8972688042864831, 3.304339362361343291 ) ) ;
#4018 = MECHANICAL_DESIGN_GEOMETRIC_PRESENTATION_REPRESENTATION (  '', ( #13819 ), #3476 ) ;
#4019 =( NAMED_UNIT ( * ) SI_UNIT ( $, .STERADIAN. ) SOLID_ANGLE_UNIT ( ) );
#4020 = CARTESIAN_POINT ( 'NONE',  ( 39.39999999999999858, 159.7113355953771077, 14.49999999999999289 ) ) ;
#4021 = CARTESIAN_POINT ( 'NONE',  ( 0.05014649552828262524, 198.5883022060938572, 52.74886208192144466 ) ) ;
#4022 = FACE_OUTER_BOUND ( 'NONE', #10720, .T. ) ;
#4023 = DIRECTION ( 'NONE',  ( 1.000000000000000000, 0.000000000000000000, 0.000000000000000000 ) ) ;
#4024 = VECTOR ( 'NONE', #6461, 1000.000000000000000 ) ;
#4025 = CARTESIAN_POINT ( 'NONE',  ( -54.75000000000000711, -7.347880794884118356E-15, 20.00000000000000000 ) ) ;
#4026 = CARTESIAN_POINT ( 'NONE',  ( 51.12499999726881583, 155.0000000000000000, -15.58253175000000823 ) ) ;
#4027 = CARTESIAN_POINT ( 'NONE',  ( 3.753561863808689836, 218.3979405102790565, 58.40113791807858235 ) ) ;
#4028 = B_SPLINE_CURVE_WITH_KNOTS ( 'NONE', 3,
 ( #12052, #1331, #30282, #20226, #27220, #4561, #24832, #14268, #32661, #29949 ),
 .UNSPECIFIED., .F., .F.,
 ( 4, 2, 2, 2, 4 ),
 ( 0.000000000000000000, 0.001989602278884366159, 0.003979204557768732317, 0.005968806836653096741, 0.007958409115537461165 ),
 .UNSPECIFIED. ) ;
#4029 = CARTESIAN_POINT ( 'NONE',  ( 40.81132485994281467, 150.1262045565064511, 15.00000000000004086 ) ) ;
#4030 = CIRCLE ( 'NONE', #24140, 1.000000000000000222 ) ;
#4031 = CARTESIAN_POINT ( 'NONE',  ( -6.220909254589537696, 198.5229672870051161, 102.0511379180785383 ) ) ;
#4032 = CARTESIAN_POINT ( 'NONE',  ( -10.00000000000000711, 207.0476921513413515, 78.50113791807856956 ) ) ;
#4033 = CARTESIAN_POINT ( 'NONE',  ( -9.680171189290716072, 199.9079932115567146, 38.19886208192142618 ) ) ;
#4034 = CARTESIAN_POINT ( 'NONE',  ( 0.05014649552828275014, 196.4853777576173002, 49.74886208192142334 ) ) ;
#4035 = CARTESIAN_POINT ( 'NONE',  ( 86.39999999453762314, 168.7903194862797420, -4.480746418436745593 ) ) ;
#4036 = CARTESIAN_POINT ( 'NONE',  ( -9.736236675707914401, 199.9851607334237542, 90.20113791807857240 ) ) ;
#4037 = CARTESIAN_POINT ( 'NONE',  ( 8.000000000000008882, 206.9523078486586485, 95.00113791807856956 ) ) ;
#4038 = CARTESIAN_POINT ( 'NONE',  ( -9.984503880673420539, 203.7031108863293980, 62.34886208192143897 ) ) ;
#4039 = CARTESIAN_POINT ( 'NONE',  ( 3.280815508853482498, 7.221948645665444921, -7.591546097228400569 ) ) ;
#4040 = EDGE_LOOP ( 'NONE', ( #33510, #13113, #3533, #11933 ) ) ;
#4041 = CARTESIAN_POINT ( 'NONE',  ( 3.753561863808876797, 195.6020594897209719, 64.59886208192142476 ) ) ;
#4042 = ORIENTED_EDGE ( 'NONE', *, *, #11060, .F. ) ;
#4043 = CARTESIAN_POINT ( 'NONE',  ( 72.27499999726879309, 160.0630714827496206, 15.58253174999999402 ) ) ;
#4044 = CARTESIAN_POINT ( 'NONE',  ( -8.000000000000008882, 206.9523078486584780, 38.49886208192143044 ) ) ;
#4045 = VERTEX_POINT ( 'NONE', #20501 ) ;
#4046 = CARTESIAN_POINT ( 'NONE',  ( 83.77499999726880731, 169.8198683612136222, -4.815267126137197984 ) ) ;
#4047 = PLANE ( 'NONE',  #27123 ) ;
#4048 = DIRECTION ( 'NONE',  ( -1.000000000000000000, 0.000000000000000000, 0.000000000000000000 ) ) ;
#4049 = AXIS2_PLACEMENT_3D ( 'NONE', #21081, #18855, #13739 ) ;
#4050 = CARTESIAN_POINT ( 'NONE',  ( -6.444103211791042618, 211.7408657792732356, 57.80113791807857382 ) ) ;
#4051 = CARTESIAN_POINT ( 'NONE',  ( -3.044812012439970683, 197.4746971517856196, 46.89886208192143613 ) ) ;
#4052 = ORIENTED_EDGE ( 'NONE', *, *, #1445, .F. ) ;
#4053 = CARTESIAN_POINT ( 'NONE',  ( 2.000000000000000000, 0.000000000000000000, 0.000000000000000000 ) ) ;
#4054 = CARTESIAN_POINT ( 'NONE',  ( 4.000000000000000000, 3.518949890710768802, -4.770489558936219510E-15 ) ) ;
#4055 = DIRECTION ( 'NONE',  ( -0.000000000000000000, -0.000000000000000000, -1.000000000000000000 ) ) ;
#4056 = CARTESIAN_POINT ( 'NONE',  ( 2.517493886309087436, 199.4062855549015865, 25.59886208192143897 ) ) ;
#4057 = CARTESIAN_POINT ( 'NONE',  ( -0.05014649552810635652, 196.4853777576173002, 56.75113791807855534 ) ) ;
#4058 = EDGE_CURVE ( 'NONE', #19467, #20904, #8066, .T. ) ;
#4059 = CARTESIAN_POINT ( 'NONE',  ( 8.062137200540920645, 201.0835637161417822, 44.30113791807857382 ) ) ;
#4060 = CARTESIAN_POINT ( 'NONE',  ( 38.41132485994281609, 167.7597621252805880, 9.270509831248428867 ) ) ;
#4061 = CONTEXT_DEPENDENT_SHAPE_REPRESENTATION ( #22060, #13892 ) ;
#4062 = CARTESIAN_POINT ( 'NONE',  ( -9.984503880673473830, 210.2968891136704315, 15.65113791807856813 ) ) ;
#4063 = CARTESIAN_POINT ( 'NONE',  ( -8.000000000000008882, 206.9523078486584780, 101.4988620819214304 ) ) ;
#4064 = CARTESIAN_POINT ( 'NONE',  ( 45.22499999726881015, 160.0630714827496206, -15.58253175000000823 ) ) ;
#4065 = DIRECTION ( 'NONE',  ( 1.000000000000000000, 0.000000000000000000, 0.000000000000000000 ) ) ;
#4066 = CARTESIAN_POINT ( 'NONE',  ( -125.0000000000000000, -25.00000000000000000, -35.00000000000000000 ) ) ;
#4067 = CARTESIAN_POINT ( 'NONE',  ( -12.01549611932652972, 203.1486557965464499, 30.35113791807856742 ) ) ;
#4068 = CARTESIAN_POINT ( 'NONE',  ( 81.78867513459482552, 155.0000000000000000, 15.00000000000001243 ) ) ;
#4069 = CARTESIAN_POINT ( 'NONE',  ( -6.220909254589537696, 198.5229672870051161, 78.05113791807858092 ) ) ;
#4070 = CARTESIAN_POINT ( 'NONE',  ( 9.984503880673473830, 203.7031108863295401, 38.15113791807857524 ) ) ;
#4071 = CARTESIAN_POINT ( 'NONE',  ( 75.98867513459481415, 146.1832212156128890, 12.13525491562421976 ) ) ;
#4072 = CARTESIAN_POINT ( 'NONE',  ( 9.093938419273300156, 26.50387701106810923, -17.76591125084756229 ) ) ;
#4073 = CARTESIAN_POINT ( 'NONE',  ( 3.662846001190051659, 195.5725841191953691, 101.6011379180785781 ) ) ;
#4074 = CARTESIAN_POINT ( 'NONE',  ( -3.044812012439970683, 197.4746971517856196, 16.89886208192143613 ) ) ;
#4075 = CARTESIAN_POINT ( 'NONE',  ( 66.09999999453764019, 159.7113355953771077, -14.50000000000000888 ) ) ;
#4076 = VERTEX_POINT ( 'NONE', #18116 ) ;
#4077 = CARTESIAN_POINT ( 'NONE',  ( 11.98450388067348271, 203.0532714938637753, 56.15113791807857524 ) ) ;
#4078 = CARTESIAN_POINT ( 'NONE',  ( -6.500168698208129925, 202.3363017425936050, 69.20113791807857240 ) ) ;
#4079 = CARTESIAN_POINT ( 'NONE',  ( -9.984503880673420539, 203.7031108863293980, 29.34886208192144252 ) ) ;
#4080 =( NAMED_UNIT ( * ) PLANE_ANGLE_UNIT ( ) SI_UNIT ( $, .RADIAN. ) );
#4081 = EDGE_LOOP ( 'NONE', ( #30312, #10229, #3042, #32399 ) ) ;
#4082 = CARTESIAN_POINT ( 'NONE',  ( 9.984503880673470277, 203.7031108863295401, 86.15113791807857524 ) ) ;
#4083 = ORIENTED_EDGE ( 'NONE', *, *, #9130, .T. ) ;
#4084 = DIRECTION ( 'NONE',  ( -1.000000000000000000, 0.000000000000000000, 0.000000000000000000 ) ) ;
#4085 = DIRECTION ( 'NONE',  ( 0.000000000000000000, 0.8660254037844380415, -0.5000000000000009992 ) ) ;
#4086 = ORIENTED_EDGE ( 'NONE', *, *, #19258, .F. ) ;
#4087 = CARTESIAN_POINT ( 'NONE',  ( -6.444103211791042618, 211.7408657792732356, 36.80113791807856671 ) ) ;
#4088 = CARTESIAN_POINT ( 'NONE',  ( 87.50000000000001421, 166.8192717339189812, 9.236060614774261879 ) ) ;
#4089 = CARTESIAN_POINT ( 'NONE',  ( 8.062137200540822946, 212.9164362838583315, 15.69886208192143506 ) ) ;
#4090 = CARTESIAN_POINT ( 'NONE',  ( 48.27499999726880731, 160.0630714827496206, 15.58253174999999224 ) ) ;
#4091 = ORIENTED_EDGE ( 'NONE', *, *, #17878, .F. ) ;
#4092 = CARTESIAN_POINT ( 'NONE',  ( 6.500168698208129925, 211.6636982574063381, 49.70113791807857240 ) ) ;
#4093 = CARTESIAN_POINT ( 'NONE',  ( 89.50000000000002842, 155.0000000000000000, 32.00000000000002842 ) ) ;
#4094 = DIRECTION ( 'NONE',  ( -0.8191520442889917986, 0.000000000000000000, -0.5735764363510460484 ) ) ;
#4095 = CARTESIAN_POINT ( 'NONE',  ( -0.05014649552828403384, 217.5146222423826714, 93.24886208192140202 ) ) ;
#4096 = CARTESIAN_POINT ( 'NONE',  ( 57.37499999726880873, 155.0000000000000000, -15.58253175000000823 ) ) ;
#4097 = CARTESIAN_POINT ( 'NONE',  ( -10.01549611932653860, 203.7984951890123284, 33.35113791807855677 ) ) ;
#4098 = FACE_OUTER_BOUND ( 'NONE', #14475, .T. ) ;
#4099 = EDGE_CURVE ( 'NONE', #26344, #8252, #7568, .T. ) ;
#4100 = CARTESIAN_POINT ( 'NONE',  ( 6.220909254589536808, 215.4770327129947702, 22.55113791807856671 ) ) ;
#4101 = CARTESIAN_POINT ( 'NONE',  ( 121.5000000000000000, 229.9533188057739039, -74.95331880577418815 ) ) ;
#4102 = CARTESIAN_POINT ( 'NONE',  ( 77.30000000000001137, 163.5228861582408797, 11.73074641843673049 ) ) ;
#4103 = DIRECTION ( 'NONE',  ( -1.000000000000000000, 0.000000000000000000, 0.000000000000000000 ) ) ;
#4104 = CARTESIAN_POINT ( 'NONE',  ( 10.00000000000000711, 206.9523078486586201, 92.00113791807858377 ) ) ;
#4105 = LINE ( 'NONE', #1389, #2633 ) ;
#4106 = CARTESIAN_POINT ( 'NONE',  ( 42.57499999726881157, 145.8408176439707802, 12.60653300113718345 ) ) ;
#4107 = CARTESIAN_POINT ( 'NONE',  ( 10.01549611932653860, 210.2015048109876716, 46.85113791807856387 ) ) ;
#4108 = CARTESIAN_POINT ( 'NONE',  ( 83.72499999726882436, 169.8198683612136222, 4.815267126137181997 ) ) ;
#4109 = ADVANCED_FACE ( 'NONE', ( #20834 ), #23485, .T. ) ;
#4110 = LINE ( 'NONE', #6677, #4867 ) ;
#4111 = FACE_OUTER_BOUND ( 'NONE', #1151, .T. ) ;
#4112 = CARTESIAN_POINT ( 'NONE',  ( 50.19999999453762740, 163.5228861582408797, -11.73074641843674470 ) ) ;
#4113 = ORIENTED_EDGE ( 'NONE', *, *, #7462, .T. ) ;
#4114 = CARTESIAN_POINT ( 'NONE',  ( -12.00000000000000711, 207.0476921513413515, 15.50113791807856600 ) ) ;
#4115 = CARTESIAN_POINT ( 'NONE',  ( 125.0000000000000000, 25.00000000000004619, -20.00000000000000000 ) ) ;
#4116 = CARTESIAN_POINT ( 'NONE',  ( 5.000000000000000000, -2.342598717236903383, 4.057500000000001883 ) ) ;
#4117 = ORIENTED_EDGE ( 'NONE', *, *, #11444, .T. ) ;
#4118 = CARTESIAN_POINT ( 'NONE',  ( -0.05014649552828442242, 219.6175466908591716, 42.24886208192143044 ) ) ;
#4119 = CARTESIAN_POINT ( 'NONE',  ( -31.74999999999995737, 0.000000000000000000, 0.000000000000000000 ) ) ;
#4120 = CARTESIAN_POINT ( 'NONE',  ( -3.135527875058821579, 197.5041725223112223, 59.90113791807856813 ) ) ;
#4121 = EDGE_CURVE ( 'NONE', #31784, #8655, #17522, .T. ) ;
#4122 =( BOUNDED_CURVE ( )  B_SPLINE_CURVE ( 2, ( #22651, #33038, #22484, #32366, #9709, #27931, #24710, #30493, #20098, #19420, #14811 ),
 .UNSPECIFIED., .F., .F. ) 
 B_SPLINE_CURVE_WITH_KNOTS ( ( 3, 2, 2, 2, 2, 3 ),
 ( 0.5178571428571427937, 0.5214285714285713524, 0.5249999999999999112, 0.5285714285714285809, 0.5321428571428571397, 0.5357142857142856984 ),
 .UNSPECIFIED. ) 
 CURVE ( )  GEOMETRIC_REPRESENTATION_ITEM ( )  RATIONAL_B_SPLINE_CURVE ( ( 1.000000000000000000, 0.9510565162951534202, 1.000000000000000000, 0.9510565162951534202, 1.000000000000000000, 0.9510565162951534202, 1.000000000000000000, 0.9510565162951534202, 1.000000000000000000, 0.9510565162951518658, 1.000000000000001554 ) ) 
 REPRESENTATION_ITEM ( '' )  );
#4123 = CARTESIAN_POINT ( 'NONE',  ( -2.426778023690076225, 199.3768101843759553, 25.89886208192143613 ) ) ;
#4124 = CARTESIAN_POINT ( 'NONE',  ( -4.336808689942017736E-16, 7.505553499465137612, -0.8000000000000003775 ) ) ;
#4125 = EDGE_LOOP ( 'NONE', ( #33172, #32411, #16064, #3478 ) ) ;
#4126 = CARTESIAN_POINT ( 'NONE',  ( 6.500168698208244500, 202.3363017425938324, 103.2988620819214560 ) ) ;
#4127 = EDGE_CURVE ( 'NONE', #6898, #26498, #22379, .T. ) ;
#4128 = CYLINDRICAL_SURFACE ( 'NONE', #14855, 2.428571428571428381 ) ;
#4129 = VECTOR ( 'NONE', #25492, 1000.000000000000000 ) ;
#4130 = CARTESIAN_POINT ( 'NONE',  ( 6.500168698208129925, 211.6636982574063381, 40.70113791807857240 ) ) ;
#4131 = CARTESIAN_POINT ( 'NONE',  ( 93.60208470531338776, 155.0000000000000000, 0.000000000000000000 ) ) ;
#4132 = ORIENTED_EDGE ( 'NONE', *, *, #27275, .T. ) ;
#4133 = CARTESIAN_POINT ( 'NONE',  ( 34.82499999726881157, 141.7447067706911810, -9.630534252274385310 ) ) ;
#4134 = CARTESIAN_POINT ( 'NONE',  ( 0.000000000000000000, 0.000000000000000000, -0.4621369752184044666 ) ) ;
#4135 = CARTESIAN_POINT ( 'NONE',  ( -8.118202686958039038, 201.1607312380087080, 0.2011379180785657361 ) ) ;
#4136 = CARTESIAN_POINT ( 'NONE',  ( 6.220909254589681581, 198.5229672870052582, 61.44886208192141908 ) ) ;
#4137 = CARTESIAN_POINT ( 'NONE',  ( 39.97499999726881015, 169.8198683612136222, 4.815267126137181997 ) ) ;
#4138 = CARTESIAN_POINT ( 'NONE',  ( 10.00000000000000711, 207.0000000000000853, 0.000000000000000000 ) ) ;
#4139 = CARTESIAN_POINT ( 'NONE',  ( -9.984503880673473830, 210.2968891136704315, 0.6511379180785656917 ) ) ;
#4140 = CARTESIAN_POINT ( 'NONE',  ( -3.500000000000001332, 1.693985822988415046, -0.2182856432892006648 ) ) ;
#4141 = CARTESIAN_POINT ( 'NONE',  ( 64.20000000000000284, 142.6655632788954620, -8.961492836873480528 ) ) ;
#4142 = DIRECTION ( 'NONE',  ( 1.000000000000000000, 0.000000000000000000, -0.000000000000000000 ) ) ;
#4143 = CARTESIAN_POINT ( 'NONE',  ( -2.426778023690076225, 199.3768101843759553, 79.89886208192143613 ) ) ;
#4144 = CARTESIAN_POINT ( 'NONE',  ( -4.406466114815342117, 6.116179640280717145, -7.446478553995464544 ) ) ;
#4145 = DIRECTION ( 'NONE',  ( -1.000000000000000000, 0.000000000000000000, 0.000000000000000000 ) ) ;
#4146 = CARTESIAN_POINT ( 'NONE',  ( 64.72499999726881015, 140.1801316387863778, -4.815267126137194431 ) ) ;
#4148 = ORIENTED_EDGE ( 'NONE', *, *, #33090, .T. ) ;
#4147 = CARTESIAN_POINT ( 'NONE',  ( -6.139770520408368348, 215.5359834540460042, 24.95113791807856174 ) ) ;
#4149 = CARTESIAN_POINT ( 'NONE',  ( -2.243702833038399902, 30.45886237079319514, -1.708299986272438842 ) ) ;
#4150 = CARTESIAN_POINT ( 'NONE',  ( 84.37499999726881583, 155.0000000000000000, 15.58253174999999402 ) ) ;
#4151 = CARTESIAN_POINT ( 'NONE',  ( -11.98450388067348804, 210.9467285061362247, 90.65113791807857524 ) ) ;
#4152 = ADVANCED_FACE ( 'NONE', ( #2787, #15720 ), #16050, .F. ) ;
#4153 = EDGE_CURVE ( 'NONE', #17881, #13027, #21000, .T. ) ;
#4154 = CARTESIAN_POINT ( 'NONE',  ( 97.30927364589244632, 155.0000000000000000, -31.00000000000000000 ) ) ;
#4155 = VERTEX_POINT ( 'NONE', #15884 ) ;
#4156 = CARTESIAN_POINT ( 'NONE',  ( 12.00000000000000711, 207.0476921513415220, 72.99886208192144466 ) ) ;
#4157 = CARTESIAN_POINT ( 'NONE',  ( -9.984503880673420539, 203.7031108863293980, 74.34886208192143897 ) ) ;
#4158 = CARTESIAN_POINT ( 'NONE',  ( -9.736236675708031640, 214.0148392665760753, 14.79886208192143471 ) ) ;
#4159 = DIRECTION ( 'NONE',  ( -1.000000000000000000, -0.000000000000000000, -0.000000000000000000 ) ) ;
#4160 = CARTESIAN_POINT ( 'NONE',  ( -6.139770520408369237, 215.5359834540460042, 27.95113791807856174 ) ) ;
#4161 = CARTESIAN_POINT ( 'NONE',  ( -1.750000000000014211, 3.031088913245526317, -2.899999999999999911 ) ) ;
#4162 = PRODUCT_RELATED_PRODUCT_CATEGORY ( 'part', '', ( #32253 ) ) ;
#4163 = EDGE_CURVE ( 'NONE', #8578, #31129, #13331, .T. ) ;
#4164 = CARTESIAN_POINT ( 'NONE',  ( -3.044812012439970683, 197.4746971517856196, 88.89886208192143613 ) ) ;
#4165 = AXIS2_PLACEMENT_3D ( 'NONE', #14276, #16662, #24676 ) ;
#4166 = DIRECTION ( 'NONE',  ( -0.5526942671207060176, -0.1536855300543007452, -0.8190908404712106128 ) ) ;
#4167 = ORIENTED_EDGE ( 'NONE', *, *, #27629, .T. ) ;
#4168 = CARTESIAN_POINT ( 'NONE',  ( 92.59660660068168170, 155.0000000000000000, 12.10452846326765020 ) ) ;
#4169 = CARTESIAN_POINT ( 'NONE',  ( 4.984841277089891776, 200.2242689037093726, 70.44886208192144750 ) ) ;
#4170 = EDGE_CURVE ( 'NONE', #24055, #10071, #25784, .T. ) ;
#4171 = ORIENTED_EDGE ( 'NONE', *, *, #2883, .T. ) ;
#4172 = CARTESIAN_POINT ( 'NONE',  ( 83.32499999726880446, 164.1591823560292198, -12.60653300113719766 ) ) ;
#4173 = VERTEX_POINT ( 'NONE', #23057 ) ;
#4174 = CARTESIAN_POINT ( 'NONE',  ( 69.71132485994280614, 155.0000000000000000, -15.00000000000002487 ) ) ;
#4175 = CARTESIAN_POINT ( 'NONE',  ( 76.02499999726880731, 160.0630714827496206, 15.58253174999999402 ) ) ;
#4176 = CARTESIAN_POINT ( 'NONE',  ( 112.4999999999999858, 155.0000000000000000, -6.938893903907228378E-15 ) ) ;
#4177 = CARTESIAN_POINT ( 'NONE',  ( 2.426778023690261410, 199.3768101843759837, 80.60113791807857808 ) ) ;
#4178 = LINE ( 'NONE', #32796, #3694 ) ;
#4179 = AXIS2_PLACEMENT_3D ( 'NONE', #4929, #9701, #31009 ) ;
#4180 = CIRCLE ( 'NONE', #15058, 13.50000000000001066 ) ;
#4181 = CARTESIAN_POINT ( 'NONE',  ( 39.80000000000000426, 142.6655632788954620, 8.961492836873471646 ) ) ;
#4182 = CARTESIAN_POINT ( 'NONE',  ( -2.517493886309087880, 214.5937144450984135, 51.09886208192143897 ) ) ;
#4183 = AXIS2_PLACEMENT_3D ( 'NONE', #1456, #15576, #22577 ) ;
#4184 = LINE ( 'NONE', #6578, #11041 ) ;
#4185 = DIRECTION ( 'NONE',  ( -1.000000000000000000, 0.000000000000000000, 0.000000000000000000 ) ) ;
#4186 = DIRECTION ( 'NONE',  ( -0.7071067811865314745, 0.000000000000000000, 0.7071067811865635599 ) ) ;
#4187 = CARTESIAN_POINT ( 'NONE',  ( 52.02499999726880731, 160.0630714827496206, 15.58253174999999224 ) ) ;
#4188 = CARTESIAN_POINT ( 'NONE',  ( 66.37499999726881583, 155.0000000000000000, 15.58253174999999402 ) ) ;
#4189 = CARTESIAN_POINT ( 'NONE',  ( 9.680171189290831535, 199.9079932115568852, 56.30113791807857382 ) ) ;
#4190 = CARTESIAN_POINT ( 'NONE',  ( 32.50000000000000000, 155.0000000000000000, -6.938893903907228378E-15 ) ) ;
#4191 = CARTESIAN_POINT ( 'NONE',  ( 3.753561863808689836, 218.3979405102790565, 1.401137918078565692 ) ) ;
#4193 = CARTESIAN_POINT ( 'NONE',  ( -3.135527875058821579, 197.5041725223112223, 80.90113791807858945 ) ) ;
#4192 =( REPRESENTATION_RELATIONSHIP ('NONE','NONE', #25663, #16299 ) REPRESENTATION_RELATIONSHIP_WITH_TRANSFORMATION ( #29628 )SHAPE_REPRESENTATION_RELATIONSHIP( ) );
#4194 = CARTESIAN_POINT ( 'NONE',  ( -7.375838497908014268, 196.7627149292498530, 41.04886208192144181 ) ) ;
#4195 = CARTESIAN_POINT ( 'NONE',  ( 6.220909254589680693, 198.5229672870052582, 49.44886208192144750 ) ) ;
#4196 = CARTESIAN_POINT ( 'NONE',  ( 87.59999999453762598, 141.2096805137202580, -4.480746418436742040 ) ) ;
#4197 = CARTESIAN_POINT ( 'NONE',  ( 0.05014649552807549926, 219.6175466908591716, 85.25113791807856956 ) ) ;
#4198 = AXIS2_PLACEMENT_3D ( 'NONE', #17897, #25895, #20622 ) ;
#4199 = CARTESIAN_POINT ( 'NONE',  ( 3.044812012440130555, 197.4746971517856764, 5.601137918078566535 ) ) ;
#4200 = CARTESIAN_POINT ( 'NONE',  ( 6.220909254589681581, 198.5229672870052582, 58.44886208192144039 ) ) ;
#4201 = DIRECTION ( 'NONE',  ( 1.000000000000000000, 0.000000000000000000, 0.000000000000000000 ) ) ;
#4202 = ORIENTED_EDGE ( 'NONE', *, *, #21802, .F. ) ;
#4203 = CARTESIAN_POINT ( 'NONE',  ( -3.753561863808878130, 218.3979405102790281, 72.09886208192142476 ) ) ;
#4204 = AXIS2_PLACEMENT_3D ( 'NONE', #17502, #24834, #4388 ) ;
#4205 = AXIS2_PLACEMENT_3D ( 'NONE', #7733, #15048, #23060 ) ;
#4206 = EDGE_LOOP ( 'NONE', ( #540, #18309 ) ) ;
#4207 = CARTESIAN_POINT ( 'NONE',  ( 70.57499999726881867, 145.8408176439707802, 12.60653300113718345 ) ) ;
#4208 = CARTESIAN_POINT ( 'NONE',  ( 2.517493886309087436, 199.4062855549015865, 46.59886208192143897 ) ) ;
#4209 = EDGE_LOOP ( 'NONE', ( #7500, #7245, #27184, #2457 ) ) ;
#4210 = CARTESIAN_POINT ( 'NONE',  ( 85.07499999726883289, 141.7447067706911810, -9.630534252274387086 ) ) ;
#4211 = DIRECTION ( 'NONE',  ( 0.000000000000000000, 0.000000000000000000, -1.000000000000000000 ) ) ;
#4212 = DIRECTION ( 'NONE',  ( 1.000000000000000000, 0.000000000000000000, 0.000000000000000000 ) ) ;
#4213 = CARTESIAN_POINT ( 'NONE',  ( 8.015496119326531499, 209.5516654185219636, 61.85113791807857098 ) ) ;
#4214 = CARTESIAN_POINT ( 'NONE',  ( -9.984503880673420539, 203.7031108863293980, 41.34886208192143897 ) ) ;
#4215 = ORIENTED_EDGE ( 'NONE', *, *, #3882, .F. ) ;
#4216 = DIRECTION ( 'NONE',  ( 0.000000000000000000, 0.000000000000000000, -1.000000000000000000 ) ) ;
#4217 = SURFACE_STYLE_USAGE ( .BOTH. , #32163 ) ;
#4218 = DIRECTION ( 'NONE',  ( 0.000000000000000000, 0.000000000000000000, 1.000000000000000000 ) ) ;
#4219 = DIRECTION ( 'NONE',  ( 1.000000000000000000, -0.000000000000000000, -0.000000000000000000 ) ) ;
#4220 = CARTESIAN_POINT ( 'NONE',  ( 6.500168698208244500, 202.3363017425938324, 22.29886208192143826 ) ) ;
#4221 = AXIS2_PLACEMENT_3D ( 'NONE', #8999, #1665, #1501 ) ;
#4222 = CARTESIAN_POINT ( 'NONE',  ( 8.062137200540920645, 201.0835637161417822, 65.30113791807858092 ) ) ;
#4223 = CARTESIAN_POINT ( 'NONE',  ( 10.00000000000000711, 206.9523078486586201, 50.00113791807856956 ) ) ;
#4224 = FACE_OUTER_BOUND ( 'NONE', #13593, .T. ) ;
#4225 = CONTEXT_DEPENDENT_SHAPE_REPRESENTATION ( #9881, #19061 ) ;
#4226 = CIRCLE ( 'NONE', #29797, 5.000000000000001776 ) ;
#4227 = CARTESIAN_POINT ( 'NONE',  ( 10.00000000000000711, 206.9523078486586201, 20.00113791807856600 ) ) ;
#4228 = CARTESIAN_POINT ( 'NONE',  ( 2.517493886308900919, 214.5937144450984420, 4.401137918078566358 ) ) ;
#4229 = CARTESIAN_POINT ( 'NONE',  ( 41.82499999726881157, 168.2552932293087906, 9.630534252274372875 ) ) ;
#4230 = FACE_BOUND ( 'NONE', #27225, .T. ) ;
#4231 = CARTESIAN_POINT ( 'NONE',  ( 34.42499999726880588, 141.7447067706911810, 9.630534252274376428 ) ) ;
#4232 = CARTESIAN_POINT ( 'NONE',  ( -11.98450388067348804, 210.9467285061362247, 27.65113791807857169 ) ) ;
#4233 = LINE ( 'NONE', #29969, #18431 ) ;
#4234 = CARTESIAN_POINT ( 'NONE',  ( 9.984503880673470277, 203.7031108863295401, 74.15113791807854682 ) ) ;
#4235 = CARTESIAN_POINT ( 'NONE',  ( 3.135527875058820690, 216.4958274776887492, 49.40113791807857524 ) ) ;
#4236 = VECTOR ( 'NONE', #32723, 1000.000000000000000 ) ;
#4237 = CARTESIAN_POINT ( 'NONE',  ( 76.18867513459481700, 140.7341522555726669, 4.635254915624211769 ) ) ;
#4238 = FACE_BOUND ( 'NONE', #23300, .T. ) ;
#4239 = CARTESIAN_POINT ( 'NONE',  ( -12.01549611932659722, 210.8513442034533227, 17.64886208192143968 ) ) ;
#4240 = CARTESIAN_POINT ( 'NONE',  ( 6.139770520408223575, 215.5359834540460611, 15.54886208192143471 ) ) ;
#4241 = CARTESIAN_POINT ( 'NONE',  ( 69.49999999453763166, 139.7537977485451393, -4.138211985947621020E-15 ) ) ;
#4242 = ORIENTED_EDGE ( 'NONE', *, *, #5161, .T. ) ;
#4243 = CARTESIAN_POINT ( 'NONE',  ( 3.753561863808689836, 218.3979405102790565, 55.40113791807858235 ) ) ;
#4244 = CARTESIAN_POINT ( 'NONE',  ( 6.444103211791042618, 202.2591342207267644, 65.30113791807858092 ) ) ;
#4245 = CARTESIAN_POINT ( 'NONE',  ( -3.135527875058982783, 216.4958274776886924, 27.09886208192143542 ) ) ;
#4246 = CARTESIAN_POINT ( 'NONE',  ( 45.61132485994281183, 150.1262045565064795, -15.00000000000007638 ) ) ;
#4247 = EDGE_LOOP ( 'NONE', ( #2141, #30712 ) ) ;
#4248 = ORIENTED_EDGE ( 'NONE', *, *, #25720, .T. ) ;
#4249 = CARTESIAN_POINT ( 'NONE',  ( 6.220909254589536808, 215.4770327129947702, 88.55113791807853829 ) ) ;
#4250 = AXIS2_PLACEMENT_3D ( 'NONE', #26142, #26305, #2976 ) ;
#4251 = ORIENTED_EDGE ( 'NONE', *, *, #29982, .F. ) ;
#4252 = EDGE_CURVE ( 'NONE', #3823, #10681, #19124, .T. ) ;
#4253 = AXIS2_PLACEMENT_3D ( 'NONE', #31822, #23662, #13429 ) ;
#4254 = B_SPLINE_CURVE_WITH_KNOTS ( 'NONE', 3,
 ( #17277, #14715, #15056, #15232, #20685, #7579, #22899, #33631, #25620, #18128, #15400, #25956 ),
 .UNSPECIFIED., .F., .F.,
 ( 4, 2, 2, 2, 2, 4 ),
 ( 0.001914709330258871581, 0.002152771118959677116, 0.002390832907660482651, 0.002866956485062089818, 0.003343080062463696552, 0.003819203639865303718 ),
 .UNSPECIFIED. ) ;
#4255 = CARTESIAN_POINT ( 'NONE',  ( 64.71132485994279193, 155.0000000000000000, 15.00000000000001243 ) ) ;
#4256 = CARTESIAN_POINT ( 'NONE',  ( 3.978477517404916064, 5.573260695678954768, -6.171287963165197787 ) ) ;
#4257 = ORIENTED_EDGE ( 'NONE', *, *, #9759, .T. ) ;
#4258 = CARTESIAN_POINT ( 'NONE',  ( -2.426778023690262742, 214.6231898156240163, 37.10113791807857098 ) ) ;
#4259 = CARTESIAN_POINT ( 'NONE',  ( -0.3755270751584372513, 206.7692714347155629, 108.3323677711371573 ) ) ;
#4260 = CARTESIAN_POINT ( 'NONE',  ( 3.044812012439969795, 216.5253028482143520, 12.39886208192143435 ) ) ;
#4261 = CARTESIAN_POINT ( 'NONE',  ( 58.47499999726881725, 149.9369285172503510, 15.58253174999999580 ) ) ;
#4263 = ORIENTED_EDGE ( 'NONE', *, *, #22410, .T. ) ;
#4262 = VECTOR ( 'NONE', #22418, 1000.000000000000114 ) ;
#4264 = CARTESIAN_POINT ( 'NONE',  ( -8.000000000000008882, 207.0476921513413515, 45.50113791807857666 ) ) ;
#4265 = DIRECTION ( 'NONE',  ( -0.8660254037844362651, 0.5000000000000041078, 0.000000000000000000 ) ) ;
#4266 = DIRECTION ( 'NONE',  ( 1.000000000000000000, 0.000000000000000000, 0.000000000000000000 ) ) ;
#4267 = CARTESIAN_POINT ( 'NONE',  ( 0.000000000000000000, 0.000000000000000000, 0.000000000000000000 ) ) ;
#4268 = CARTESIAN_POINT ( 'NONE',  ( -3.044812012439970683, 197.4746971517856196, 103.8988620819214361 ) ) ;
#4269 = CARTESIAN_POINT ( 'NONE',  ( 64.47499999726881015, 149.9369285172503510, 15.58253174999999580 ) ) ;
#4270 = CARTESIAN_POINT ( 'NONE',  ( -3.135527875058821579, 197.5041725223112223, 35.90113791807856813 ) ) ;
#4271 = SURFACE_STYLE_FILL_AREA ( #27603 ) ;
#4272 = CARTESIAN_POINT ( 'NONE',  ( -8.118202686958039038, 201.1607312380087080, 15.20113791807856884 ) ) ;
#4273 = CARTESIAN_POINT ( 'NONE',  ( 132.3999999999999773, 80.04668119422662187, 74.95331880577468553 ) ) ;
#4274 = CARTESIAN_POINT ( 'NONE',  ( 79.90000000000000568, 141.2096805137202580, 4.480746418436733158 ) ) ;
#4275 = DIRECTION ( 'NONE',  ( -0.000000000000000000, -0.000000000000000000, 1.000000000000000000 ) ) ;
#4276 = DIRECTION ( 'NONE',  ( 0.000000000000000000, 0.9963496021943381020, -0.08536668089591059605 ) ) ;
#4277 = ADVANCED_FACE ( 'NONE', ( #28344 ), #8784, .F. ) ;
#4278 = CARTESIAN_POINT ( 'NONE',  ( 3.753561863808689836, 218.3979405102790565, 1.401137918078565692 ) ) ;
#4279 = VECTOR ( 'NONE', #30085, 1000.000000000000000 ) ;
#4280 = CARTESIAN_POINT ( 'NONE',  ( 110.1179863365115636, 155.0000000000000000, -32.10452846326764131 ) ) ;
#4281 = CARTESIAN_POINT ( 'NONE',  ( 46.67499999726880588, 141.7447067706911810, 9.630534252274376428 ) ) ;
#4282 = CARTESIAN_POINT ( 'NONE',  ( 8.062137200540920645, 201.0835637161417822, 47.30113791807857382 ) ) ;
#4283 = VECTOR ( 'NONE', #28740, 1000.000000000000114 ) ;
#4284 = CARTESIAN_POINT ( 'NONE',  ( 82.42499999726882720, 141.7447067706911810, 9.630534252274376428 ) ) ;
#4285 = AXIS2_PLACEMENT_3D ( 'NONE', #15423, #12866, #28550 ) ;
#4286 = CARTESIAN_POINT ( 'NONE',  ( -52.50000000000002132, 155.0000000000000000, 6.938893903907228378E-15 ) ) ;
#4287 = CARTESIAN_POINT ( 'NONE',  ( -12.99999999999999112, -3.903127820947815962E-15, 0.000000000000000000 ) ) ;
#4288 = CARTESIAN_POINT ( 'NONE',  ( 45.89999999453762314, 150.2886644046228639, -14.50000000000000888 ) ) ;
#4289 = ORIENTED_EDGE ( 'NONE', *, *, #29372, .F. ) ;
#4290 = CARTESIAN_POINT ( 'NONE',  ( -11.98450388067348804, 210.9467285061362247, 27.65113791807857169 ) ) ;
#4291 = CARTESIAN_POINT ( 'NONE',  ( 98.19869130599479945, 155.0000000000000000, 32.10452846326769816 ) ) ;
#4292 = CONICAL_SURFACE ( 'NONE', #13529, 3.047499999999999876, 1.047197551196590748 ) ;
#4293 = CYLINDRICAL_SURFACE ( 'NONE', #33547, 12.99999999999999822 ) ;
#4294 = ORIENTED_EDGE ( 'NONE', *, *, #5442, .F. ) ;
#4295 = CARTESIAN_POINT ( 'NONE',  ( -0.05014649552828442242, 219.6175466908591716, 45.24886208192143755 ) ) ;
#4296 = CARTESIAN_POINT ( 'NONE',  ( 6.220909254589536808, 215.4770327129947702, 4.551137918078564937 ) ) ;
#4297 = CARTESIAN_POINT ( 'NONE',  ( -8.062137200540920645, 212.9164362838581894, 63.80113791807858092 ) ) ;
#4298 = CARTESIAN_POINT ( 'NONE',  ( 4.903702542908435547, 213.8346818373419751, 27.54886208192144181 ) ) ;
#4299 = ADVANCED_FACE ( 'NONE', ( #11280 ), #11613, .F. ) ;
#4300 = CARTESIAN_POINT ( 'NONE',  ( 115.4999999999999858, 52.61186241335891367, 27.43481878086798176 ) ) ;
#4301 = EDGE_LOOP ( 'NONE', ( #17124, #24743 ) ) ;
#4302 = CARTESIAN_POINT ( 'NONE',  ( 8.015496119326531499, 209.5516654185219636, 4.851137918078565647 ) ) ;
#4303 = EDGE_CURVE ( 'NONE', #29326, #14989, #20782, .T. ) ;
#4304 = CIRCLE ( 'NONE', #27694, 12.00000000000001066 ) ;
#4305 = CYLINDRICAL_SURFACE ( 'NONE', #18679, 15.00000000000001776 ) ;
#4306 = CARTESIAN_POINT ( 'NONE',  ( 7.456977232089471386, 196.8216656703012006, 88.44886208192144750 ) ) ;
#4307 = CARTESIAN_POINT ( 'NONE',  ( 39.07499999726881157, 141.7447067706911810, -9.630534252274387086 ) ) ;
#4308 = ORIENTED_EDGE ( 'NONE', *, *, #25161, .T. ) ;
#4309 = CARTESIAN_POINT ( 'NONE',  ( 47.22499999726881015, 160.0630714827496206, -15.58253175000000823 ) ) ;
#4310 = CARTESIAN_POINT ( 'NONE',  ( 95.59906517536109050, 155.0000000000000000, 31.00000000000000000 ) ) ;
#4311 = EDGE_CURVE ( 'NONE', #29827, #11491, #10949, .T. ) ;
#4312 = CARTESIAN_POINT ( 'NONE',  ( -9.657736897290682521, 207.8482824000647611, 102.5857182426188388 ) ) ;
#4313 = CARTESIAN_POINT ( 'NONE',  ( -10.01549611932659722, 210.2015048109875011, 74.64886208192142192 ) ) ;
#4314 = CARTESIAN_POINT ( 'NONE',  ( 38.37499999726880873, 155.0000000000000000, 15.58253174999999402 ) ) ;
#4315 = FACE_BOUND ( 'NONE', #4247, .T. ) ;
#4316 = CARTESIAN_POINT ( 'NONE',  ( 9.984503880673470277, 203.7031108863295401, 5.151137918078567246 ) ) ;
#4317 = CARTESIAN_POINT ( 'NONE',  ( -3.499999999999999112, 0.3416723310689463444, 2.286988957586610299E-17 ) ) ;
#4318 = CARTESIAN_POINT ( 'NONE',  ( 59.19999999999999574, 167.3344367211045096, 8.961492836873468093 ) ) ;
#4319 = CARTESIAN_POINT ( 'NONE',  ( 64.31132485994281467, 169.2658477444273331, 4.635254915624208216 ) ) ;
#4320 = CARTESIAN_POINT ( 'NONE',  ( -8.015496119326597224, 209.5516654185217362, 86.64886208192143613 ) ) ;
#4321 = DIRECTION ( 'NONE',  ( 0.000000000000000000, 0.000000000000000000, 1.000000000000000000 ) ) ;
#4322 = CARTESIAN_POINT ( 'NONE',  ( 5.000000000000000000, 4.685197434473814759, -5.637851296924623057E-15 ) ) ;
#4323 = EDGE_CURVE ( 'NONE', #24997, #747, #21840, .T. ) ;
#4324 = CARTESIAN_POINT ( 'NONE',  ( 3.662846001189864698, 218.4274158808046593, 90.39886208192143613 ) ) ;
#4325 = CARTESIAN_POINT ( 'NONE',  ( 64.92499999726881299, 145.8408176439707802, -12.60653300113719588 ) ) ;
#4327 = VERTEX_POINT ( 'NONE', #8720 ) ;
#4326 = CARTESIAN_POINT ( 'NONE',  ( 0.05014649552810506589, 217.5146222423826714, 22.25113791807856956 ) ) ;
#4328 = CARTESIAN_POINT ( 'NONE',  ( -0.3755270751584372513, 206.7692714347155629, 108.3323677711371573 ) ) ;
#4329 = CARTESIAN_POINT ( 'NONE',  ( 82.37499999726881583, 155.0000000000000000, 15.58253174999999402 ) ) ;
#4330 = CARTESIAN_POINT ( 'NONE',  ( 9.680171189290831535, 199.9079932115568852, 89.30113791807858092 ) ) ;
#4331 = AXIS2_PLACEMENT_3D ( 'NONE', #18954, #26951, #10796 ) ;
#4332 = ADVANCED_FACE ( 'NONE', ( #6323 ), #29500, .F. ) ;
#4333 = DIRECTION ( 'NONE',  ( 0.000000000000000000, 0.000000000000000000, -1.000000000000000000 ) ) ;
#4334 = ORIENTED_EDGE ( 'NONE', *, *, #32696, .F. ) ;
#4335 = CARTESIAN_POINT ( 'NONE',  ( -12.00000000000000711, 206.9523078486584780, 68.49886208192144466 ) ) ;
#4336 = CARTESIAN_POINT ( 'NONE',  ( 3.135527875058981895, 197.5041725223112792, 73.59886208192143897 ) ) ;
#4337 = CARTESIAN_POINT ( 'NONE',  ( 3.662846001189864698, 218.4274158808046593, 9.398862081921436129 ) ) ;
#4338 = CARTESIAN_POINT ( 'NONE',  ( -27.50000000000000711, -9.324699302609172236, -17.12819780694306004 ) ) ;
#4339 = CARTESIAN_POINT ( 'NONE',  ( 8.062137200540920645, 201.0835637161417822, 35.30113791807857382 ) ) ;
#4340 = DIRECTION ( 'NONE',  ( 0.000000000000000000, 0.000000000000000000, -1.000000000000000000 ) ) ;
#4341 = CARTESIAN_POINT ( 'NONE',  ( 8.062137200540822946, 212.9164362838583315, 93.69886208192143329 ) ) ;
#4342 = EDGE_CURVE ( 'NONE', #26926, #8252, #19662, .T. ) ;
#4343 = LINE ( 'NONE', #12347, #9410 ) ;
#4344 = ORIENTED_EDGE ( 'NONE', *, *, #11903, .T. ) ;
#4345 = CARTESIAN_POINT ( 'NONE',  ( 5.000000000000000000, 4.685197434473814759, -5.637851296924623057E-15 ) ) ;
#4346 = CARTESIAN_POINT ( 'NONE',  ( -0.05014649552828365914, 215.4116977939061144, 78.24886208192144466 ) ) ;
#4347 = ORIENTED_EDGE ( 'NONE', *, *, #33290, .F. ) ;
#4348 = CARTESIAN_POINT ( 'NONE',  ( 82.42499999726882720, 141.7447067706911810, 9.630534252274376428 ) ) ;
#4349 = VERTEX_POINT ( 'NONE', #27117 ) ;
#4350 = CARTESIAN_POINT ( 'NONE',  ( 92.60208470531341618, 155.0000000000000000, 0.000000000000000000 ) ) ;
#4351 = CARTESIAN_POINT ( 'NONE',  ( 73.62499999726883004, 171.3844434931184253, -7.942151717890132712E-15 ) ) ;
#4352 = CARTESIAN_POINT ( 'NONE',  ( 77.50000000000000000, 155.0000000000000000, 69.99999999999998579 ) ) ;
#4353 = CARTESIAN_POINT ( 'NONE',  ( 6.500168698208129925, 211.6636982574063381, 76.70113791807857240 ) ) ;
#4354 = EDGE_CURVE ( 'NONE', #3157, #20526, #13668, .T. ) ;
#4355 = CARTESIAN_POINT ( 'NONE',  ( -145.0000000000000000, 0.000000000000000000, -20.00000000000000000 ) ) ;
#4356 = CARTESIAN_POINT ( 'NONE',  ( 41.09999999999999432, 168.7903194862797420, 4.480746418436729606 ) ) ;
#4357 = CARTESIAN_POINT ( 'NONE',  ( 2.517493886309087436, 199.4062855549015865, 55.59886208192143897 ) ) ;
#4358 = ADVANCED_FACE ( 'NONE', ( #14166 ), #26943, .T. ) ;
#4359 = CIRCLE ( 'NONE', #33212, 2.200000000000001066 ) ;
#4360 = CARTESIAN_POINT ( 'NONE',  ( 125.5000000000000000, 228.4330392262239116, 76.47359838532422316 ) ) ;
#4361 = CARTESIAN_POINT ( 'NONE',  ( -7.500000000000000000, 4.330127018922191873, -7.422398894150032511 ) ) ;
#4362 = DIRECTION ( 'NONE',  ( 0.000000000000000000, 0.000000000000000000, 1.000000000000000000 ) ) ;
#4363 = CARTESIAN_POINT ( 'NONE',  ( 50.72499999726881725, 140.1801316387863778, -4.815267126137194431 ) ) ;
#4364 = CARTESIAN_POINT ( 'NONE',  ( 61.47499999726879594, 160.0630714827496206, -15.58253175000000823 ) ) ;
#4365 = CARTESIAN_POINT ( 'NONE',  ( 9.736236675707914401, 214.0148392665762458, 61.70113791807857240 ) ) ;
#4366 = DIRECTION ( 'NONE',  ( 1.000000000000000000, 0.000000000000000000, 0.000000000000000000 ) ) ;
#4367 = ADVANCED_FACE ( 'NONE', ( #13830 ), #14233, .F. ) ;
#4368 = CARTESIAN_POINT ( 'NONE',  ( -8.118202686958039038, 201.1607312380087080, 102.2011379180785866 ) ) ;
#4369 = CARTESIAN_POINT ( 'NONE',  ( 6.139770520408367460, 198.4640165459539389, 77.45113791807855819 ) ) ;
#4370 = CARTESIAN_POINT ( 'NONE',  ( 3.662846001189864698, 218.4274158808046593, 45.39886208192143613 ) ) ;
#4371 = CARTESIAN_POINT ( 'NONE',  ( -6.220909254589682469, 215.4770327129947134, 44.94886208192143329 ) ) ;
#4372 = DIRECTION ( 'NONE',  ( 0.000000000000000000, 0.000000000000000000, -1.000000000000000000 ) ) ;
#4373 = CARTESIAN_POINT ( 'NONE',  ( 3.662846001190051659, 195.5725841191953691, 89.60113791807857808 ) ) ;
#4374 = CARTESIAN_POINT ( 'NONE',  ( 74.48867513459482836, 142.2402378747194405, -9.270509831248439525 ) ) ;
#4375 = CARTESIAN_POINT ( 'NONE',  ( 8.062137200540920645, 201.0835637161417822, 2.301137918078566269 ) ) ;
#4376 = CARTESIAN_POINT ( 'NONE',  ( -3.044812012439970683, 197.4746971517856196, 73.89886208192143613 ) ) ;
#4377 = CARTESIAN_POINT ( 'NONE',  ( 89.50000000000002842, 155.0000000000000000, 0.000000000000000000 ) ) ;
#4378 = EDGE_LOOP ( 'NONE', ( #20165, #13924, #27388, #19802 ) ) ;
#4379 = CARTESIAN_POINT ( 'NONE',  ( 3.662846001189864698, 218.4274158808046593, 72.39886208192143613 ) ) ;
#4380 = ORIENTED_EDGE ( 'NONE', *, *, #23746, .T. ) ;
#4381 = CARTESIAN_POINT ( 'NONE',  ( 72.77499999726882152, 140.1801316387863778, 4.815267126137185549 ) ) ;
#4382 = CARTESIAN_POINT ( 'NONE',  ( -4.984841277089891776, 213.7757310962905990, 41.94886208192144750 ) ) ;
#4383 = ORIENTED_EDGE ( 'NONE', *, *, #32414, .T. ) ;
#4384 = CARTESIAN_POINT ( 'NONE',  ( 83.07499999726880446, 141.7447067706911810, -9.630534252274387086 ) ) ;
#4385 = LINE ( 'NONE', #22439, #15693 ) ;
#4386 = DIRECTION ( 'NONE',  ( -1.000000000000000000, -0.000000000000000000, -0.000000000000000000 ) ) ;
#4387 = CARTESIAN_POINT ( 'NONE',  ( 54.82499999726879736, 141.7447067706911810, -9.630534252274385310 ) ) ;
#4388 = DIRECTION ( 'NONE',  ( 0.000000000000000000, 1.000000000000000000, -6.454785026890489601E-15 ) ) ;
#4389 = ADVANCED_FACE ( 'NONE', ( #21497 ), #8551, .T. ) ;
#4390 = CARTESIAN_POINT ( 'NONE',  ( 10.00000000000000711, 207.0476921513415220, 42.99886208192143044 ) ) ;
#4391 = VERTEX_POINT ( 'NONE', #13996 ) ;
#4392 = CARTESIAN_POINT ( 'NONE',  ( 125.0000000000000000, -24.99999999999995737, -35.00000000000000000 ) ) ;
#4393 = CARTESIAN_POINT ( 'NONE',  ( -0.04050535873993951069, -7.919512791578242172, -6.573129608219095310 ) ) ;
#4394 = CARTESIAN_POINT ( 'NONE',  ( 62.70000000000001705, -88.00000000000000000, 20.00000000000000000 ) ) ;
#4395 = CARTESIAN_POINT ( 'NONE',  ( 6.444103211790928043, 211.7408657792734061, 24.69886208192143684 ) ) ;
#4396 = EDGE_CURVE ( 'NONE', #29530, #21869, #24392, .T. ) ;
#4397 = CARTESIAN_POINT ( 'NONE',  ( -6.220909254589537696, 198.5229672870051161, 60.05113791807855961 ) ) ;
#4398 = EDGE_CURVE ( 'NONE', #171, #13101, #11448, .T. ) ;
#4399 = CARTESIAN_POINT ( 'NONE',  ( -3.044812012440131443, 216.5253028482142952, 46.10113791807857098 ) ) ;
#4400 = CONTEXT_DEPENDENT_SHAPE_REPRESENTATION ( #11619, #18237 ) ;
#4401 = CARTESIAN_POINT ( 'NONE',  ( 6.220909254589536808, 215.4770327129947702, 19.55113791807856671 ) ) ;
#4402 = CARTESIAN_POINT ( 'NONE',  ( 4.984841277089725686, 213.7757310962907411, 4.551137918078565825 ) ) ;
#4403 = CARTESIAN_POINT ( 'NONE',  ( 46.92499999726881299, 145.8408176439707802, -12.60653300113719588 ) ) ;
#4404 = CARTESIAN_POINT ( 'NONE',  ( 0.000000000000000000, 0.000000000000000000, -0.5251556536572846712 ) ) ;
#4405 = DIRECTION ( 'NONE',  ( -1.000000000000000000, 0.000000000000000000, 0.000000000000000000 ) ) ;
#4406 = CARTESIAN_POINT ( 'NONE',  ( -0.05014649552807705357, 194.3824533091408000, 32.75113791807856956 ) ) ;
#4407 = CARTESIAN_POINT ( 'NONE',  ( -0.3755270751584372513, 206.7692714347155629, 108.3323677711371573 ) ) ;
#4408 = CARTESIAN_POINT ( 'NONE',  ( 8.062137200540920645, 201.0835637161417822, 74.30113791807858092 ) ) ;
#4409 = CARTESIAN_POINT ( 'NONE',  ( -3.044812012440131443, 216.5253028482142952, 52.10113791807857808 ) ) ;
#4410 = CARTESIAN_POINT ( 'NONE',  ( 101.3062541159399075, 155.0000000000000000, 0.000000000000000000 ) ) ;
#4411 = CARTESIAN_POINT ( 'NONE',  ( 115.4999999999999858, 244.6486928011512134, 52.99999999999884892 ) ) ;
#4412 = CARTESIAN_POINT ( 'NONE',  ( -7.456977232089471386, 217.1783343296987709, 11.94886208192143506 ) ) ;
#4413 = CARTESIAN_POINT ( 'NONE',  ( 3.135527875058981895, 197.5041725223112792, 19.59886208192143542 ) ) ;
#4414 = TOROIDAL_SURFACE ( 'NONE', #8240, 10.12668159690567649, 0.7733184030943209830 ) ;
#4415 = CARTESIAN_POINT ( 'NONE',  ( 75.79999999453762882, 146.4771138417591203, -11.73074641843674470 ) ) ;
#4416 = VERTEX_POINT ( 'NONE', #29845 ) ;
#4417 = CARTESIAN_POINT ( 'NONE',  ( 7.375838497908181246, 196.7627149292499666, 62.45113791807857240 ) ) ;
#4418 = CARTESIAN_POINT ( 'NONE',  ( 2.517493886308900919, 214.5937144450984420, 76.40113791807856103 ) ) ;
#4419 = CARTESIAN_POINT ( 'NONE',  ( 0.05014649552828275708, 196.4853777576173002, 31.74886208192143044 ) ) ;
#4420 = FACE_OUTER_BOUND ( 'NONE', #15159, .T. ) ;
#4421 = ORIENTED_EDGE ( 'NONE', *, *, #14399, .F. ) ;
#4422 = ORIENTED_EDGE ( 'NONE', *, *, #13855, .T. ) ;
#4423 = ORIENTED_EDGE ( 'NONE', *, *, #26819, .T. ) ;
#4424 = DIRECTION ( 'NONE',  ( -1.000000000000000000, -1.804112415015879378E-16, -0.000000000000000000 ) ) ;
#4425 = FACE_OUTER_BOUND ( 'NONE', #7153, .T. ) ;
#4426 = EDGE_LOOP ( 'NONE', ( #26831, #11930, #30542, #23954 ) ) ;
#4427 = CARTESIAN_POINT ( 'NONE',  ( -8.000000000000008882, 207.0476921513413515, 30.50113791807856600 ) ) ;
#4428 = CARTESIAN_POINT ( 'NONE',  ( 85.01132485994281751, 142.2402378747194405, 9.270509831248432420 ) ) ;
#4429 = CARTESIAN_POINT ( 'NONE',  ( 6.139770520408223575, 215.5359834540460611, 18.54886208192143826 ) ) ;
#4430 = CARTESIAN_POINT ( 'NONE',  ( 57.27499999726882152, 149.9369285172503510, -15.58253175000000823 ) ) ;
#4431 = EDGE_LOOP ( 'NONE', ( #20479, #3207, #22862, #15414 ) ) ;
#4432 = CARTESIAN_POINT ( 'NONE',  ( -6.444103211791042618, 211.7408657792732356, 45.80113791807857382 ) ) ;
#4433 = DIRECTION ( 'NONE',  ( 0.000000000000000000, 0.000000000000000000, -1.000000000000000000 ) ) ;
#4434 = AXIS2_PLACEMENT_3D ( 'NONE', #13167, #31559, #231 ) ;
#4435 = CARTESIAN_POINT ( 'NONE',  ( 77.50000000000000000, 155.0000000000000000, -13.50000000000001776 ) ) ;
#4436 = CARTESIAN_POINT ( 'NONE',  ( 9.984503880673420539, 210.2968891136705167, 99.84886208192141055 ) ) ;
#4437 = CARTESIAN_POINT ( 'NONE',  ( 66.27499999726880731, 160.0630714827496206, 15.58253174999999402 ) ) ;
#4438 = CARTESIAN_POINT ( 'NONE',  ( -6.139770520408369237, 215.5359834540460042, 30.95113791807857240 ) ) ;
#4439 = CARTESIAN_POINT ( 'NONE',  ( 32.50000000000000000, 155.0000000000000000, -6.938893903907228378E-15 ) ) ;
#4440 = CARTESIAN_POINT ( 'NONE',  ( 8.118202686958039038, 212.8392687619912635, 19.70113791807856884 ) ) ;
#4441 = CARTESIAN_POINT ( 'NONE',  ( 132.3999999999999773, 154.9999999999996305, -106.0000000000000142 ) ) ;
#4442 = AXIS2_PLACEMENT_3D ( 'NONE', #15260, #7433, #28384 ) ;
#4443 = CARTESIAN_POINT ( 'NONE',  ( 80.50000000000000000, 155.0000000000000000, -14.50000000000000711 ) ) ;
#4444 = CARTESIAN_POINT ( 'NONE',  ( -56.01598787314604522, 194.9989914758641305, 0.3258944654411097264 ) ) ;
#4445 = DIRECTION ( 'NONE',  ( 0.000000000000000000, 0.000000000000000000, -1.000000000000000000 ) ) ;
#4446 = CARTESIAN_POINT ( 'NONE',  ( 12.00000000000000711, 206.9523078486586485, 2.001137918078565114 ) ) ;
#4447 = CARTESIAN_POINT ( 'NONE',  ( 82.78867513459482552, 155.0000000000000000, -15.00000000000002487 ) ) ;
#4448 = CARTESIAN_POINT ( 'NONE',  ( 51.77499999726881441, 169.8198683612136222, -4.815267126137197984 ) ) ;
#4449 = CARTESIAN_POINT ( 'NONE',  ( 6.139770520408368348, 198.4640165459539674, 50.45113791807857240 ) ) ;
#4450 = CARTESIAN_POINT ( 'NONE',  ( 84.02499999726882152, 160.0630714827496206, 15.58253174999999402 ) ) ;
#4451 = CARTESIAN_POINT ( 'NONE',  ( -52.50000000000002132, 120.3589838486224579, -20.00000000000000000 ) ) ;
#4452 = CARTESIAN_POINT ( 'NONE',  ( -1.250000000000000444, -7.938566201357367902, -7.198902722707430257 ) ) ;
#4453 = CARTESIAN_POINT ( 'NONE',  ( 52.29999999453762882, 167.3344367211045096, -8.961492836873482304 ) ) ;
#4454 = ORIENTED_EDGE ( 'NONE', *, *, #1406, .F. ) ;
#4455 = CARTESIAN_POINT ( 'NONE',  ( 3.662846001190051659, 195.5725841191953691, 29.60113791807856742 ) ) ;
#4456 = B_SPLINE_CURVE_WITH_KNOTS ( 'NONE', 3,
 ( #25551, #12598, #23663, #20616 ),
 .UNSPECIFIED., .F., .F.,
 ( 4, 4 ),
 ( 0.000000000000000000, 0.004600009204204579850 ),
 .UNSPECIFIED. ) ;
#4457 = DIRECTION ( 'NONE',  ( 0.000000000000000000, 0.000000000000000000, -1.000000000000000000 ) ) ;
#4458 = CARTESIAN_POINT ( 'NONE',  ( -10.00000000000000711, 206.9523078486584495, 5.498862081921434886 ) ) ;
#4459 = LINE ( 'NONE', #4116, #6344 ) ;
#4460 = ORIENTED_EDGE ( 'NONE', *, *, #30545, .F. ) ;
#4461 = VECTOR ( 'NONE', #12793, 1000.000000000000000 ) ;
#4462 = CARTESIAN_POINT ( 'NONE',  ( -8.118202686958039038, 201.1607312380087080, 0.2011379180785657361 ) ) ;
#4463 = CARTESIAN_POINT ( 'NONE',  ( -3.135527875058821579, 197.5041725223112223, 65.90113791807857524 ) ) ;
#4464 = ORIENTED_EDGE ( 'NONE', *, *, #14579, .T. ) ;
#4465 = CARTESIAN_POINT ( 'NONE',  ( 8.000000000000008882, 207.0476921513415220, 27.99886208192144110 ) ) ;
#4466 = DIRECTION ( 'NONE',  ( 1.000000000000000000, -0.000000000000000000, -0.000000000000000000 ) ) ;
#4467 = ORIENTED_EDGE ( 'NONE', *, *, #6484, .F. ) ;
#4468 = VECTOR ( 'NONE', #5652, 1000.000000000000000 ) ;
#4469 = CARTESIAN_POINT ( 'NONE',  ( -4.903702542908602524, 213.8346818373418898, 0.9511379180785658471 ) ) ;
#4470 = CARTESIAN_POINT ( 'NONE',  ( -0.5984201754795734907, -8.314755988442763979, -0.7022220667781372549 ) ) ;
#4471 = CARTESIAN_POINT ( 'NONE',  ( 9.736236675708031640, 199.9851607334238963, 91.29886208192142760 ) ) ;
#4472 = CARTESIAN_POINT ( 'NONE',  ( 34.47499999726881015, 149.9369285172503510, 15.58253174999999580 ) ) ;
#4473 = VERTEX_POINT ( 'NONE', #16883 ) ;
#4474 = CARTESIAN_POINT ( 'NONE',  ( 46.92499999726881299, 145.8408176439707802, -12.60653300113719588 ) ) ;
#4475 = CARTESIAN_POINT ( 'NONE',  ( 32.50000000000000000, 155.0000000000000000, -15.00000000000002487 ) ) ;
#4476 = CARTESIAN_POINT ( 'NONE',  ( 3.044812012440130555, 197.4746971517856764, -0.3988620819214342972 ) ) ;
#4477 = CARTESIAN_POINT ( 'NONE',  ( 10.01549611932659545, 203.7984951890123853, 67.14886208192143613 ) ) ;
#4478 = CARTESIAN_POINT ( 'NONE',  ( 50.07499999726881157, 168.2552932293087906, 9.630534252274372875 ) ) ;
#4479 = CARTESIAN_POINT ( 'NONE',  ( -31.74999999999995737, 0.000000000000000000, 0.000000000000000000 ) ) ;
#4480 = CARTESIAN_POINT ( 'NONE',  ( 9.984503880673470277, 203.7031108863295401, 8.151137918078564581 ) ) ;
#4481 = CARTESIAN_POINT ( 'NONE',  ( 6.500000000000000000, 1.602771114417268050, -0.1495523863686167576 ) ) ;
#4482 = AXIS2_PLACEMENT_3D ( 'NONE', #6020, #27447, #6666 ) ;
#4483 = CARTESIAN_POINT ( 'NONE',  ( 58.70000000000000284, 163.5228861582408797, -11.73074641843674470 ) ) ;
#4484 = CARTESIAN_POINT ( 'NONE',  ( -6.139770520408369237, 215.5359834540460042, 90.95113791807854398 ) ) ;
#4485 = PLANE ( 'NONE',  #31103 ) ;
#4486 = CARTESIAN_POINT ( 'NONE',  ( 9.984503880673470277, 203.7031108863295401, 77.15113791807857524 ) ) ;
#4487 = DIRECTION ( 'NONE',  ( 0.000000000000000000, 0.000000000000000000, 1.000000000000000000 ) ) ;
#4488 = PLANE ( 'NONE',  #9579 ) ;
#4489 = CARTESIAN_POINT ( 'NONE',  ( 9.736236675708031640, 199.9851607334238963, 85.29886208192145602 ) ) ;
#4490 = EDGE_CURVE ( 'NONE', #1916, #18599, #24575, .T. ) ;
#4491 = CARTESIAN_POINT ( 'NONE',  ( 61.72499999726881015, 169.8198683612136222, 4.815267126137181997 ) ) ;
#4493 = ORIENTED_EDGE ( 'NONE', *, *, #25434, .T. ) ;
#4492 = CARTESIAN_POINT ( 'NONE',  ( 8.118202686958039038, 212.8392687619912635, 19.70113791807856884 ) ) ;
#4494 = CYLINDRICAL_SURFACE ( 'NONE', #20634, 2.500000000000000000 ) ;
#4495 = CIRCLE ( 'NONE', #5059, 0.2000000000000000944 ) ;
#4496 = CARTESIAN_POINT ( 'NONE',  ( 81.37499999726881583, 155.0000000000000000, -15.58253175000000823 ) ) ;
#4497 = CARTESIAN_POINT ( 'NONE',  ( 9.736236675707914401, 214.0148392665762458, 82.70113791807858661 ) ) ;
#4498 = VECTOR ( 'NONE', #22056, 1000.000000000000000 ) ;
#4499 = LINE ( 'NONE', #28006, #21896 ) ;
#4500 = EDGE_LOOP ( 'NONE', ( #6558, #20766, #11342, #4422 ) ) ;
#4501 = CARTESIAN_POINT ( 'NONE',  ( -7.456977232089471386, 217.1783343296987709, 68.94886208192144750 ) ) ;
#4502 = CARTESIAN_POINT ( 'NONE',  ( 10.01549611932659367, 203.7984951890124421, 76.14886208192143613 ) ) ;
#4503 = CARTESIAN_POINT ( 'NONE',  ( 9.736236675708031640, 199.9851607334238963, 10.29886208192143471 ) ) ;
#4504 = DIRECTION ( 'NONE',  ( 1.000000000000000000, 0.000000000000000000, 0.000000000000000000 ) ) ;
#4505 = CARTESIAN_POINT ( 'NONE',  ( 3.135527875058820690, 216.4958274776887492, 31.40113791807857524 ) ) ;
#4506 = CARTESIAN_POINT ( 'NONE',  ( -67.50000000000000000, 155.0000000000000000, 6.938893903907228378E-15 ) ) ;
#4507 = CARTESIAN_POINT ( 'NONE',  ( -0.05014649552828403384, 217.5146222423826714, 102.2488620819214020 ) ) ;
#4508 = AXIS2_PLACEMENT_3D ( 'NONE', #3235, #682, #11084 ) ;
#4509 = CARTESIAN_POINT ( 'NONE',  ( 0.9108756637626340691, 6.979659189792313256, -6.219623095964331050 ) ) ;
#4510 = VERTEX_POINT ( 'NONE', #11121 ) ;
#4511 = DIRECTION ( 'NONE',  ( 0.000000000000000000, 0.000000000000000000, -1.000000000000000000 ) ) ;
#4512 = CARTESIAN_POINT ( 'NONE',  ( -0.05014649552828365914, 215.4116977939061144, 84.24886208192143044 ) ) ;
#4513 = VERTEX_POINT ( 'NONE', #26768 ) ;
#4514 = CARTESIAN_POINT ( 'NONE',  ( 117.5000000000000000, 207.9999999999998010, -89.64869280115065919 ) ) ;
#4515 = ORIENTED_EDGE ( 'NONE', *, *, #26989, .T. ) ;
#4516 = CARTESIAN_POINT ( 'NONE',  ( 7.777900015783946408, 4.169681370001526055, -7.928862157988300297 ) ) ;
#4517 = CONICAL_SURFACE ( 'NONE', #19736, 3.499999999999999556, 1.047197551196589638 ) ;
#4518 = EDGE_CURVE ( 'NONE', #11179, #24063, #32218, .T. ) ;
#4519 = VECTOR ( 'NONE', #22349, 1000.000000000000000 ) ;
#4520 = CARTESIAN_POINT ( 'NONE',  ( 72.97499999726881015, 140.1801316387863778, -4.815267126137194431 ) ) ;
#4521 = CARTESIAN_POINT ( 'NONE',  ( 80.22499999726881015, 149.9369285172503510, 15.58253174999999580 ) ) ;
#4522 = DIRECTION ( 'NONE',  ( 0.000000000000000000, 0.000000000000000000, -1.000000000000000000 ) ) ;
#4523 = CARTESIAN_POINT ( 'NONE',  ( -2.426778023690262742, 214.6231898156240163, 79.10113791807857808 ) ) ;
#4524 = CARTESIAN_POINT ( 'NONE',  ( 75.68867513459480278, 159.8737954434933499, 15.00000000000019895 ) ) ;
#4525 =( LENGTH_UNIT ( ) NAMED_UNIT ( * ) SI_UNIT ( .MILLI., .METRE. ) );
#4526 = CARTESIAN_POINT ( 'NONE',  ( 43.89999999999999858, 141.2096805137202580, 4.480746418436733158 ) ) ;
#4527 = CARTESIAN_POINT ( 'NONE',  ( 8.000000000000008882, 207.0476921513415220, 54.99886208192145176 ) ) ;
#4528 = EDGE_CURVE ( 'NONE', #21688, #31784, #28925, .T. ) ;
#4529 = DIRECTION ( 'NONE',  ( -1.000000000000000000, 0.000000000000000000, 0.000000000000000000 ) ) ;
#4530 = CARTESIAN_POINT ( 'NONE',  ( -0.3755270751584372513, 206.2625674640609645, 118.9447509161623344 ) ) ;
#4531 = CARTESIAN_POINT ( 'NONE',  ( -119.7500000000000000, -6.429395695523609083E-16, 35.00000599999999906 ) ) ;
#4532 = CARTESIAN_POINT ( 'NONE',  ( 55.92499999726881299, 164.1591823560292198, 12.60653300113718167 ) ) ;
#4533 = CARTESIAN_POINT ( 'NONE',  ( 62.37499999726880873, 155.0000000000000000, 15.58253174999999402 ) ) ;
#4534 = PRESENTATION_LAYER_ASSIGNMENT (  '', '', ( #3457 ) ) ;
#4535 = CARTESIAN_POINT ( 'NONE',  ( -7.375838497908182134, 217.2372850707499765, 57.95113791807855819 ) ) ;
#4536 = DIRECTION ( 'NONE',  ( 0.5526942671207055735, 0.1536855300543024383, 0.8190908404712107238 ) ) ;
#4537 = PRODUCT_DEFINITION_SHAPE ( 'NONE', 'NONE',  #1660 ) ;
#4538 = CARTESIAN_POINT ( 'NONE',  ( -3.662846001190052991, 218.4274158808045740, 1.101137918078565647 ) ) ;
#4539 = CARTESIAN_POINT ( 'NONE',  ( -6.220909254589537696, 198.5229672870051445, 81.05113791807858092 ) ) ;
#4540 = EDGE_CURVE ( 'NONE', #2760, #23658, #27296, .T. ) ;
#4541 = CARTESIAN_POINT ( 'NONE',  ( -0.05014649552828442242, 219.6175466908591716, 42.24886208192143044 ) ) ;
#4542 = CARTESIAN_POINT ( 'NONE',  ( 8.118202686958138514, 201.1607312380088501, 46.29886208192143471 ) ) ;
#4543 = CARTESIAN_POINT ( 'NONE',  ( 2.000000000000000000, 1.773042676681340968, -2.276824562219559311E-15 ) ) ;
#4544 = TOROIDAL_SURFACE ( 'NONE', #18149, 3.299999999999999822, 0.2000000000000000111 ) ;
#4545 = CARTESIAN_POINT ( 'NONE',  ( 0.05014649552807549926, 219.6175466908591716, 88.25113791807856956 ) ) ;
#4546 = CARTESIAN_POINT ( 'NONE',  ( 67.91132485994280898, 163.8167787843871110, -12.13525491562423397 ) ) ;
#4547 = CARTESIAN_POINT ( 'NONE',  ( 8.118202686958039038, 212.8392687619912635, 4.701137918078565292 ) ) ;
#4548 = AXIS2_PLACEMENT_3D ( 'NONE', #31582, #8247, #11798 ) ;
#4549 = CARTESIAN_POINT ( 'NONE',  ( -8.062137200540822946, 201.0835637161416400, 65.19886208192143329 ) ) ;
#4550 = AXIS2_PLACEMENT_3D ( 'NONE', #2962, #24060, #732 ) ;
#4551 = DIRECTION ( 'NONE',  ( -1.000000000000000000, 0.000000000000000000, 0.000000000000000000 ) ) ;
#4552 = ORIENTED_EDGE ( 'NONE', *, *, #13261, .F. ) ;
#4553 = CARTESIAN_POINT ( 'NONE',  ( -7.375838497908014268, 196.7627149292498530, 68.04886208192144181 ) ) ;
#4554 = ORIENTED_EDGE ( 'NONE', *, *, #12518, .T. ) ;
#4555 = CARTESIAN_POINT ( 'NONE',  ( 75.37499999726881583, 155.0000000000000000, -15.58253175000000823 ) ) ;
#4556 = CARTESIAN_POINT ( 'NONE',  ( -8.015496119326597224, 209.5516654185217362, 53.64886208192143613 ) ) ;
#4557 = ORIENTED_EDGE ( 'NONE', *, *, #7388, .F. ) ;
#4558 = EDGE_CURVE ( 'NONE', #4641, #16283, #10980, .T. ) ;
#4559 = CARTESIAN_POINT ( 'NONE',  ( 72.52499999726882152, 140.1801316387863778, 4.815267126137185549 ) ) ;
#4560 = FACE_BOUND ( 'NONE', #31244, .T. ) ;
#4561 = CARTESIAN_POINT ( 'NONE',  ( -3.978477517404915176, -5.573260695678958321, -6.171287963165198676 ) ) ;
#4562 = ADVANCED_FACE ( 'NONE', ( #22847 ), #32721, .F. ) ;
#4563 = CARTESIAN_POINT ( 'NONE',  ( 54.92499999726881299, 145.8408176439707802, -12.60653300113719588 ) ) ;
#4564 = FACE_OUTER_BOUND ( 'NONE', #32871, .T. ) ;
#4565 = CARTESIAN_POINT ( 'NONE',  ( -8.062137200540822946, 201.0835637161416400, 44.19886208192143329 ) ) ;
#4566 = ORIENTED_EDGE ( 'NONE', *, *, #8901, .F. ) ;
#4567 = DIRECTION ( 'NONE',  ( -1.000000000000000000, 0.000000000000000000, 0.000000000000000000 ) ) ;
#4568 = COLOUR_RGB ( '', 0.09019608, 0.27058824, 0.51372549) ;
#4569 = CARTESIAN_POINT ( 'NONE',  ( 0.8808064505790902388, -6.997019658119350005, -5.875704392893848826 ) ) ;
#4570 = CARTESIAN_POINT ( 'NONE',  ( 125.0000000000000000, 3.061616997868383121E-14, 20.00000000000000000 ) ) ;
#4571 = CARTESIAN_POINT ( 'NONE',  ( -4.903702542908436435, 200.1653181626580249, 29.04886208192143471 ) ) ;
#4572 = VECTOR ( 'NONE', #8993, 1000.000000000000000 ) ;
#4573 = CARTESIAN_POINT ( 'NONE',  ( -9.984503880673473830, 210.2968891136704315, 66.65113791807857524 ) ) ;
#4574 = FACE_OUTER_BOUND ( 'NONE', #24318, .T. ) ;
#4575 = CARTESIAN_POINT ( 'NONE',  ( 6.139770520408368348, 198.4640165459539674, 50.45113791807857240 ) ) ;
#4576 = CARTESIAN_POINT ( 'NONE',  ( -10.00000000000000711, 207.0476921513413515, 21.50113791807856956 ) ) ;
#4577 = CARTESIAN_POINT ( 'NONE',  ( -2.517493886308901807, 199.4062855549015012, 2.901137918078565914 ) ) ;
#4578 = FACE_OUTER_BOUND ( 'NONE', #30029, .T. ) ;
#4579 = DIRECTION ( 'NONE',  ( 1.000000000000000000, 0.000000000000000000, 0.000000000000000000 ) ) ;
#4580 = CARTESIAN_POINT ( 'NONE',  ( 7.375838497908181246, 196.7627149292499666, 26.45113791807857240 ) ) ;
#4581 = CARTESIAN_POINT ( 'NONE',  ( 64.50000000000000000, -73.00000000000000000, 20.00000000000000000 ) ) ;
#4582 = CARTESIAN_POINT ( 'NONE',  ( -3.135527875058821579, 197.5041725223112223, 74.90113791807857524 ) ) ;
#4583 = CARTESIAN_POINT ( 'NONE',  ( -0.05014649552810635652, 196.4853777576173002, 50.75113791807856956 ) ) ;
#4584 = UNCERTAINTY_MEASURE_WITH_UNIT (LENGTH_MEASURE( 1.000000000000000082E-05 ), #13398, 'distance_accuracy_value', 'NONE');
#4585 = CARTESIAN_POINT ( 'NONE',  ( 125.0000000000000000, -24.99999999999995737, 35.00000000000000000 ) ) ;
#4586 = COLOUR_RGB ( '', 0.72549020, 0.75294118, 0.79215686) ;
#4587 = CARTESIAN_POINT ( 'NONE',  ( -58.50000000000002132, 185.0000000000000000, 2.500000000000000000 ) ) ;
#4588 = CARTESIAN_POINT ( 'NONE',  ( 3.753561863808876797, 195.6020594897209719, 13.59886208192143719 ) ) ;
#4589 = CARTESIAN_POINT ( 'NONE',  ( 8.118202686958138514, 201.1607312380088501, 22.29886208192143826 ) ) ;
#4590 = CARTESIAN_POINT ( 'NONE',  ( 73.99999999453763166, 155.0000000000000000, -14.50000000000000711 ) ) ;
#4591 = ORIENTED_EDGE ( 'NONE', *, *, #29161, .T. ) ;
#4592 = CARTESIAN_POINT ( 'NONE',  ( 7.456977232089302632, 217.1783343296989131, 55.55113791807858092 ) ) ;
#4593 = CARTESIAN_POINT ( 'NONE',  ( -6.500168698208129925, 202.3363017425936050, 81.20113791807858661 ) ) ;
#4594 = EDGE_CURVE ( 'NONE', #5483, #20223, #26450, .T. ) ;
#4595 = CARTESIAN_POINT ( 'NONE',  ( 8.062137200540822946, 212.9164362838583315, 42.69886208192143329 ) ) ;
#4596 = EDGE_CURVE ( 'NONE', #14298, #4983, #22508, .T. ) ;
#4597 = CARTESIAN_POINT ( 'NONE',  ( 75.31132485994281467, 140.7341522555726669, -4.635254915624220651 ) ) ;
#4598 = ORIENTED_EDGE ( 'NONE', *, *, #21604, .F. ) ;
#4599 = COLOUR_RGB ( '', 0.08235294, 0.09019608, 0.10196078) ;
#4600 = ORIENTED_EDGE ( 'NONE', *, *, #3552, .T. ) ;
#4601 = ORIENTED_EDGE ( 'NONE', *, *, #6376, .F. ) ;
#4602 = EDGE_CURVE ( 'NONE', #33380, #25118, #4982, .T. ) ;
#4603 = DIRECTION ( 'NONE',  ( 1.000000000000000000, -0.000000000000000000, -0.000000000000000000 ) ) ;
#4604 = CARTESIAN_POINT ( 'NONE',  ( 117.5000000000000000, 244.6486928011512134, 52.99999999999884892 ) ) ;
#4605 = ORIENTED_EDGE ( 'NONE', *, *, #13314, .T. ) ;
#4606 = CARTESIAN_POINT ( 'NONE',  ( 2.426778023690261410, 199.3768101843759837, 35.60113791807857098 ) ) ;
#4607 = EDGE_CURVE ( 'NONE', #5261, #21434, #9318, .T. ) ;
#4608 = DIRECTION ( 'NONE',  ( 0.5000000000000005551, -0.8660254037844383745, 0.000000000000000000 ) ) ;
#4609 = CARTESIAN_POINT ( 'NONE',  ( 3.135527875058981895, 197.5041725223112792, 10.59886208192143542 ) ) ;
#4610 = CARTESIAN_POINT ( 'NONE',  ( 55.37499999726881583, 155.0000000000000000, -15.58253175000000823 ) ) ;
#4611 = ORIENTED_EDGE ( 'NONE', *, *, #9801, .T. ) ;
#4612 = CARTESIAN_POINT ( 'NONE',  ( 4.903702542908601636, 200.1653181626581102, 56.45113791807857950 ) ) ;
#4613 = CARTESIAN_POINT ( 'NONE',  ( 110.1179863365115636, 155.0000000000000000, 0.000000000000000000 ) ) ;
#4614 =( GEOMETRIC_REPRESENTATION_CONTEXT ( 3 ) GLOBAL_UNCERTAINTY_ASSIGNED_CONTEXT ( ( #21276 ) ) GLOBAL_UNIT_ASSIGNED_CONTEXT ( ( #26679, #5566, #10693 ) ) REPRESENTATION_CONTEXT ( 'NONE', 'WORKASPACE' ) );
#4615 = CARTESIAN_POINT ( 'NONE',  ( 27.50000000000000355, 15.87713240271469317, -18.00000000000000000 ) ) ;
#4616 = CARTESIAN_POINT ( 'NONE',  ( -9.984503880673420539, 203.7031108863293980, 104.3488620819214105 ) ) ;
#4617 = CARTESIAN_POINT ( 'NONE',  ( 63.47499999726881725, 160.0630714827496206, -15.58253175000000823 ) ) ;
#4618 = CARTESIAN_POINT ( 'NONE',  ( -10.01549611932653860, 203.7984951890123284, 30.35113791807856742 ) ) ;
#4619 = CARTESIAN_POINT ( 'NONE',  ( 125.0000000000000000, 4.592425496802574367E-14, 35.00000000000000000 ) ) ;
#4620 = CARTESIAN_POINT ( 'NONE',  ( -3.044812012440131443, 216.5253028482142952, 19.10113791807856742 ) ) ;
#4621 = DIRECTION ( 'NONE',  ( 1.000000000000000000, 0.000000000000000000, 0.000000000000000000 ) ) ;
#4622 = CARTESIAN_POINT ( 'NONE',  ( 86.29999999999999716, 146.4771138417591203, -11.73074641843674470 ) ) ;
#4623 = LINE ( 'NONE', #12281, #19794 ) ;
#4624 = CARTESIAN_POINT ( 'NONE',  ( -4.945910536743085117, 206.2642604888503968, -6.000000000000014211 ) ) ;
#4625 = CARTESIAN_POINT ( 'NONE',  ( 6.220909254589536808, 215.4770327129947702, 100.5511379180785809 ) ) ;
#4626 = DIRECTION ( 'NONE',  ( 1.000000000000000000, 0.000000000000000000, 0.000000000000000000 ) ) ;
#4627 = CARTESIAN_POINT ( 'NONE',  ( 52.87499999726880162, 138.6155565068815463, -3.929120461958505118E-15 ) ) ;
#4628 = CARTESIAN_POINT ( 'NONE',  ( -8.118202686958039038, 201.1607312380087080, 48.20113791807857950 ) ) ;
#4629 = CARTESIAN_POINT ( 'NONE',  ( 84.32499999726880446, 145.8408176439707802, 12.60653300113718345 ) ) ;
#4630 = CARTESIAN_POINT ( 'NONE',  ( 42.61132485994281893, 159.8737954434936341, 14.99999999999998934 ) ) ;
#4631 = DIRECTION ( 'NONE',  ( 1.000000000000000000, 0.000000000000000000, -0.000000000000000000 ) ) ;
#4632 = CARTESIAN_POINT ( 'NONE',  ( 52.19999999453762740, 163.5228861582408797, -11.73074641843674470 ) ) ;
#4633 = VERTEX_POINT ( 'NONE', #9388 ) ;
#4634 = CARTESIAN_POINT ( 'NONE',  ( -3.753561863808691168, 195.6020594897209435, 32.90113791807856813 ) ) ;
#4635 = DIRECTION ( 'NONE',  ( -0.000000000000000000, -0.000000000000000000, -1.000000000000000000 ) ) ;
#4636 = CARTESIAN_POINT ( 'NONE',  ( -3.135527875058982783, 216.4958274776886924, 15.09886208192143542 ) ) ;
#4637 = DIRECTION ( 'NONE',  ( 0.000000000000000000, 0.000000000000000000, -1.000000000000000000 ) ) ;
#4638 = ORIENTED_EDGE ( 'NONE', *, *, #25487, .F. ) ;
#4639 = CARTESIAN_POINT ( 'NONE',  ( -6.139770520408369237, 215.5359834540460042, 3.951137918078566180 ) ) ;
#4640 = CARTESIAN_POINT ( 'NONE',  ( 0.05014649552810505201, 217.5146222423826714, 58.25113791807856245 ) ) ;
#4641 = VERTEX_POINT ( 'NONE', #19784 ) ;
#4642 = CARTESIAN_POINT ( 'NONE',  ( 6.444103211790928043, 211.7408657792734061, 24.69886208192143684 ) ) ;
#4643 = DIRECTION ( 'NONE',  ( 1.000000000000000000, 0.000000000000000000, 0.000000000000000000 ) ) ;
#4644 = ORIENTED_EDGE ( 'NONE', *, *, #18831, .F. ) ;
#4645 = CARTESIAN_POINT ( 'NONE',  ( -4.984841277089726574, 200.2242689037092305, 6.051137918078566713 ) ) ;
#4646 = DIRECTION ( 'NONE',  ( 1.000000000000000000, 0.000000000000000000, 0.000000000000000000 ) ) ;
#4647 = CARTESIAN_POINT ( 'NONE',  ( -9.680171189290716072, 199.9079932115567146, 92.19886208192143329 ) ) ;
#4648 = CARTESIAN_POINT ( 'NONE',  ( 39.47499999726881015, 160.0630714827496206, -15.58253175000000823 ) ) ;
#4649 = ORIENTED_EDGE ( 'NONE', *, *, #2624, .T. ) ;
#4650 = CARTESIAN_POINT ( 'NONE',  ( 46.32499999726881157, 145.8408176439707802, 12.60653300113718345 ) ) ;
#4651 = DIRECTION ( 'NONE',  ( 0.000000000000000000, 0.8660254037844381525, -0.5000000000000008882 ) ) ;
#4652 = CARTESIAN_POINT ( 'NONE',  ( -6.220909254589537696, 198.5229672870051161, 0.05113791807856577637 ) ) ;
#4653 = CARTESIAN_POINT ( 'NONE',  ( -8.118202686958138514, 212.8392687619910930, 74.79886208192144181 ) ) ;
#4654 = CARTESIAN_POINT ( 'NONE',  ( 44.37499999726881583, 155.0000000000000000, 15.58253174999999402 ) ) ;
#4655 = CARTESIAN_POINT ( 'NONE',  ( 79.31132485994280046, 140.7341522555726669, -4.635254915624220651 ) ) ;
#4656 = CARTESIAN_POINT ( 'NONE',  ( -10.01549611932653860, 203.7984951890123284, 3.351137918078566091 ) ) ;
#4657 = CARTESIAN_POINT ( 'NONE',  ( 6.500000000000000000, 3.752776749732573247, -0.8000000000000003775 ) ) ;
#4658 =( REPRESENTATION_RELATIONSHIP ('NONE','NONE', #25663, #32622 ) REPRESENTATION_RELATIONSHIP_WITH_TRANSFORMATION ( #15297 )SHAPE_REPRESENTATION_RELATIONSHIP( ) );
#4659 = CARTESIAN_POINT ( 'NONE',  ( 62.19999999999999574, 142.6655632788954620, -8.961492836873480528 ) ) ;
#4660 = CARTESIAN_POINT ( 'NONE',  ( 9.984503880673470277, 203.7031108863295401, 92.15113791807856103 ) ) ;
#4661 = CARTESIAN_POINT ( 'NONE',  ( -2.343682934607786983, -2.688325911136475899, -0.02993401039715462217 ) ) ;
#4662 = CARTESIAN_POINT ( 'NONE',  ( 3.044812012440130555, 197.4746971517856764, 71.60113791807857808 ) ) ;
#4663 = DIRECTION ( 'NONE',  ( 0.000000000000000000, 1.000000000000000000, 0.000000000000000000 ) ) ;
#4664 = CARTESIAN_POINT ( 'NONE',  ( 105.9028607166213192, 155.0000000000000000, -32.10452846326769816 ) ) ;
#4665 = CARTESIAN_POINT ( 'NONE',  ( -12.00000000000000711, 206.9523078486584780, 86.49886208192144466 ) ) ;
#4666 = CARTESIAN_POINT ( 'NONE',  ( 62.32499999726881867, 145.8408176439707802, 12.60653300113718345 ) ) ;
#4668 = ORIENTED_EDGE ( 'NONE', *, *, #26852, .F. ) ;
#4667 = CARTESIAN_POINT ( 'NONE',  ( 3.044812012440130555, 197.4746971517856764, 29.60113791807856742 ) ) ;
#4669 = CARTESIAN_POINT ( 'NONE',  ( -60.02418147676856108, 194.9506531851598936, 1.988357156115594826 ) ) ;
#4670 = CARTESIAN_POINT ( 'NONE',  ( 87.67499999726882720, 168.2552932293087906, -9.630534252274385310 ) ) ;
#4671 = CARTESIAN_POINT ( 'NONE',  ( 7.375838497908181246, 196.7627149292499666, 95.45113791807858661 ) ) ;
#4672 = CARTESIAN_POINT ( 'NONE',  ( 72.38867513459481984, 140.7341522555726669, -4.635254915624220651 ) ) ;
#4673 = VERTEX_POINT ( 'NONE', #1554 ) ;
#4674 = CARTESIAN_POINT ( 'NONE',  ( -6.220909254589682469, 215.4770327129947134, 89.94886208192143329 ) ) ;
#4675 = CARTESIAN_POINT ( 'NONE',  ( -9.680171189290716072, 199.9079932115567146, 20.19886208192143684 ) ) ;
#4676 = CARTESIAN_POINT ( 'NONE',  ( -6.826425371444817536, 2.641426549045769345, -6.344843397090116355 ) ) ;
#4677 = CARTESIAN_POINT ( 'NONE',  ( 0.05014649552810505201, 217.5146222423826714, 37.25113791807855534 ) ) ;
#4678 = CARTESIAN_POINT ( 'NONE',  ( -64.50000000000000000, -95.00000000000000000, 270.4495957273638282 ) ) ;
#4679 = CARTESIAN_POINT ( 'NONE',  ( -3.044812012439970683, 197.4746971517856196, 94.89886208192143613 ) ) ;
#4680 = CARTESIAN_POINT ( 'NONE',  ( 5.619193549421086509, 4.261310591078260046, -5.875704392893767114 ) ) ;
#4681 = ORIENTED_EDGE ( 'NONE', *, *, #6446, .F. ) ;
#4682 = CARTESIAN_POINT ( 'NONE',  ( 69.71132485994280614, 155.0000000000000000, -15.00000000000002487 ) ) ;
#4683 = CARTESIAN_POINT ( 'NONE',  ( 2.517493886309087436, 199.4062855549015865, 79.59886208192143897 ) ) ;
#4684 = VERTEX_POINT ( 'NONE', #24894 ) ;
#4685 = ADVANCED_FACE ( 'NONE', ( #9555 ), #3358, .T. ) ;
#4686 = CARTESIAN_POINT ( 'NONE',  ( 34.71132485994281325, 155.0000000000000000, 15.00000000000001243 ) ) ;
#4687 = ORIENTED_EDGE ( 'NONE', *, *, #19753, .F. ) ;
#4688 = CARTESIAN_POINT ( 'NONE',  ( 72.99495483890930814, 155.0000000000000000, -6.938893903907228378E-15 ) ) ;
#4689 = CARTESIAN_POINT ( 'NONE',  ( 83.22499999726879594, 160.0630714827496206, -15.58253175000000823 ) ) ;
#4690 = CARTESIAN_POINT ( 'NONE',  ( 115.4999999999999858, 258.9084171661918958, -28.95509836041981444 ) ) ;
#4691 = CARTESIAN_POINT ( 'NONE',  ( 7.984503880673485376, 204.3529502787953902, 83.15113791807856103 ) ) ;
#4692 = CARTESIAN_POINT ( 'NONE',  ( 41.70000000000000284, 146.4771138417591203, 11.73074641843673227 ) ) ;
#4693 = CARTESIAN_POINT ( 'NONE',  ( 2.517493886309087436, 199.4062855549015865, 58.59886208192145318 ) ) ;
#4694 = AXIS2_PLACEMENT_3D ( 'NONE', #30527, #5140, #7369 ) ;
#4695 = CARTESIAN_POINT ( 'NONE',  ( 8.062137200540920645, 201.0835637161417822, 2.301137918078566269 ) ) ;
#4696 = DIRECTION ( 'NONE',  ( 0.000000000000000000, -0.7071067811865442421, 0.7071067811865506814 ) ) ;
#4697 = CARTESIAN_POINT ( 'NONE',  ( -129.5873785388598662, 2.643999646947224669, 35.00001200000000523 ) ) ;
#4698 = CARTESIAN_POINT ( 'NONE',  ( 56.32499999726881157, 145.8408176439707802, 12.60653300113718345 ) ) ;
#4699 = CARTESIAN_POINT ( 'NONE',  ( 70.77499999726880731, 140.1801316387863778, 4.815267126137185549 ) ) ;
#4700 = CARTESIAN_POINT ( 'NONE',  ( 7.375838497908181246, 196.7627149292499666, 62.45113791807857240 ) ) ;
#4701 = FACE_OUTER_BOUND ( 'NONE', #15033, .T. ) ;
#4702 = CARTESIAN_POINT ( 'NONE',  ( 7.456977232089302632, 217.1783343296989131, 10.55113791807856671 ) ) ;
#4703 = CARTESIAN_POINT ( 'NONE',  ( 0.05014649552810506589, 217.5146222423826714, 76.25113791807856956 ) ) ;
#4704 = CIRCLE ( 'NONE', #17769, 2.500000000000000000 ) ;
#4705 = CARTESIAN_POINT ( 'NONE',  ( -9.736236675708031640, 214.0148392665760753, 44.79886208192143471 ) ) ;
#4706 = CARTESIAN_POINT ( 'NONE',  ( -10.00000000000000711, 206.9523078486584495, 59.49886208192143755 ) ) ;
#4707 = CARTESIAN_POINT ( 'NONE',  ( -6.499999999999999112, 1.286902272306389428, -0.09436334093186068972 ) ) ;
#4708 = CARTESIAN_POINT ( 'NONE',  ( 9.736236675707914401, 214.0148392665762458, 88.70113791807857240 ) ) ;
#4709 = CARTESIAN_POINT ( 'NONE',  ( 74.28867513459483973, 139.2280666364260071, -4.041636747397287284E-15 ) ) ;
#4710 = CARTESIAN_POINT ( 'NONE',  ( 6.139770520408368348, 198.4640165459539674, 8.451137918078565292 ) ) ;
#4711 = CARTESIAN_POINT ( 'NONE',  ( 8.062137200540822946, 212.9164362838583315, 66.69886208192143329 ) ) ;
#4712 = LINE ( 'NONE', #2168, #24875 ) ;
#4713 = EDGE_LOOP ( 'NONE', ( #11471, #33174, #26340, #14353, #27131 ) ) ;
#4714 = CARTESIAN_POINT ( 'NONE',  ( -3.662846001189865142, 195.5725841191952838, 73.89886208192143613 ) ) ;
#4715 = ORIENTED_EDGE ( 'NONE', *, *, #2071, .T. ) ;
#4716 = CARTESIAN_POINT ( 'NONE',  ( 76.97499999726881015, 140.1801316387863778, -4.815267126137194431 ) ) ;
#4717 = CARTESIAN_POINT ( 'NONE',  ( -2.426778023690076225, 199.3768101843759553, 55.89886208192144323 ) ) ;
#4718 = ORIENTED_EDGE ( 'NONE', *, *, #16395, .F. ) ;
#4719 = EDGE_CURVE ( 'NONE', #27181, #10769, #22400, .T. ) ;
#4720 = AXIS2_PLACEMENT_3D ( 'NONE', #8649, #11206, #3363 ) ;
#4721 = CARTESIAN_POINT ( 'NONE',  ( 69.02499999726880731, 149.9369285172503510, -15.58253175000000823 ) ) ;
#4722 = DIRECTION ( 'NONE',  ( 1.000000000000000000, 0.000000000000000000, 0.000000000000000000 ) ) ;
#4723 = CIRCLE ( 'NONE', #6345, 31.00000000000000000 ) ;
#4724 = DIRECTION ( 'NONE',  ( 0.000000000000000000, 0.04769215134145521340, 0.9988620819214352187 ) ) ;
#4725 = CARTESIAN_POINT ( 'NONE',  ( 65.42499999726881299, 168.2552932293087906, -9.630534252274385310 ) ) ;
#4726 = DIRECTION ( 'NONE',  ( 0.000000000000000000, 0.000000000000000000, -1.000000000000000000 ) ) ;
#4727 = CARTESIAN_POINT ( 'NONE',  ( -3.135527875058982783, 216.4958274776886924, 39.09886208192143187 ) ) ;
#4728 = ORIENTED_EDGE ( 'NONE', *, *, #20197, .T. ) ;
#4729 = AXIS2_PLACEMENT_3D ( 'NONE', #2142, #12690, #15073 ) ;
#4730 = PLANE ( 'NONE',  #16189 ) ;
#4731 = EDGE_CURVE ( 'NONE', #29479, #22574, #30586, .T. ) ;
#4732 = CARTESIAN_POINT ( 'NONE',  ( 5.727634848075544127, -4.575561887445499742, -6.326622577869666308 ) ) ;
#4733 = CARTESIAN_POINT ( 'NONE',  ( 4.250000000000000000, 0.000000000000000000, -9.449444346342714240 ) ) ;
#4734 = CARTESIAN_POINT ( 'NONE',  ( -6.444103211790928043, 202.2591342207265939, 23.19886208192143684 ) ) ;
#4735 = CARTESIAN_POINT ( 'NONE',  ( -0.05014649552810635652, 196.4853777576173002, 68.75113791807855534 ) ) ;
#4736 = CARTESIAN_POINT ( 'NONE',  ( -10.01549611932653860, 203.7984951890123284, 48.35113791807855677 ) ) ;
#4737 = CONTEXT_DEPENDENT_SHAPE_REPRESENTATION ( #9428, #23676 ) ;
#4738 = CARTESIAN_POINT ( 'NONE',  ( -3.135527875058821579, 197.5041725223112223, 20.90113791807856813 ) ) ;
#4739 = CARTESIAN_POINT ( 'NONE',  ( -7.984503880673488041, 209.6470497212046098, 9.651137918078566358 ) ) ;
#4740 = CARTESIAN_POINT ( 'NONE',  ( 38.92499999726881299, 145.8408176439707802, -12.60653300113719588 ) ) ;
#4741 = CARTESIAN_POINT ( 'NONE',  ( 3.753561863808689836, 218.3979405102790565, 25.40113791807857169 ) ) ;
#4742 = CARTESIAN_POINT ( 'NONE',  ( 0.000000000000000000, 0.000000000000000000, -25.03750572909317285 ) ) ;
#4743 = AXIS2_PLACEMENT_3D ( 'NONE', #26593, #31713, #31873 ) ;
#4744 = ADVANCED_FACE ( 'NONE', ( #33061 ), #17222, .T. ) ;
#4745 = CARTESIAN_POINT ( 'NONE',  ( 6.139770520408368348, 198.4640165459539674, 71.45113791807857240 ) ) ;
#4746 = CARTESIAN_POINT ( 'NONE',  ( -3.135527875058821579, 197.5041725223112223, 44.90113791807857524 ) ) ;
#4747 = AXIS2_PLACEMENT_3D ( 'NONE', #28736, #23782, #3005 ) ;
#4748 = DIRECTION ( 'NONE',  ( 1.000000000000000000, 0.000000000000000000, 0.000000000000000000 ) ) ;
#4749 = CARTESIAN_POINT ( 'NONE',  ( 34.98867513459482126, 163.8167787843871110, -12.13525491562423397 ) ) ;
#4750 = CARTESIAN_POINT ( 'NONE',  ( -9.736236675708031640, 214.0148392665760753, 14.79886208192143471 ) ) ;
#4751 = CARTESIAN_POINT ( 'NONE',  ( 8.062137200540822946, 212.9164362838583315, 18.69886208192143329 ) ) ;
#4752 = CARTESIAN_POINT ( 'NONE',  ( 72.69999999453763451, 167.3344367211045096, 8.961492836873468093 ) ) ;
#4753 = ORIENTED_EDGE ( 'NONE', *, *, #9929, .F. ) ;
#4754 = CARTESIAN_POINT ( 'NONE',  ( -7.456977232089304408, 196.8216656703010301, 57.05113791807856671 ) ) ;
#4755 = CARTESIAN_POINT ( 'NONE',  ( -7.984503880673488041, 209.6470497212046098, 78.65113791807858945 ) ) ;
#4756 = EDGE_CURVE ( 'NONE', #6483, #25501, #10469, .T. ) ;
#4757 = CARTESIAN_POINT ( 'NONE',  ( 3.044812012439969795, 216.5253028482143520, 36.39886208192142902 ) ) ;
#4758 = CARTESIAN_POINT ( 'NONE',  ( -9.996365641501871124, 207.8097375604742467, 102.5363179372327096 ) ) ;
#4759 = VECTOR ( 'NONE', #4663, 1000.000000000000000 ) ;
#4760 = ORIENTED_EDGE ( 'NONE', *, *, #23511, .T. ) ;
#4761 = EDGE_LOOP ( 'NONE', ( #18178, #16576, #31300, #24192, #4605, #18975 ) ) ;
#4762 = ORIENTED_EDGE ( 'NONE', *, *, #17424, .T. ) ;
#4763 = CARTESIAN_POINT ( 'NONE',  ( 18.00000000000000711, 2.204364238465236217E-15, -17.97459999999999525 ) ) ;
#4764 = CARTESIAN_POINT ( 'NONE',  ( 3.250000000000004441, 5.629165124598849879, 0.000000000000000000 ) ) ;
#4765 = ORIENTED_EDGE ( 'NONE', *, *, #24869, .F. ) ;
#4766 = CARTESIAN_POINT ( 'NONE',  ( -8.000000000000008882, 207.0476921513413515, 33.50113791807857666 ) ) ;
#4767 = TOROIDAL_SURFACE ( 'NONE', #4747, 2.466666666666999408, 1.033333333332998372 ) ;
#4768 = CARTESIAN_POINT ( 'NONE',  ( 0.05014649552828275708, 196.4853777576173002, 10.74886208192143755 ) ) ;
#4769 = CARTESIAN_POINT ( 'NONE',  ( 55.57499999726881157, 164.1591823560292198, -12.60653300113719766 ) ) ;
#4770 = ORIENTED_EDGE ( 'NONE', *, *, #22643, .F. ) ;
#4771 = CARTESIAN_POINT ( 'NONE',  ( -2.426778023690262742, 214.6231898156240163, 58.10113791807857808 ) ) ;
#4772 = DIRECTION ( 'NONE',  ( 0.000000000000000000, -0.8660254037844390407, -0.4999999999999995004 ) ) ;
#4773 = CARTESIAN_POINT ( 'NONE',  ( -3.999999999999999112, 0.000000000000000000, -7.974599999999998801 ) ) ;
#4774 = CARTESIAN_POINT ( 'NONE',  ( 10.01549611932659545, 203.7984951890123853, 100.1488620819214077 ) ) ;
#4775 = CARTESIAN_POINT ( 'NONE',  ( 67.87499999726881583, 171.3844434931184253, -7.942151717890132712E-15 ) ) ;
#4776 = CARTESIAN_POINT ( 'NONE',  ( 3.135527875058820690, 216.4958274776887492, 40.40113791807857524 ) ) ;
#4777 = CARTESIAN_POINT ( 'NONE',  ( -6.826399921716642005, -2.638123634694629516, -6.344399053232583796 ) ) ;
#4778 = EDGE_CURVE ( 'NONE', #25118, #33380, #24597, .T. ) ;
#4779 = CARTESIAN_POINT ( 'NONE',  ( 6.220909254589536808, 215.4770327129947702, 13.55113791807856849 ) ) ;
#4780 = CARTESIAN_POINT ( 'NONE',  ( 3.135527875058981895, 197.5041725223112792, 100.5988620819214390 ) ) ;
#4781 = AXIS2_PLACEMENT_3D ( 'NONE', #9687, #19741, #6970 ) ;
#4782 = APPLICATION_PROTOCOL_DEFINITION ( 'draft international standard', 'automotive_design', 1998, #29421 ) ;
#4783 = CARTESIAN_POINT ( 'NONE',  ( 33.52499999726880731, 169.8198683612136222, -4.815267126137197984 ) ) ;
#4784 = CARTESIAN_POINT ( 'NONE',  ( -67.50000000000000000, 122.1366465496900418, -17.00000000000001421 ) ) ;
#4785 = CARTESIAN_POINT ( 'NONE',  ( 32.50000000000000000, 155.0000000000000000, -6.938893903907228378E-15 ) ) ;
#4786 = CARTESIAN_POINT ( 'NONE',  ( 7.456977232089302632, 217.1783343296989131, 1.551137918078565603 ) ) ;
#4787 = CARTESIAN_POINT ( 'NONE',  ( 18.40606158072673182, -21.12752019707603424, -0.2340887491524535069 ) ) ;
#4788 = CARTESIAN_POINT ( 'NONE',  ( 54.07499999726880446, 168.2552932293087906, 9.630534252274372875 ) ) ;
#4789 = ADVANCED_FACE ( 'NONE', ( #6669 ), #14336, .F. ) ;
#4790 = CARTESIAN_POINT ( 'NONE',  ( 0.05014649552810505201, 217.5146222423826714, 43.25113791807856956 ) ) ;
#4791 = CARTESIAN_POINT ( 'NONE',  ( 88.02499999726880731, 160.0630714827496206, 15.58253174999999402 ) ) ;
#4792 = CARTESIAN_POINT ( 'NONE',  ( 42.01132485994281751, 167.7597621252805880, -9.270509831248443078 ) ) ;
#4793 = CARTESIAN_POINT ( 'NONE',  ( 32.50000000000000000, 155.0000000000000000, -6.938893903907228378E-15 ) ) ;
#4794 = CARTESIAN_POINT ( 'NONE',  ( 56.59999999453763309, 168.7903194862797420, 4.480746418436729606 ) ) ;
#4795 = VERTEX_POINT ( 'NONE', #32552 ) ;
#4796 = CARTESIAN_POINT ( 'NONE',  ( -7.456977232089304408, 196.8216656703010301, 27.05113791807857027 ) ) ;
#4797 = CIRCLE ( 'NONE', #3162, 112.0000000000000426 ) ;
#4798 = EDGE_CURVE ( 'NONE', #22066, #29326, #9807, .T. ) ;
#4799 = DIRECTION ( 'NONE',  ( -0.000000000000000000, -0.000000000000000000, 1.000000000000000000 ) ) ;
#4800 = CARTESIAN_POINT ( 'NONE',  ( 10.00000000000000711, 207.0476921513415220, 15.99886208192143400 ) ) ;
#4801 = CARTESIAN_POINT ( 'NONE',  ( 32.50000000000000000, 155.0000000000000000, 15.00000000000001243 ) ) ;
#4802 = ORIENTED_EDGE ( 'NONE', *, *, #598, .F. ) ;
#4803 = CARTESIAN_POINT ( 'NONE',  ( 9.984503880673470277, 203.7031108863295401, 8.151137918078564581 ) ) ;
#4804 = CARTESIAN_POINT ( 'NONE',  ( -10.01549611932653860, 203.7984951890123284, 72.35113791807859229 ) ) ;
#4805 = VERTEX_POINT ( 'NONE', #30513 ) ;
#4806 = CARTESIAN_POINT ( 'NONE',  ( -6.444103211790928043, 202.2591342207265939, 23.19886208192143684 ) ) ;
#4807 = VECTOR ( 'NONE', #12580, 1000.000000000000000 ) ;
#4808 = DIRECTION ( 'NONE',  ( -1.000000000000000000, -0.000000000000000000, -0.000000000000000000 ) ) ;
#4809 = ORIENTED_EDGE ( 'NONE', *, *, #27849, .T. ) ;
#4810 = CARTESIAN_POINT ( 'NONE',  ( 0.05014649552807626948, 215.4116977939061144, 7.251137918078565114 ) ) ;
#4811 = CARTESIAN_POINT ( 'NONE',  ( 7.375838497908012492, 217.2372850707501186, 93.54886208192142760 ) ) ;
#4812 = CARTESIAN_POINT ( 'NONE',  ( 35.07499999726881157, 141.7447067706911810, -9.630534252274387086 ) ) ;
#4813 = EDGE_LOOP ( 'NONE', ( #8074, #7187, #7163, #16722 ) ) ;
#4814 = CARTESIAN_POINT ( 'NONE',  ( 43.02499999726880020, 149.9369285172503510, -15.58253175000000823 ) ) ;
#4815 = CARTESIAN_POINT ( 'NONE',  ( -65.20000000000000284, 0.9203920079924619024, 19.30000000000001847 ) ) ;
#4816 = CARTESIAN_POINT ( 'NONE',  ( -10.00000000000000711, 207.0476921513413515, 3.501137918078566003 ) ) ;
#4817 = CIRCLE ( 'NONE', #12432, 2.149999999999994138 ) ;
#4818 = CARTESIAN_POINT ( 'NONE',  ( 3.135527875058981895, 197.5041725223112792, 70.59886208192143897 ) ) ;
#4819 = CARTESIAN_POINT ( 'NONE',  ( 50.17499999726881299, 164.1591823560292198, 12.60653300113718167 ) ) ;
#4820 = CARTESIAN_POINT ( 'NONE',  ( -67.50001199999998391, 139.7198396726428768, 7.533570508255921006 ) ) ;
#4821 = CARTESIAN_POINT ( 'NONE',  ( 10.01549611932653860, 210.2015048109876716, 16.85113791807856032 ) ) ;
#4822 = DIRECTION ( 'NONE',  ( -1.000000000000000000, 0.000000000000000000, 0.000000000000000000 ) ) ;
#4823 = EDGE_CURVE ( 'NONE', #31786, #29479, #20632, .T. ) ;
#4824 = AXIS2_PLACEMENT_3D ( 'NONE', #2884, #31989, #11215 ) ;
#4825 = CONICAL_SURFACE ( 'NONE', #23862, 7.500000000000001776, 0.8594454914424796144 ) ;
#4826 = CARTESIAN_POINT ( 'NONE',  ( 69.79999999999996874, 142.6655632788954620, 8.961492836873471646 ) ) ;
#4827 = CARTESIAN_POINT ( 'NONE',  ( -10.00000000000000711, 207.0476921513413515, 93.50113791807858377 ) ) ;
#4828 = FACE_OUTER_BOUND ( 'NONE', #742, .T. ) ;
#4829 = CARTESIAN_POINT ( 'NONE',  ( 0.05014649552810505201, 217.5146222423826714, 73.25113791807855534 ) ) ;
#4830 = DIRECTION ( 'NONE',  ( -1.000000000000000000, 0.000000000000000000, 0.000000000000000000 ) ) ;
#4831 = CARTESIAN_POINT ( 'NONE',  ( 34.07499999726879736, 168.2552932293087906, 9.630534252274372875 ) ) ;
#4832 = EDGE_CURVE ( 'NONE', #32368, #8582, #22968, .T. ) ;
#4833 = CARTESIAN_POINT ( 'NONE',  ( -9.680171189290716072, 199.9079932115567146, 83.19886208192144750 ) ) ;
#4834 = CIRCLE ( 'NONE', #28789, 100.0000000000000284 ) ;
#4835 = CARTESIAN_POINT ( 'NONE',  ( 71.82499999726883289, 168.2552932293087906, 9.630534252274372875 ) ) ;
#4837 = ORIENTED_EDGE ( 'NONE', *, *, #10381, .T. ) ;
#4836 = CARTESIAN_POINT ( 'NONE',  ( -6.220909254589537696, 198.5229672870051445, 30.05113791807856671 ) ) ;
#4838 = CARTESIAN_POINT ( 'NONE',  ( -58.50000000000002132, 194.9217985566782829, 2.500000000000000000 ) ) ;
#4839 = CARTESIAN_POINT ( 'NONE',  ( 37.09999999453763309, 150.2886644046228639, 14.49999999999999645 ) ) ;
#4840 = CARTESIAN_POINT ( 'NONE',  ( 3.753561863808689836, 218.3979405102790565, 94.40113791807857524 ) ) ;
#4841 = CARTESIAN_POINT ( 'NONE',  ( 0.000000000000000000, 0.000000000000000000, 0.000000000000000000 ) ) ;
#4842 = ORIENTED_EDGE ( 'NONE', *, *, #7670, .T. ) ;
#4843 = CARTESIAN_POINT ( 'NONE',  ( -8.062137200540822946, 201.0835637161416400, 83.19886208192143329 ) ) ;
#4844 = CARTESIAN_POINT ( 'NONE',  ( 12.00000000000000711, 207.0476921513415220, 18.99886208192143400 ) ) ;
#4845 = CARTESIAN_POINT ( 'NONE',  ( 10.83124253962820305, -25.50084400951698527, -0.1142222407377387061 ) ) ;
#4846 = CARTESIAN_POINT ( 'NONE',  ( -9.984503880673473830, 210.2968891136704315, 30.65113791807856813 ) ) ;
#4847 = ORIENTED_EDGE ( 'NONE', *, *, #25539, .F. ) ;
#4848 = CARTESIAN_POINT ( 'NONE',  ( 8.118202686958138514, 201.1607312380088501, 94.29886208192144181 ) ) ;
#4849 = CIRCLE ( 'NONE', #9202, 112.0000000000000711 ) ;
#4850 = CARTESIAN_POINT ( 'NONE',  ( 4.574783636564339950, 5.228990388887490681, -6.171384342982508819 ) ) ;
#4851 = EDGE_LOOP ( 'NONE', ( #7398, #16730 ) ) ;
#4852 = CARTESIAN_POINT ( 'NONE',  ( -0.5725525826505220017, -3.710888496608931497, -0.1217565302851259662 ) ) ;
#4853 = CARTESIAN_POINT ( 'NONE',  ( 7.984503880673422316, 209.6470497212048372, 84.84886208192142476 ) ) ;
#4854 = ORIENTED_EDGE ( 'NONE', *, *, #30340, .T. ) ;
#4855 = APPLICATION_CONTEXT ( 'automotive_design' ) ;
#4856 = AXIS2_PLACEMENT_3D ( 'NONE', #1255, #1590, #9257 ) ;
#4857 = CARTESIAN_POINT ( 'NONE',  ( 4.764707147349631625E-14, -103.0000000000000284, 20.00000000000000000 ) ) ;
#4858 = ORIENTED_EDGE ( 'NONE', *, *, #4975, .F. ) ;
#4859 = DIRECTION ( 'NONE',  ( 0.000000000000000000, 1.000000000000000000, -1.100686371591861952E-15 ) ) ;
#4860 = CARTESIAN_POINT ( 'NONE',  ( 8.015496119326531499, 209.5516654185219636, 58.85113791807857098 ) ) ;
#4861 = CARTESIAN_POINT ( 'NONE',  ( 81.12499999726881583, 155.0000000000000000, -15.58253175000000823 ) ) ;
#4862 = LINE ( 'NONE', #28374, #29556 ) ;
#4863 = CARTESIAN_POINT ( 'NONE',  ( 7.984503880673485376, 204.3529502787953902, 77.15113791807857524 ) ) ;
#4864 = CARTESIAN_POINT ( 'NONE',  ( -1.994931997373328159E-14, -8.660254037844390851, -1.000000000000000888 ) ) ;
#4865 = CARTESIAN_POINT ( 'NONE',  ( 45.50000000000000000, 155.0000000000000000, 14.49999999999999467 ) ) ;
#4866 = CARTESIAN_POINT ( 'NONE',  ( 8.000000000000008882, 207.0476921513415220, 60.99886208192144466 ) ) ;
#4867 = VECTOR ( 'NONE', #24740, 1000.000000000000000 ) ;
#4868 = CARTESIAN_POINT ( 'NONE',  ( 67.28867513459482552, 170.7719333635740497, -7.904646289410545231E-15 ) ) ;
#4869 = CARTESIAN_POINT ( 'NONE',  ( 6.220909254589536808, 215.4770327129947987, 1.551137918078565825 ) ) ;
#4870 = CARTESIAN_POINT ( 'NONE',  ( -3.750000000000001776, 6.495190528383289141, -6.991905250253753756 ) ) ;
#4871 = CARTESIAN_POINT ( 'NONE',  ( -120.8017490774095393, 3.226370279868306046, 35.00001199999999812 ) ) ;
#4872 = CARTESIAN_POINT ( 'NONE',  ( 57.12499999726880873, 155.0000000000000000, -15.58253175000000823 ) ) ;
#4873 = CARTESIAN_POINT ( 'NONE',  ( 70.47499999726881015, 149.9369285172503510, 15.58253174999999580 ) ) ;
#4874 = CARTESIAN_POINT ( 'NONE',  ( 11.98450388067348271, 203.0532714938637753, 65.15113791807856103 ) ) ;
#4875 = LINE ( 'NONE', #33666, #14061 ) ;
#4876 = CARTESIAN_POINT ( 'NONE',  ( -0.05014649552807705357, 194.3824533091408000, 11.75113791807856600 ) ) ;
#4877 = EDGE_CURVE ( 'NONE', #33593, #5010, #23506, .T. ) ;
#4878 = CARTESIAN_POINT ( 'NONE',  ( 3.135527875058820690, 216.4958274776887492, 88.40113791807857524 ) ) ;
#4879 = CARTESIAN_POINT ( 'NONE',  ( -12.00000000000000711, 206.9523078486584780, 47.49886208192144466 ) ) ;
#4880 = CARTESIAN_POINT ( 'NONE',  ( -3.135527875058982783, 216.4958274776886924, 54.09886208192143897 ) ) ;
#4881 = CARTESIAN_POINT ( 'NONE',  ( 4.000000000000000000, 0.000000000000000000, 0.000000000000000000 ) ) ;
#4882 =( BOUNDED_CURVE ( )  B_SPLINE_CURVE ( 2, ( #13053, #27748, #28086, #33204, #20085, #2994, #9867, #14797, #13373, #20250, #23770 ),
 .UNSPECIFIED., .F., .T. ) 
 B_SPLINE_CURVE_WITH_KNOTS ( ( 3, 2, 2, 2, 2, 3 ),
 ( 0.5892857142857139685, 0.5928571428571425272, 0.5964285714285710860, 0.5999999999999997558, 0.6035714285714283145, 0.6071428571428568732 ),
 .UNSPECIFIED. ) 
 CURVE ( )  GEOMETRIC_REPRESENTATION_ITEM ( )  RATIONAL_B_SPLINE_CURVE ( ( 1.000000000000003109, 0.9510565162951504226, 1.000000000000000000, 0.9510565162951534202, 1.000000000000000000, 0.9510565162951534202, 1.000000000000000000, 0.9510565162951534202, 1.000000000000000000, 0.9510565162951564178, 0.9999999999999970024 ) ) 
 REPRESENTATION_ITEM ( '' )  );
#4883 = CARTESIAN_POINT ( 'NONE',  ( 12.01549611932652972, 210.8513442034534933, 97.85113791807857808 ) ) ;
#4884 = DIRECTION ( 'NONE',  ( 1.000000000000000000, 0.000000000000000000, 0.000000000000000000 ) ) ;
#4885 = CARTESIAN_POINT ( 'NONE',  ( 0.05014649552810505201, 217.5146222423826714, 1.251137918078566003 ) ) ;
#4886 = CARTESIAN_POINT ( 'NONE',  ( -10.01549611932659722, 210.2015048109875011, 68.64886208192143613 ) ) ;
#4887 = DIRECTION ( 'NONE',  ( 0.000000000000000000, 0.000000000000000000, -1.000000000000000000 ) ) ;
#4888 = EDGE_LOOP ( 'NONE', ( #8453, #28571, #8129 ) ) ;
#4889 = CARTESIAN_POINT ( 'NONE',  ( 9.736236675708031640, 199.9851607334238963, 70.29886208192142760 ) ) ;
#4890 = CARTESIAN_POINT ( 'NONE',  ( 6.220909254589536808, 215.4770327129947702, 94.55113791807858092 ) ) ;
#4891 = VERTEX_POINT ( 'NONE', #12964 ) ;
#4892 = CARTESIAN_POINT ( 'NONE',  ( 81.07499999726880446, 141.7447067706911810, -9.630534252274385310 ) ) ;
#4893 = CARTESIAN_POINT ( 'NONE',  ( -4.984841277089891776, 213.7757310962905990, 53.94886208192144039 ) ) ;
#4894 = CIRCLE ( 'NONE', #3796, 1.000000000000000888 ) ;
#4895 = EDGE_LOOP ( 'NONE', ( #10562, #15791, #29430, #25406 ) ) ;
#4896 = CARTESIAN_POINT ( 'NONE',  ( 68.62499999726880162, 138.6155565068815747, -3.929120461958505118E-15 ) ) ;
#4897 = DIRECTION ( 'NONE',  ( -1.000000000000000000, 0.000000000000000000, 0.000000000000000000 ) ) ;
#4898 = CARTESIAN_POINT ( 'NONE',  ( -56.61815514298172758, 194.9659613751070140, -1.653849335561433209 ) ) ;
#4899 = CARTESIAN_POINT ( 'NONE',  ( 62.32499999726881867, 145.8408176439707802, 12.60653300113718345 ) ) ;
#4900 = CARTESIAN_POINT ( 'NONE',  ( -7.500000000000000000, 3.202583086485915942, -7.213046687579523386 ) ) ;
#4901 = CARTESIAN_POINT ( 'NONE',  ( -10.01549611932659722, 210.2015048109875011, 56.64886208192142902 ) ) ;
#4902 = ORIENTED_EDGE ( 'NONE', *, *, #19173, .F. ) ;
#4903 = CYLINDRICAL_SURFACE ( 'NONE', #5306, 16.00000000000000000 ) ;
#4904 = LINE ( 'NONE', #22961, #7980 ) ;
#4905 = FACE_OUTER_BOUND ( 'NONE', #8529, .T. ) ;
#4906 = CARTESIAN_POINT ( 'NONE',  ( -8.015496119326597224, 209.5516654185217362, 38.64886208192143613 ) ) ;
#4907 = CARTESIAN_POINT ( 'NONE',  ( 3.135527875058820690, 216.4958274776887492, 73.40113791807857524 ) ) ;
#4908 = DIRECTION ( 'NONE',  ( 0.000000000000000000, 0.000000000000000000, -1.000000000000000000 ) ) ;
#4909 = CARTESIAN_POINT ( 'NONE',  ( -9.984503880673473830, 210.2968891136704315, 60.65113791807856103 ) ) ;
#4910 = ITEM_DEFINED_TRANSFORMATION ( 'NONE', 'NONE', #6676,  #2404 ) ;
#4911 = CARTESIAN_POINT ( 'NONE',  ( -6.139770520408369237, 215.5359834540460042, 30.95113791807857240 ) ) ;
#4912 = CARTESIAN_POINT ( 'NONE',  ( 8.015496119326531499, 209.5516654185219636, 7.851137918078565647 ) ) ;
#4913 = CARTESIAN_POINT ( 'NONE',  ( 46.18867513459481700, 140.7341522555726669, 4.635254915624211769 ) ) ;
#4914 = LINE ( 'NONE', #23313, #24730 ) ;
#4915 = CARTESIAN_POINT ( 'NONE',  ( 40.52499999726881441, 140.1801316387863778, 4.815267126137185549 ) ) ;
#4916 = CARTESIAN_POINT ( 'NONE',  ( -7.456977232089304408, 196.8216656703010301, 42.05113791807857382 ) ) ;
#4917 = CYLINDRICAL_SURFACE ( 'NONE', #21679, 15.00000000000001776 ) ;
#4918 = CARTESIAN_POINT ( 'NONE',  ( -8.118202686958039038, 201.1607312380087080, 81.20113791807857240 ) ) ;
#4919 = ADVANCED_FACE ( 'NONE', ( #10585 ), #17911, .T. ) ;
#4920 = CARTESIAN_POINT ( 'NONE',  ( -3.135527875058821579, 197.5041725223112223, 56.90113791807857524 ) ) ;
#4921 = CARTESIAN_POINT ( 'NONE',  ( 2.000000000000000000, 1.773042676681340968, -2.276824562219559311E-15 ) ) ;
#4922 = CARTESIAN_POINT ( 'NONE',  ( 9.680171189290716072, 214.0920067884432854, 9.698862081921433287 ) ) ;
#4923 = CARTESIAN_POINT ( 'NONE',  ( 8.118202686958138514, 201.1607312380088501, 31.29886208192143826 ) ) ;
#4924 = CARTESIAN_POINT ( 'NONE',  ( 74.29999999453762882, 167.3344367211045096, -8.961492836873482304 ) ) ;
#4925 = ORIENTED_EDGE ( 'NONE', *, *, #8272, .F. ) ;
#4926 = CARTESIAN_POINT ( 'NONE',  ( 3.753561863808689836, 218.3979405102790565, 67.40113791807856103 ) ) ;
#4927 = CARTESIAN_POINT ( 'NONE',  ( 4.984841277089725686, 213.7757310962907411, 76.55113791807858092 ) ) ;
#4928 = CARTESIAN_POINT ( 'NONE',  ( 6.139770520408223575, 215.5359834540460611, 36.54886208192142050 ) ) ;
#4929 = CARTESIAN_POINT ( 'NONE',  ( 91.60208470531341618, 155.0000000000000000, 0.000000000000000000 ) ) ;
#4930 = ORIENTED_EDGE ( 'NONE', *, *, #12672, .F. ) ;
#4931 = ADVANCED_FACE ( 'NONE', ( #7691 ), #2408, .F. ) ;
#4932 = CARTESIAN_POINT ( 'NONE',  ( -7.375838497908014268, 196.7627149292498530, 41.04886208192144181 ) ) ;
#4933 = AXIS2_PLACEMENT_3D ( 'NONE', #12401, #27556, #32669 ) ;
#4934 = ORIENTED_EDGE ( 'NONE', *, *, #1063, .T. ) ;
#4935 = ORIENTED_EDGE ( 'NONE', *, *, #26240, .F. ) ;
#4936 = DIRECTION ( 'NONE',  ( 0.000000000000000000, 0.000000000000000000, 1.000000000000000000 ) ) ;
#4937 = DIRECTION ( 'NONE',  ( 1.000000000000000000, 0.000000000000000000, 0.000000000000000000 ) ) ;
#4938 = EDGE_CURVE ( 'NONE', #5394, #24155, #20962, .T. ) ;
#4939 = EDGE_LOOP ( 'NONE', ( #20400, #17543, #13634, #16072 ) ) ;
#4940 = CARTESIAN_POINT ( 'NONE',  ( 4.984841277089725686, 213.7757310962907411, 43.55113791807857382 ) ) ;
#4941 = CARTESIAN_POINT ( 'NONE',  ( -10.01549611932659722, 210.2015048109875011, 26.64886208192142902 ) ) ;
#4942 = CARTESIAN_POINT ( 'NONE',  ( 53.67499999726880588, 168.2552932293087906, -9.630534252274387086 ) ) ;
#4943 = ORIENTED_EDGE ( 'NONE', *, *, #20444, .F. ) ;
#4944 = CARTESIAN_POINT ( 'NONE',  ( -4.903702542908602524, 213.8346818373418898, 54.95113791807857240 ) ) ;
#4945 = CARTESIAN_POINT ( 'NONE',  ( -10.00000000000000178, 206.7692714347156198, 108.3323677711372000 ) ) ;
#4946 = CARTESIAN_POINT ( 'NONE',  ( 0.000000000000000000, 0.000000000000000000, -8.000000000000000000 ) ) ;
#4947 = CARTESIAN_POINT ( 'NONE',  ( 0.05014649552828275708, 196.4853777576173002, 100.7488620819214304 ) ) ;
#4948 = EDGE_CURVE ( 'NONE', #22445, #13672, #13175, .T. ) ;
#4949 = CARTESIAN_POINT ( 'NONE',  ( 67.97499999726881015, 169.8198683612136222, 4.815267126137181997 ) ) ;
#4950 = CARTESIAN_POINT ( 'NONE',  ( -3.135527875058821579, 197.5041725223112223, 38.90113791807857524 ) ) ;
#4951 = CARTESIAN_POINT ( 'NONE',  ( 86.71132485994282035, 155.0000000000000000, 15.00000000000001243 ) ) ;
#4952 = CARTESIAN_POINT ( 'NONE',  ( 8.062137200540920645, 201.0835637161417822, 23.30113791807856671 ) ) ;
#4953 = CARTESIAN_POINT ( 'NONE',  ( 8.118202686958138514, 201.1607312380088501, 100.2988620819214418 ) ) ;
#4954 = SHAPE_DEFINITION_REPRESENTATION ( #24647, #22175 ) ;
#4955 = VECTOR ( 'NONE', #22448, 1000.000000000000000 ) ;
#4956 = CARTESIAN_POINT ( 'NONE',  ( 4.903702542908435547, 213.8346818373419751, 78.54886208192142760 ) ) ;
#4957 = CARTESIAN_POINT ( 'NONE',  ( 86.70000000000000284, 163.5228861582408797, -11.73074641843674470 ) ) ;
#4958 = CARTESIAN_POINT ( 'NONE',  ( -57.39039945611308013, 194.9369330859559284, 2.246172506675526481 ) ) ;
#4959 = DIRECTION ( 'NONE',  ( 0.000000000000000000, 0.7071067811865442421, -0.7071067811865506814 ) ) ;
#4960 = CARTESIAN_POINT ( 'NONE',  ( 12.01549611932652972, 210.8513442034534933, 4.851137918078565647 ) ) ;
#4961 = CYLINDRICAL_SURFACE ( 'NONE', #17838, 4.250000000000000000 ) ;
#4962 = CARTESIAN_POINT ( 'NONE',  ( 48.87499999726880873, 138.6155565068815463, -3.929120461958505118E-15 ) ) ;
#4963 = CARTESIAN_POINT ( 'NONE',  ( -10.00000000000000711, 207.0476921513413515, 60.50113791807857666 ) ) ;
#4964 = EDGE_CURVE ( 'NONE', #19918, #8949, #23184, .T. ) ;
#4965 = CARTESIAN_POINT ( 'NONE',  ( 87.42499999726881299, 168.2552932293087906, -9.630534252274385310 ) ) ;
#4966 = CARTESIAN_POINT ( 'NONE',  ( 42.11132485994280472, 169.2658477444273331, -4.635254915624224203 ) ) ;
#4967 = CARTESIAN_POINT ( 'NONE',  ( 125.5000000000000000, 231.4735983853249763, -73.43303922622312996 ) ) ;
#4968 = CARTESIAN_POINT ( 'NONE',  ( 54.89999999453763024, 159.7113355953771077, 14.49999999999999289 ) ) ;
#4969 = ORIENTED_EDGE ( 'NONE', *, *, #23752, .T. ) ;
#4970 = CARTESIAN_POINT ( 'NONE',  ( 0.05014649552807549926, 219.6175466908591716, 28.25113791807856245 ) ) ;
#4971 = DIRECTION ( 'NONE',  ( -0.000000000000000000, -0.000000000000000000, 1.000000000000000000 ) ) ;
#4972 = CARTESIAN_POINT ( 'NONE',  ( -9.984503880673420539, 203.7031108863293980, 14.34886208192143542 ) ) ;
#4973 = CARTESIAN_POINT ( 'NONE',  ( -67.50000000000000000, 155.0000000000000000, 6.938893903907228378E-15 ) ) ;
#4974 = ORIENTED_EDGE ( 'NONE', *, *, #1, .F. ) ;
#4975 = EDGE_CURVE ( 'NONE', #8265, #26498, #11011, .T. ) ;
#4976 = B_SPLINE_CURVE_WITH_KNOTS ( 'NONE', 3,
 ( #3844, #13037, #30938, #20873, #25820, #4864 ),
 .UNSPECIFIED., .F., .F.,
 ( 4, 2, 4 ),
 ( 0.004444412883774326306, 0.006655097293744431999, 0.008865781703714537693 ),
 .UNSPECIFIED. ) ;
#4977 = CARTESIAN_POINT ( 'NONE',  ( -10.01549611932653860, 203.7984951890123284, 12.35113791807856387 ) ) ;
#4978 = CARTESIAN_POINT ( 'NONE',  ( -8.062137200540920645, 212.9164362838581894, 66.80113791807858092 ) ) ;
#4979 = VERTEX_POINT ( 'NONE', #5126 ) ;
#4980 = CARTESIAN_POINT ( 'NONE',  ( -2.517493886309087880, 214.5937144450984135, 30.09886208192144252 ) ) ;
#4981 = CARTESIAN_POINT ( 'NONE',  ( 80.38867513459483405, 140.7341522555726669, -4.635254915624220651 ) ) ;
#4982 = CIRCLE ( 'NONE', #24008, 0.9999999999999915623 ) ;
#4983 = VERTEX_POINT ( 'NONE', #17735 ) ;
#4984 = CARTESIAN_POINT ( 'NONE',  ( -2.426778023690262742, 214.6231898156240163, 1.101137918078566091 ) ) ;
#4985 = EDGE_CURVE ( 'NONE', #2381, #2474, #26153, .T. ) ;
#4986 = CARTESIAN_POINT ( 'NONE',  ( 9.680171189290716072, 214.0920067884432854, 84.69886208192144750 ) ) ;
#4987 = CARTESIAN_POINT ( 'NONE',  ( 40.27499999726881441, 160.0630714827496206, 15.58253174999999224 ) ) ;
#4988 = ORIENTED_EDGE ( 'NONE', *, *, #26148, .T. ) ;
#4989 = CARTESIAN_POINT ( 'NONE',  ( 44.62499999726880873, 138.6155565068815463, -3.929120461958505118E-15 ) ) ;
#4990 = FACE_OUTER_BOUND ( 'NONE', #28545, .T. ) ;
#4991 = CARTESIAN_POINT ( 'NONE',  ( 10.00000000000000711, 206.9523078486586201, 5.001137918078565114 ) ) ;
#4992 = CARTESIAN_POINT ( 'NONE',  ( -8.118202686958138514, 212.8392687619910930, 71.79886208192142760 ) ) ;
#4993 = CARTESIAN_POINT ( 'NONE',  ( 47.77499999726881441, 169.8198683612136222, -4.815267126137197984 ) ) ;
#4994 = CARTESIAN_POINT ( 'NONE',  ( -67.50001199999998391, 149.5223338078428696, 16.13174377802662818 ) ) ;
#4995 = CARTESIAN_POINT ( 'NONE',  ( -8.062137200540920645, 212.9164362838581894, 15.80113791807856849 ) ) ;
#4996 = CARTESIAN_POINT ( 'NONE',  ( 125.5000000000000000, 80.04668119422662187, 74.95331880577468553 ) ) ;
#4997 = CARTESIAN_POINT ( 'NONE',  ( 65.79999999999998295, 142.6655632788954620, 8.961492836873471646 ) ) ;
#4998 = CARTESIAN_POINT ( 'NONE',  ( 10.01549611932653860, 210.2015048109876716, 100.8511379180785497 ) ) ;
#4999 = DIRECTION ( 'NONE',  ( 0.000000000000000000, 0.000000000000000000, -1.000000000000000000 ) ) ;
#5000 = CARTESIAN_POINT ( 'NONE',  ( 8.118202686958039038, 212.8392687619912635, 79.70113791807857240 ) ) ;
#5001 = CARTESIAN_POINT ( 'NONE',  ( 86.68867513459481700, 150.1262045565063374, -14.99999999999995737 ) ) ;
#5002 = CARTESIAN_POINT ( 'NONE',  ( 33.57499999726881157, 164.1591823560292198, -12.60653300113719766 ) ) ;
#5003 = CARTESIAN_POINT ( 'NONE',  ( -9.736236675708031640, 214.0148392665760753, 86.79886208192142760 ) ) ;
#5004 = CARTESIAN_POINT ( 'NONE',  ( 73.52499999726882152, 169.8198683612136222, -4.815267126137197984 ) ) ;
#5005 = VERTEX_POINT ( 'NONE', #7859 ) ;
#5006 = CARTESIAN_POINT ( 'NONE',  ( -60.38481630464774241, 194.9660974499433053, -1.650668498912690740 ) ) ;
#5007 = CARTESIAN_POINT ( 'NONE',  ( 87.57499999726880446, 164.1591823560292198, -12.60653300113719766 ) ) ;
#5008 = CARTESIAN_POINT ( 'NONE',  ( -11.98450388067348804, 210.9467285061362247, 99.65113791807858945 ) ) ;
#5009 = CYLINDRICAL_SURFACE ( 'NONE', #24085, 24.99999999999999289 ) ;
#5010 = VERTEX_POINT ( 'NONE', #18244 ) ;
#5011 = CARTESIAN_POINT ( 'NONE',  ( 0.05014649552828275014, 196.4853777576173002, 82.74886208192143044 ) ) ;
#5012 = VECTOR ( 'NONE', #22251, 1000.000000000000000 ) ;
#5013 = CARTESIAN_POINT ( 'NONE',  ( 12.01549611932659367, 203.1486557965466773, 22.14886208192143613 ) ) ;
#5014 = DIRECTION ( 'NONE',  ( 0.000000000000000000, -1.000000000000000000, 1.222984857324291014E-15 ) ) ;
#5015 = CARTESIAN_POINT ( 'NONE',  ( 8.062137200540920645, 201.0835637161417822, 44.30113791807857382 ) ) ;
#5016 = ORIENTED_EDGE ( 'NONE', *, *, #29173, .F. ) ;
#5017 = CARTESIAN_POINT ( 'NONE',  ( 0.05014649552828275708, 196.4853777576173002, 100.7488620819214304 ) ) ;
#5018 = EDGE_CURVE ( 'NONE', #17155, #25250, #23, .T. ) ;
#5019 = EDGE_CURVE ( 'NONE', #25798, #12782, #19635, .T. ) ;
#5020 = CARTESIAN_POINT ( 'NONE',  ( -0.04050535873993896946, 7.919512791578231514, -6.573129608219091757 ) ) ;
#5021 = VERTEX_POINT ( 'NONE', #33411 ) ;
#5022 = CARTESIAN_POINT ( 'NONE',  ( -7.984503880673422316, 204.3529502787951628, 80.34886208192143897 ) ) ;
#5023 = EDGE_CURVE ( 'NONE', #18870, #7638, #28873, .T. ) ;
#5024 = ORIENTED_EDGE ( 'NONE', *, *, #8078, .F. ) ;
#5025 = EDGE_CURVE ( 'NONE', #17895, #7373, #342, .T. ) ;
#5026 = DIRECTION ( 'NONE',  ( 0.000000000000000000, 0.000000000000000000, 1.000000000000000000 ) ) ;
#5027 = ORIENTED_EDGE ( 'NONE', *, *, #10798, .T. ) ;
#5028 = LINE ( 'NONE', #2477, #930 ) ;
#5029 = CARTESIAN_POINT ( 'NONE',  ( -0.05014649552807731031, 198.5883022060938572, 59.75113791807857666 ) ) ;
#5030 = CARTESIAN_POINT ( 'NONE',  ( 85.42499999726879878, 168.2552932293087906, -9.630534252274385310 ) ) ;
#5031 = DIRECTION ( 'NONE',  ( -0.000000000000000000, -0.000000000000000000, -1.000000000000000000 ) ) ;
#5032 = CARTESIAN_POINT ( 'NONE',  ( -6.500168698208129925, 202.3363017425936050, 84.20113791807858661 ) ) ;
#5033 = CARTESIAN_POINT ( 'NONE',  ( 100.3007760113082156, 155.0000000000000000, 12.10452846326762177 ) ) ;
#5034 = PRESENTATION_STYLE_ASSIGNMENT (( #17985 ) ) ;
#5035 = CARTESIAN_POINT ( 'NONE',  ( 49.19999999999999574, 167.3344367211045096, 8.961492836873468093 ) ) ;
#5036 = CARTESIAN_POINT ( 'NONE',  ( 6.444103211790928043, 211.7408657792734061, 63.69886208192144039 ) ) ;
#5037 = CARTESIAN_POINT ( 'NONE',  ( 92.60208470531341618, 155.0000000000000000, 0.000000000000000000 ) ) ;
#5038 = AXIS2_PLACEMENT_3D ( 'NONE', #18468, #28854, #5510 ) ;
#5039 = CARTESIAN_POINT ( 'NONE',  ( 53.42499999726879878, 168.2552932293087906, -9.630534252274385310 ) ) ;
#5040 = CARTESIAN_POINT ( 'NONE',  ( 125.5000000000000000, 81.56696077377769427, 76.47359838532574372 ) ) ;
#5041 = LINE ( 'NONE', #7432, #22790 ) ;
#5042 = CARTESIAN_POINT ( 'NONE',  ( 58.12499999726881583, 155.0000000000000000, 15.58253174999999402 ) ) ;
#5043 = CARTESIAN_POINT ( 'NONE',  ( 70.27499999726880731, 160.0630714827496206, 15.58253174999999402 ) ) ;
#5044 = CARTESIAN_POINT ( 'NONE',  ( -11.98450388067348804, 210.9467285061362247, 63.65113791807855392 ) ) ;
#5045 = CARTESIAN_POINT ( 'NONE',  ( 46.31132485994280756, 169.2658477444273331, 4.635254915624208216 ) ) ;
#5046 = CARTESIAN_POINT ( 'NONE',  ( 7.375838497908181246, 196.7627149292499666, 14.45113791807856707 ) ) ;
#5047 = CARTESIAN_POINT ( 'NONE',  ( -3.135527875058821579, 197.5041725223112223, 86.90113791807857524 ) ) ;
#5048 = CARTESIAN_POINT ( 'NONE',  ( 7.375838497908012492, 217.2372850707501186, 48.54886208192142050 ) ) ;
#5049 = PRODUCT_DEFINITION_FORMATION_WITH_SPECIFIED_SOURCE ( 'ANY', '', #32253, .NOT_KNOWN. ) ;
#5050 = CARTESIAN_POINT ( 'NONE',  ( -8.062137200540822946, 201.0835637161416400, 56.19886208192144039 ) ) ;
#5051 = CARTESIAN_POINT ( 'NONE',  ( 95.70416941062676131, 155.0000000000000000, 0.000000000000000000 ) ) ;
#5052 = CARTESIAN_POINT ( 'NONE',  ( -12.01549611932652972, 203.1486557965464499, 99.35113791807857808 ) ) ;
#5053 = CARTESIAN_POINT ( 'NONE',  ( -67.50001199999998391, 171.9999999999999716, -1.112647398146377142 ) ) ;
#5054 = CARTESIAN_POINT ( 'NONE',  ( -6.139770520408369237, 215.5359834540460042, 15.95113791807856884 ) ) ;
#5055 = CARTESIAN_POINT ( 'NONE',  ( -10.01549611932659722, 210.2015048109875011, 71.64886208192143613 ) ) ;
#5056 = ORIENTED_EDGE ( 'NONE', *, *, #2430, .T. ) ;
#5057 = CARTESIAN_POINT ( 'NONE',  ( -11.98450388067341876, 203.0532714938636047, 77.34886208192143897 ) ) ;
#5058 = CARTESIAN_POINT ( 'NONE',  ( -0.05014649552810635652, 196.4853777576173002, 89.75113791807854113 ) ) ;
#5059 = AXIS2_PLACEMENT_3D ( 'NONE', #2797, #23575, #31410 ) ;
#5060 = ORIENTED_EDGE ( 'NONE', *, *, #7734, .T. ) ;
#5061 = CARTESIAN_POINT ( 'NONE',  ( 76.67499999726881299, 141.7447067706911810, 9.630534252274376428 ) ) ;
#5062 = CARTESIAN_POINT ( 'NONE',  ( 2.426778023690075337, 214.6231898156240447, 48.39886208192144323 ) ) ;
#5063 = ORIENTED_EDGE ( 'NONE', *, *, #19325, .T. ) ;
#5064 = CARTESIAN_POINT ( 'NONE',  ( 74.22499999726881015, 149.9369285172503510, 15.58253174999999580 ) ) ;
#5065 = CARTESIAN_POINT ( 'NONE',  ( 0.000000000000000000, 0.000000000000000000, -9.974600000000000577 ) ) ;
#5066 = CARTESIAN_POINT ( 'NONE',  ( 60.71132485994280614, 155.0000000000000000, 15.00000000000001243 ) ) ;
#5067 = CARTESIAN_POINT ( 'NONE',  ( 61.12499999726880873, 155.0000000000000000, -15.58253175000000823 ) ) ;
#5068 = CARTESIAN_POINT ( 'NONE',  ( -7.500000000000000000, -3.160302461882432024, -7.231849989190475725 ) ) ;
#5069 = CARTESIAN_POINT ( 'NONE',  ( -10.00000000000000711, 206.9523078486584495, 47.49886208192143755 ) ) ;
#5070 = EDGE_LOOP ( 'NONE', ( #26447, #15986, #25757, #5642 ) ) ;
#5071 = AXIS2_PLACEMENT_3D ( 'NONE', #23018, #33416, #10090 ) ;
#5072 = DIRECTION ( 'NONE',  ( 1.000000000000000000, -0.000000000000000000, -0.000000000000000000 ) ) ;
#5073 = CARTESIAN_POINT ( 'NONE',  ( -4.984841277089891776, 213.7757310962905990, 29.94886208192143684 ) ) ;
#5074 = CARTESIAN_POINT ( 'NONE',  ( -0.05014649552810635652, 196.4853777576173002, 71.75113791807858377 ) ) ;
#5075 = LINE ( 'NONE', #20416, #29977 ) ;
#5076 = CARTESIAN_POINT ( 'NONE',  ( -6.220909254589537696, 198.5229672870051161, 60.05113791807855961 ) ) ;
#5077 = CARTESIAN_POINT ( 'NONE',  ( 8.062137200540920645, 201.0835637161417822, 29.30113791807857027 ) ) ;
#5078 = CARTESIAN_POINT ( 'NONE',  ( -8.015496119326531499, 204.4483345814780364, 15.35113791807856387 ) ) ;
#5079 = CARTESIAN_POINT ( 'NONE',  ( 107.0104235265664556, 155.0000000000000000, 0.000000000000000000 ) ) ;
#5080 = AXIS2_PLACEMENT_3D ( 'NONE', #23053, #4822, #22367 ) ;
#5081 = CARTESIAN_POINT ( 'NONE',  ( -64.96121601855533356, 1.809269760319432319, 19.53878398144468775 ) ) ;
#5082 = CARTESIAN_POINT ( 'NONE',  ( 35.72499999726881015, 169.8198683612136222, 4.815267126137181997 ) ) ;
#5083 = CARTESIAN_POINT ( 'NONE',  ( -9.680171189290831535, 214.0920067884431148, 36.80113791807856671 ) ) ;
#5084 = DIRECTION ( 'NONE',  ( -0.000000000000000000, -0.000000000000000000, 1.000000000000000000 ) ) ;
#5085 = CIRCLE ( 'NONE', #33395, 32.10452846326766974 ) ;
#5086 = CARTESIAN_POINT ( 'NONE',  ( -6.220909254589537696, 198.5229672870051161, 84.05113791807855250 ) ) ;
#5087 = CARTESIAN_POINT ( 'NONE',  ( -10.00000000000000711, 207.0476921513413515, 63.50113791807856956 ) ) ;
#5088 = AXIS2_PLACEMENT_3D ( 'NONE', #1412, #30031, #6696 ) ;
#5089 = CARTESIAN_POINT ( 'NONE',  ( -58.50000000000002132, 209.9999999999999716, -2.500000000000000000 ) ) ;
#5090 = CARTESIAN_POINT ( 'NONE',  ( -3.753561863808878130, 218.3979405102790281, 21.09886208192143897 ) ) ;
#5091 = CARTESIAN_POINT ( 'NONE',  ( -3.044812012439970683, 197.4746971517856196, 31.89886208192143613 ) ) ;
#5092 = CARTESIAN_POINT ( 'NONE',  ( 74.59999999453762598, 168.7903194862797420, 4.480746418436729606 ) ) ;
#5093 = CARTESIAN_POINT ( 'NONE',  ( -12.01549611932652972, 203.1486557965464499, 66.35113791807857808 ) ) ;
#5094 = CARTESIAN_POINT ( 'NONE',  ( -4.984841277089726574, 200.2242689037092305, 81.05113791807856671 ) ) ;
#5095 = CARTESIAN_POINT ( 'NONE',  ( -3.044812012439970683, 197.4746971517856196, 40.89886208192143613 ) ) ;
#5096 = CARTESIAN_POINT ( 'NONE',  ( 75.11132485994279762, 140.7341522555726669, 4.635254915624211769 ) ) ;
#5097 = ORIENTED_EDGE ( 'NONE', *, *, #27929, .T. ) ;
#5098 = CARTESIAN_POINT ( 'NONE',  ( -9.736236675708031640, 214.0148392665760753, 53.79886208192143471 ) ) ;
#5099 = AXIS2_PLACEMENT_3D ( 'NONE', #7320, #7822, #20756 ) ;
#5100 = ORIENTED_EDGE ( 'NONE', *, *, #30794, .F. ) ;
#5101 = MECHANICAL_DESIGN_GEOMETRIC_PRESENTATION_REPRESENTATION (  '', ( #1832 ), #29026 ) ;
#5102 = ORIENTED_EDGE ( 'NONE', *, *, #28904, .T. ) ;
#5103 = PRODUCT_DEFINITION_SHAPE ( 'NONE', 'NONE',  #33691 ) ;
#5104 = CARTESIAN_POINT ( 'NONE',  ( 6.831979103402612274, 3.295157223185832596, -6.443785395948806283 ) ) ;
#5105 = DIRECTION ( 'NONE',  ( 0.000000000000000000, 0.000000000000000000, 1.000000000000000000 ) ) ;
#5106 = ORIENTED_EDGE ( 'NONE', *, *, #14915, .T. ) ;
#5107 = AXIS2_PLACEMENT_3D ( 'NONE', #18569, #26226, #16 ) ;
#5108 = CARTESIAN_POINT ( 'NONE',  ( -0.05014649552807731031, 198.5883022060938572, 44.75113791807857666 ) ) ;
#5109 = VECTOR ( 'NONE', #24322, 1000.000000000000000 ) ;
#5110 = ADVANCED_FACE ( 'NONE', ( #23519 ), #28124, .T. ) ;
#5111 = CARTESIAN_POINT ( 'NONE',  ( -6.139770520408224463, 198.4640165459539389, 23.04886208192143116 ) ) ;
#5112 = CARTESIAN_POINT ( 'NONE',  ( 64.37499999726881583, 155.0000000000000000, 15.58253174999999402 ) ) ;
#5113 = ORIENTED_EDGE ( 'NONE', *, *, #8496, .F. ) ;
#5114 = FACE_OUTER_BOUND ( 'NONE', #22649, .T. ) ;
#5115 = FACE_OUTER_BOUND ( 'NONE', #22282, .T. ) ;
#5116 = CARTESIAN_POINT ( 'NONE',  ( 8.015496119326595448, 204.4483345814782638, 4.148862081921435241 ) ) ;
#5117 = CARTESIAN_POINT ( 'NONE',  ( 6.220909254589536808, 215.4770327129947702, 40.55113791807855250 ) ) ;
#5118 = CARTESIAN_POINT ( 'NONE',  ( 87.01132485994283172, 142.2402378747194405, 9.270509831248432420 ) ) ;
#5119 = CARTESIAN_POINT ( 'NONE',  ( -3.044812012440131443, 216.5253028482142952, 25.10113791807856742 ) ) ;
#5120 = CARTESIAN_POINT ( 'NONE',  ( 8.062137200540822946, 212.9164362838583315, 102.6988620819214475 ) ) ;
#5121 = SHAPE_DEFINITION_REPRESENTATION ( #30668, #25663 ) ;
#5122 = AXIS2_PLACEMENT_3D ( 'NONE', #8421, #23919, #21195 ) ;
#5123 = CARTESIAN_POINT ( 'NONE',  ( 0.05014649552828262524, 198.5883022060938572, 94.74886208192144466 ) ) ;
#5124 = CARTESIAN_POINT ( 'NONE',  ( 87.40000000000000568, 159.7113355953771077, 14.49999999999999289 ) ) ;
#5125 = CARTESIAN_POINT ( 'NONE',  ( -56.51026148866456111, 194.9712507328865740, 1.522362431316129916 ) ) ;
#5126 = CARTESIAN_POINT ( 'NONE',  ( 4.000000000000000000, 2.639212418033077157, 1.523749999999998161 ) ) ;
#5127 = CARTESIAN_POINT ( 'NONE',  ( -12.01549611932652972, 203.1486557965464499, 9.351137918078563871 ) ) ;
#5128 = FACE_OUTER_BOUND ( 'NONE', #6845, .T. ) ;
#5129 = CARTESIAN_POINT ( 'NONE',  ( 53.57499999726881157, 164.1591823560292198, -12.60653300113719766 ) ) ;
#5130 = CARTESIAN_POINT ( 'NONE',  ( -6.220909254589537696, 198.5229672870051161, 57.05113791807857382 ) ) ;
#5131 = CARTESIAN_POINT ( 'NONE',  ( 127.5000000000000000, 157.1500000000010573, 105.9999999999999858 ) ) ;
#5132 = CARTESIAN_POINT ( 'NONE',  ( 0.000000000000000000, 0.000000000000000000, -0.5251556536572846712 ) ) ;
#5133 = CARTESIAN_POINT ( 'NONE',  ( 6.220909254589680693, 198.5229672870052582, 4.448862081921433287 ) ) ;
#5134 = MECHANICAL_DESIGN_GEOMETRIC_PRESENTATION_REPRESENTATION (  '', ( #27423 ), #28537 ) ;
#5135 = CARTESIAN_POINT ( 'NONE',  ( 55.69999999453762030, 142.6655632788954620, -8.961492836873480528 ) ) ;
#5136 = ORIENTED_EDGE ( 'NONE', *, *, #19362, .F. ) ;
#5137 = CARTESIAN_POINT ( 'NONE',  ( 3.753561863808689836, 218.3979405102790565, 40.40113791807857524 ) ) ;
#5138 = CARTESIAN_POINT ( 'NONE',  ( 47.41132485994281609, 142.2402378747194405, -9.270509831248439525 ) ) ;
#5139 = CARTESIAN_POINT ( 'NONE',  ( 3.135527875058981895, 197.5041725223112792, 16.59886208192143542 ) ) ;
#5140 = DIRECTION ( 'NONE',  ( -1.000000000000000000, -0.000000000000000000, -0.000000000000000000 ) ) ;
#5141 = EDGE_LOOP ( 'NONE', ( #18509, #5550, #27056, #19591 ) ) ;
#5142 = CARTESIAN_POINT ( 'NONE',  ( -6.139770520408369237, 215.5359834540460042, 12.95113791807856352 ) ) ;
#5143 = CARTESIAN_POINT ( 'NONE',  ( 6.220909254589536808, 215.4770327129947702, 73.55113791807858092 ) ) ;
#5144 = ORIENTED_EDGE ( 'NONE', *, *, #28298, .T. ) ;
#5145 = CARTESIAN_POINT ( 'NONE',  ( -8.000000000000008882, 206.9523078486584780, 32.49886208192143044 ) ) ;
#5146 =( GEOMETRIC_REPRESENTATION_CONTEXT ( 3 ) GLOBAL_UNCERTAINTY_ASSIGNED_CONTEXT ( ( #505 ) ) GLOBAL_UNIT_ASSIGNED_CONTEXT ( ( #16997, #12058, #9172 ) ) REPRESENTATION_CONTEXT ( 'NONE', 'WORKASPACE' ) );
#5147 = VERTEX_POINT ( 'NONE', #7526 ) ;
#5148 = CARTESIAN_POINT ( 'NONE',  ( -8.000000000000008882, 207.0476921513413515, 12.50113791807856600 ) ) ;
#5149 = ADVANCED_FACE ( 'NONE', ( #2235 ), #12619, .T. ) ;
#5150 = CARTESIAN_POINT ( 'NONE',  ( -9.736236675708031640, 214.0148392665760753, 98.79886208192142760 ) ) ;
#5151 = CARTESIAN_POINT ( 'NONE',  ( 43.57499999726881157, 164.1591823560292198, -12.60653300113719766 ) ) ;
#5152 = VERTEX_POINT ( 'NONE', #19238 ) ;
#5153 = CARTESIAN_POINT ( 'NONE',  ( 51.62499999726880873, 171.3844434931184253, -7.942151717890132712E-15 ) ) ;
#5154 = CARTESIAN_POINT ( 'NONE',  ( 130.2499999999999716, 2.997323040913146538E-14, 35.00000599999999906 ) ) ;
#5155 = CARTESIAN_POINT ( 'NONE',  ( -8.118202686958039038, 201.1607312380087080, 9.201137918078565292 ) ) ;
#5156 = CARTESIAN_POINT ( 'NONE',  ( -6.139770520408224463, 198.4640165459539389, 77.04886208192144181 ) ) ;
#5157 = CARTESIAN_POINT ( 'NONE',  ( 43.97499999726881015, 169.8198683612136222, 4.815267126137181997 ) ) ;
#5158 = CARTESIAN_POINT ( 'NONE',  ( 79.61132485994284025, 150.1262045565065364, -15.00000000000012434 ) ) ;
#5159 = CARTESIAN_POINT ( 'NONE',  ( -10.00000000000000711, 207.0476921513413515, 15.50113791807856600 ) ) ;
#5160 = CARTESIAN_POINT ( 'NONE',  ( 43.78867513459481842, 155.0000000000000000, 15.00000000000001243 ) ) ;
#5161 = EDGE_CURVE ( 'NONE', #30416, #25924, #4359, .T. ) ;
#5162 = CARTESIAN_POINT ( 'NONE',  ( 64.60000000000000853, 159.7113355953771077, -14.50000000000000888 ) ) ;
#5163 = CARTESIAN_POINT ( 'NONE',  ( 6.139770520408368348, 198.4640165459539674, 95.45113791807855819 ) ) ;
#5164 = CARTESIAN_POINT ( 'NONE',  ( 13.75000000000002487, 23.81569860407205397, 0.000000000000000000 ) ) ;
#5165 = CARTESIAN_POINT ( 'NONE',  ( 10.01549611932653860, 210.2015048109876716, 82.85113791807854966 ) ) ;
#5166 = CARTESIAN_POINT ( 'NONE',  ( -27.50000000000000000, 15.87713240271469672, -2.456200930618631428 ) ) ;
#5167 = LINE ( 'NONE', #17775, #11213 ) ;
#5168 = CARTESIAN_POINT ( 'NONE',  ( 12.01549611932659367, 203.1486557965466773, 94.14886208192145034 ) ) ;
#5169 = CARTESIAN_POINT ( 'NONE',  ( 73.02499999726882152, 149.9369285172503510, -15.58253175000000823 ) ) ;
#5170 = VERTEX_POINT ( 'NONE', #18740 ) ;
#5171 = CARTESIAN_POINT ( 'NONE',  ( 43.71132485994280614, 155.0000000000000000, -15.00000000000002487 ) ) ;
#5172 = CARTESIAN_POINT ( 'NONE',  ( 35.69999999453762740, 142.6655632788954620, -8.961492836873480528 ) ) ;
#5173 = CARTESIAN_POINT ( 'NONE',  ( 12.01549611932652972, 210.8513442034534933, 100.8511379180785781 ) ) ;
#5174 = ADVANCED_FACE ( 'NONE', ( #29457 ), #29126, .F. ) ;
#5175 = DIRECTION ( 'NONE',  ( -1.000000000000000000, 0.000000000000000000, -0.000000000000000000 ) ) ;
#5176 = B_SPLINE_CURVE_WITH_KNOTS ( 'NONE', 3,
 ( #28078, #12577, #30814, #18031, #2364, #12917 ),
 .UNSPECIFIED., .F., .F.,
 ( 4, 2, 4 ),
 ( 0.002044882221487502854, 0.003063384235218504989, 0.004081886248949507558 ),
 .UNSPECIFIED. ) ;
#5177 = ORIENTED_EDGE ( 'NONE', *, *, #9983, .F. ) ;
#5178 = CARTESIAN_POINT ( 'NONE',  ( 6.139770520408223575, 215.5359834540460611, 90.54886208192144181 ) ) ;
#5179 = CARTESIAN_POINT ( 'NONE',  ( 9.680171189290716072, 214.0920067884432854, 24.69886208192143684 ) ) ;
#5180 = CARTESIAN_POINT ( 'NONE',  ( 2.243702833038385247, -30.45886237079320580, -1.708299986272457938 ) ) ;
#5181 = CARTESIAN_POINT ( 'NONE',  ( -10.01549611932653860, 203.7984951890123284, 45.35113791807857808 ) ) ;
#5182 = EDGE_CURVE ( 'NONE', #27759, #29773, #16673, .T. ) ;
#5183 = ORIENTED_EDGE ( 'NONE', *, *, #21633, .F. ) ;
#5184 = CARTESIAN_POINT ( 'NONE',  ( 6.500168698208244500, 202.3363017425938324, 7.298862081921435596 ) ) ;
#5185 = DIRECTION ( 'NONE',  ( 0.8660254037844382635, -0.5000000000000006661, 0.000000000000000000 ) ) ;
#5186 = ORIENTED_EDGE ( 'NONE', *, *, #20771, .F. ) ;
#5187 = CARTESIAN_POINT ( 'NONE',  ( 4.903702542908435547, 213.8346818373419751, 87.54886208192142760 ) ) ;
#5188 = VERTEX_POINT ( 'NONE', #16505 ) ;
#5189 = CARTESIAN_POINT ( 'NONE',  ( 8.015496119326531499, 209.5516654185219636, 34.85113791807857098 ) ) ;
#5190 = FACE_OUTER_BOUND ( 'NONE', #27458, .T. ) ;
#5191 = ORIENTED_EDGE ( 'NONE', *, *, #15157, .T. ) ;
#5192 = CARTESIAN_POINT ( 'NONE',  ( 81.31132485994280046, 140.7341522555726669, -4.635254915624220651 ) ) ;
#5193 = CARTESIAN_POINT ( 'NONE',  ( 85.12499999726881583, 155.0000000000000000, -15.58253175000000823 ) ) ;
#5194 = CARTESIAN_POINT ( 'NONE',  ( 0.000000000000000000, 0.000000000000000000, 0.000000000000000000 ) ) ;
#5195 = CARTESIAN_POINT ( 'NONE',  ( 2.517493886308900919, 214.5937144450984420, 88.40113791807857524 ) ) ;
#5196 = CARTESIAN_POINT ( 'NONE',  ( -67.50000000000000000, -92.00000000000000000, -17.00000000000001421 ) ) ;
#5197 = DIRECTION ( 'NONE',  ( -1.000000000000000000, 2.385244779468109755E-17, -3.081487911019577365E-33 ) ) ;
#5198 = CARTESIAN_POINT ( 'NONE',  ( 51.19999999999999574, 167.3344367211045096, 8.961492836873468093 ) ) ;
#5199 = CARTESIAN_POINT ( 'NONE',  ( -0.05014649552828365914, 215.4116977939061144, 63.24886208192142334 ) ) ;
#5200 = CARTESIAN_POINT ( 'NONE',  ( 0.000000000000000000, 0.000000000000000000, 2.066666666667000385 ) ) ;
#5201 = ADVANCED_FACE ( 'NONE', ( #19068 ), #26631, .T. ) ;
#5202 = EDGE_CURVE ( 'NONE', #1337, #29025, #8726, .T. ) ;
#5203 = CARTESIAN_POINT ( 'NONE',  ( 53.72499999726881015, 169.8198683612136222, 4.815267126137181997 ) ) ;
#5204 = DIRECTION ( 'NONE',  ( 0.000000000000000000, 0.000000000000000000, -1.000000000000000000 ) ) ;
#5205 = DIRECTION ( 'NONE',  ( -1.000000000000000000, 0.000000000000000000, 0.000000000000000000 ) ) ;
#5206 = CARTESIAN_POINT ( 'NONE',  ( 56.72499999726881015, 140.1801316387863778, -4.815267126137194431 ) ) ;
#5207 = CARTESIAN_POINT ( 'NONE',  ( 68.97499999726881015, 140.1801316387863778, -4.815267126137194431 ) ) ;
#5208 = CARTESIAN_POINT ( 'NONE',  ( 9.680171189290831535, 199.9079932115568852, 65.30113791807858092 ) ) ;
#5209 = CARTESIAN_POINT ( 'NONE',  ( 46.21132485994280614, 170.7719333635740497, -7.904646289410545231E-15 ) ) ;
#5210 = CARTESIAN_POINT ( 'NONE',  ( 7.375838497908181246, 196.7627149292499666, 5.451137918078566180 ) ) ;
#5211 = ADVANCED_FACE ( 'NONE', ( #1172 ), #32176, .T. ) ;
#5212 = CARTESIAN_POINT ( 'NONE',  ( 6.139770520408367460, 198.4640165459539389, 86.45113791807857240 ) ) ;
#5213 = CARTESIAN_POINT ( 'NONE',  ( 0.05014649552828288198, 194.3824533091408000, 52.74886208192143755 ) ) ;
#5214 = CARTESIAN_POINT ( 'NONE',  ( -3.135527875058982783, 216.4958274776886924, 57.09886208192143187 ) ) ;
#5215 = CARTESIAN_POINT ( 'NONE',  ( 7.456977232089302632, 217.1783343296989131, 100.5511379180785809 ) ) ;
#5216 = PLANE ( 'NONE',  #32771 ) ;
#5217 = CARTESIAN_POINT ( 'NONE',  ( 3.044812012440130555, 197.4746971517856764, 14.60113791807856565 ) ) ;
#5218 = EDGE_CURVE ( 'NONE', #19176, #25951, #3228, .T. ) ;
#5219 = CARTESIAN_POINT ( 'NONE',  ( -6.220909254589682469, 215.4770327129946850, 83.94886208192143329 ) ) ;
#5220 = VERTEX_POINT ( 'NONE', #11569 ) ;
#5221 = CARTESIAN_POINT ( 'NONE',  ( -7.375838497908014268, 196.7627149292498530, 80.04886208192144181 ) ) ;
#5222 = CARTESIAN_POINT ( 'NONE',  ( 8.118202686958039038, 212.8392687619912635, 97.70113791807857240 ) ) ;
#5223 = VERTEX_POINT ( 'NONE', #29294 ) ;
#5224 = CARTESIAN_POINT ( 'NONE',  ( 3.273409709747122864, 207.3577873115561943, -8.276342481318904376 ) ) ;
#5225 = CARTESIAN_POINT ( 'NONE',  ( 8.015496119326595448, 204.4483345814782638, 52.14886208192145034 ) ) ;
#5226 = ORIENTED_EDGE ( 'NONE', *, *, #26790, .T. ) ;
#5227 =( BOUNDED_CURVE ( )  B_SPLINE_CURVE ( 2, ( #13125, #186, #10584, #17910, #11406, #18898, #1011, #3061, #3390, #21617, #21458 ),
 .UNSPECIFIED., .F., .T. ) 
 B_SPLINE_CURVE_WITH_KNOTS ( ( 3, 2, 2, 2, 2, 3 ),
 ( 0.1071428571428569843, 0.1107142857142855291, 0.1142857142857140879, 0.1178571428571426327, 0.1214285714285711915, 0.1249999999999998473 ),
 .UNSPECIFIED. ) 
 CURVE ( )  GEOMETRIC_REPRESENTATION_ITEM ( )  RATIONAL_B_SPLINE_CURVE ( ( 1.000000000000001554, 0.9510565162951518658, 1.000000000000000000, 0.9510565162951534202, 1.000000000000000000, 0.9510565162951534202, 1.000000000000000000, 0.9510565162951534202, 1.000000000000000000, 0.9510565162951555296, 0.9999999999999978906 ) ) 
 REPRESENTATION_ITEM ( '' )  );
#5228 = CARTESIAN_POINT ( 'NONE',  ( 69.92499999726881299, 164.1591823560292198, 12.60653300113718167 ) ) ;
#5229 = DIRECTION ( 'NONE',  ( 1.000000000000000000, 0.000000000000000000, 0.000000000000000000 ) ) ;
#5230 = DIRECTION ( 'NONE',  ( 0.000000000000000000, -1.000000000000000000, 1.295896757998781966E-15 ) ) ;
#5231 = CARTESIAN_POINT ( 'NONE',  ( 60.72499999726881015, 140.1801316387863778, -4.815267126137194431 ) ) ;
#5232 = CARTESIAN_POINT ( 'NONE',  ( -7.499999999999999112, -4.652405105468739421, -7.929127756970856034 ) ) ;
#5233 = CARTESIAN_POINT ( 'NONE',  ( -8.118202686958138514, 212.8392687619910930, 53.79886208192143471 ) ) ;
#5234 = EDGE_CURVE ( 'NONE', #3669, #1409, #24012, .T. ) ;
#5235 = AXIS2_PLACEMENT_3D ( 'NONE', #23111, #12546, #22937 ) ;
#5236 = ORIENTED_EDGE ( 'NONE', *, *, #20639, .F. ) ;
#5237 = DIRECTION ( 'NONE',  ( 0.000000000000000000, 0.5000000000000013323, 0.8660254037844379305 ) ) ;
#5238 = CARTESIAN_POINT ( 'NONE',  ( 4.200000000000001954, 0.000000000000000000, 0.000000000000000000 ) ) ;
#5239 = CARTESIAN_POINT ( 'NONE',  ( 2.426778023690075337, 214.6231898156240447, 33.39886208192144323 ) ) ;
#5240 = CARTESIAN_POINT ( 'NONE',  ( -0.05014649552810635652, 196.4853777576173002, 74.75113791807858377 ) ) ;
#5241 = CARTESIAN_POINT ( 'NONE',  ( -3.499999999999997780, -2.020725942163716038, -2.899999999999999911 ) ) ;
#5242 = CARTESIAN_POINT ( 'NONE',  ( 6.220909254589536808, 215.4770327129947702, 58.55113791807858092 ) ) ;
#5243 = CARTESIAN_POINT ( 'NONE',  ( 9.984503880673470277, 203.7031108863295401, 32.15113791807857524 ) ) ;
#5244 = CARTESIAN_POINT ( 'NONE',  ( -0.05014649552807731031, 198.5883022060938572, 11.75113791807856600 ) ) ;
#5245 = CARTESIAN_POINT ( 'NONE',  ( 111.1125082318798007, 155.0000000000000000, -32.00000000000002842 ) ) ;
#5246 = CYLINDRICAL_SURFACE ( 'NONE', #17117, 32.00000000000002842 ) ;
#5247 = CARTESIAN_POINT ( 'NONE',  ( 37.02499999726880731, 149.9369285172503510, -15.58253175000000823 ) ) ;
#5248 = CARTESIAN_POINT ( 'NONE',  ( 3.753561863808689836, 218.3979405102790565, 37.40113791807856813 ) ) ;
#5249 = CARTESIAN_POINT ( 'NONE',  ( 32.50000000000000000, 155.0000000000000000, -6.938893903907228378E-15 ) ) ;
#5250 = CARTESIAN_POINT ( 'NONE',  ( 6.139770520408368348, 198.4640165459539674, 89.45113791807857240 ) ) ;
#5251 = CARTESIAN_POINT ( 'NONE',  ( 10.01549611932653860, 210.2015048109876716, 58.85113791807857098 ) ) ;
#5252 = CARTESIAN_POINT ( 'NONE',  ( 117.5000000000000000, 127.5651812191323557, -102.3881375866411645 ) ) ;
#5253 = CARTESIAN_POINT ( 'NONE',  ( 7.375838497908012492, 217.2372850707501186, 27.54886208192144181 ) ) ;
#5254 = CARTESIAN_POINT ( 'NONE',  ( 3.044812012439969795, 216.5253028482143520, 27.39886208192143613 ) ) ;
#5255 = CARTESIAN_POINT ( 'NONE',  ( 79.19999999453763451, 146.4771138417591203, 11.73074641843673227 ) ) ;
#5256 = CARTESIAN_POINT ( 'NONE',  ( -7.375838497908182134, 217.2372850707499765, 66.95113791807857240 ) ) ;
#5257 = CARTESIAN_POINT ( 'NONE',  ( 6.444103211791042618, 202.2591342207267644, 89.30113791807858092 ) ) ;
#5258 = CARTESIAN_POINT ( 'NONE',  ( -0.05014649552828403384, 217.5146222423826714, 39.24886208192142334 ) ) ;
#5259 = CIRCLE ( 'NONE', #9047, 4.057500000000000107 ) ;
#5260 = CARTESIAN_POINT ( 'NONE',  ( 75.51132485994280330, 146.1832212156128890, -12.13525491562423042 ) ) ;
#5261 = VERTEX_POINT ( 'NONE', #8505 ) ;
#5262 = CARTESIAN_POINT ( 'NONE',  ( 12.00000000000000711, 207.0476921513415220, 48.99886208192143044 ) ) ;
#5263 = ORIENTED_EDGE ( 'NONE', *, *, #30605, .T. ) ;
#5264 = ORIENTED_EDGE ( 'NONE', *, *, #7911, .F. ) ;
#5265 = VECTOR ( 'NONE', #1502, 1000.000000000000000 ) ;
#5266 = CARTESIAN_POINT ( 'NONE',  ( 6.837824896291514243, 3.947820044545427454, -6.564402953523716278 ) ) ;
#5267 = CARTESIAN_POINT ( 'NONE',  ( 0.000000000000000000, 0.000000000000000000, -7.974599999999998801 ) ) ;
#5268 = ORIENTED_EDGE ( 'NONE', *, *, #20104, .T. ) ;
#5269 = CARTESIAN_POINT ( 'NONE',  ( -6.444103211791042618, 211.7408657792732356, 45.80113791807857382 ) ) ;
#5270 = CARTESIAN_POINT ( 'NONE',  ( 82.71132485994282035, 155.0000000000000000, 15.00000000000001243 ) ) ;
#5271 = CARTESIAN_POINT ( 'NONE',  ( -9.984503880673420539, 203.7031108863293980, 20.34886208192143187 ) ) ;
#5272 = CARTESIAN_POINT ( 'NONE',  ( 60.37499999726880873, 155.0000000000000000, 15.58253174999999402 ) ) ;
#5273 = EDGE_LOOP ( 'NONE', ( #649, #29485, #28143, #26822, #653 ) ) ;
#5274 = CARTESIAN_POINT ( 'NONE',  ( 105.0134430565187387, 155.0000000000000000, 0.000000000000000000 ) ) ;
#5275 = CARTESIAN_POINT ( 'NONE',  ( 32.50000000000000000, 155.0000000000000000, -6.938893903907228378E-15 ) ) ;
#5276 = CARTESIAN_POINT ( 'NONE',  ( 0.05014649552828262524, 198.5883022060938572, 7.748862081921434886 ) ) ;
#5277 = VECTOR ( 'NONE', #17549, 1000.000000000000000 ) ;
#5278 = CARTESIAN_POINT ( 'NONE',  ( 6.220909254589536808, 215.4770327129947702, 43.55113791807857382 ) ) ;
#5279 = CARTESIAN_POINT ( 'NONE',  ( 121.3406204335659879, 155.0000000000000000, -6.938893903907228378E-15 ) ) ;
#5280 = CARTESIAN_POINT ( 'NONE',  ( 9.984503880673470277, 203.7031108863295401, 26.15113791807856813 ) ) ;
#5281 = LINE ( 'NONE', #18239, #15726 ) ;
#5282 = AXIS2_PLACEMENT_3D ( 'NONE', #28932, #2878, #316 ) ;
#5283 = APPLICATION_PROTOCOL_DEFINITION ( 'draft international standard', 'automotive_design', 1998, #20073 ) ;
#5284 = AXIS2_PLACEMENT_3D ( 'NONE', #25891, #28451, #26066 ) ;
#5285 = CARTESIAN_POINT ( 'NONE',  ( 6.500168698208244500, 202.3363017425938324, 88.29886208192142760 ) ) ;
#5286 = CARTESIAN_POINT ( 'NONE',  ( 34.22499999726881015, 149.9369285172503510, 15.58253174999999580 ) ) ;
#5287 = CARTESIAN_POINT ( 'NONE',  ( 105.0134430565187387, 155.0000000000000000, -31.00000000000000000 ) ) ;
#5288 = DIRECTION ( 'NONE',  ( -0.8191520442889907994, 1.003171929053523514E-16, 0.5735764363510474917 ) ) ;
#5289 = CARTESIAN_POINT ( 'NONE',  ( 11.98450388067348271, 203.0532714938637753, 14.15113791807856991 ) ) ;
#5290 = DIRECTION ( 'NONE',  ( -1.000000000000000000, 0.000000000000000000, 0.000000000000000000 ) ) ;
#5291 = CARTESIAN_POINT ( 'NONE',  ( 57.87499999726880873, 171.3844434931184253, -7.942151717890132712E-15 ) ) ;
#5292 = CARTESIAN_POINT ( 'NONE',  ( 9.984503880673470277, 203.7031108863295401, 53.15113791807857524 ) ) ;
#5293 = AXIS2_PLACEMENT_3D ( 'NONE', #22069, #32452, #9121 ) ;
#5294 = CARTESIAN_POINT ( 'NONE',  ( 0.000000000000000000, 0.000000000000000000, -7.974599999999998801 ) ) ;
#5295 = DIRECTION ( 'NONE',  ( 0.000000000000000000, 0.000000000000000000, -1.000000000000000000 ) ) ;
#5296 = LINE ( 'NONE', #23852, #3197 ) ;
#5297 = CARTESIAN_POINT ( 'NONE',  ( 59.19999999453762740, 146.4771138417591203, 11.73074641843673227 ) ) ;
#5298 = ORIENTED_EDGE ( 'NONE', *, *, #29583, .T. ) ;
#5299 = CARTESIAN_POINT ( 'NONE',  ( -0.05014649552807705357, 194.3824533091408000, 35.75113791807857666 ) ) ;
#5300 = CARTESIAN_POINT ( 'NONE',  ( 125.5000000000000000, 48.99999999999998579, -1.387778780781445676E-14 ) ) ;
#5301 = ADVANCED_FACE ( 'NONE', ( #21785 ), #21288, .T. ) ;
#5302 = CARTESIAN_POINT ( 'NONE',  ( 3.135527875058981895, 197.5041725223112792, 7.598862081921435419 ) ) ;
#5303 = DIRECTION ( 'NONE',  ( 0.9396926207859072067, 4.188538737677028743E-17, 0.3420201433256717105 ) ) ;
#5304 = ORIENTED_EDGE ( 'NONE', *, *, #11411, .T. ) ;
#5305 = CARTESIAN_POINT ( 'NONE',  ( -10.01549611932653860, 203.7984951890123284, 69.35113791807857808 ) ) ;
#5306 = AXIS2_PLACEMENT_3D ( 'NONE', #15289, #2352, #23133 ) ;
#5307 = ORIENTED_EDGE ( 'NONE', *, *, #29774, .T. ) ;
#5308 = CARTESIAN_POINT ( 'NONE',  ( 6.444103211790928043, 211.7408657792734061, 36.69886208192144039 ) ) ;
#5309 = AXIS2_PLACEMENT_3D ( 'NONE', #3663, #21890, #14562 ) ;
#5310 = STYLED_ITEM ( 'NONE', ( #16991 ), #951 ) ;
#5311 = AXIS2_PLACEMENT_3D ( 'NONE', #7275, #18002, #33333 ) ;
#5312 = CARTESIAN_POINT ( 'NONE',  ( 79.88867513459481984, 150.1262045565063374, 14.99999999999994316 ) ) ;
#5313 = ORIENTED_EDGE ( 'NONE', *, *, #3875, .T. ) ;
#5314 = CARTESIAN_POINT ( 'NONE',  ( 8.000000000000008882, 206.9523078486586485, 17.00113791807856956 ) ) ;
#5315 = CARTESIAN_POINT ( 'NONE',  ( 11.98450388067341876, 210.9467285061363953, 99.84886208192143897 ) ) ;
#5316 = CARTESIAN_POINT ( 'NONE',  ( 42.77499999726880731, 140.1801316387863778, 4.815267126137185549 ) ) ;
#5317 = ORIENTED_EDGE ( 'NONE', *, *, #20997, .F. ) ;
#5318 = CARTESIAN_POINT ( 'NONE',  ( 52.82499999726880446, 141.7447067706911810, -9.630534252274385310 ) ) ;
#5319 = CARTESIAN_POINT ( 'NONE',  ( 7.499999999999999112, 2.575910028905302074, -0.3641256808890108720 ) ) ;
#5320 = CARTESIAN_POINT ( 'NONE',  ( 6.220909254589536808, 215.4770327129947702, 10.55113791807856138 ) ) ;
#5321 = CARTESIAN_POINT ( 'NONE',  ( -8.118202686958138514, 212.8392687619910930, 83.79886208192144181 ) ) ;
#5322 = CARTESIAN_POINT ( 'NONE',  ( 53.37499999726881583, 155.0000000000000000, -15.58253175000000823 ) ) ;
#5323 = CARTESIAN_POINT ( 'NONE',  ( -67.50001199999999812, 147.4664294917440373, 15.28016032735713559 ) ) ;
#5324 = CARTESIAN_POINT ( 'NONE',  ( -6.220909254589537696, 198.5229672870051161, 9.051137918078561384 ) ) ;
#5325 = CARTESIAN_POINT ( 'NONE',  ( 44.58867513459481557, 146.1832212156128890, -12.13525491562423042 ) ) ;
#5326 = CARTESIAN_POINT ( 'NONE',  ( 65.10000000000000853, 168.7903194862797420, 4.480746418436729606 ) ) ;
#5327 = CARTESIAN_POINT ( 'NONE',  ( -9.984503880673473830, 210.2968891136704315, 96.65113791807857524 ) ) ;
#5328 = CARTESIAN_POINT ( 'NONE',  ( 14.91983402814537563, 23.14029461301514345, -0.01440555954223494972 ) ) ;
#5329 = CARTESIAN_POINT ( 'NONE',  ( 0.05014649552810505201, 217.5146222423826714, 82.25113791807858377 ) ) ;
#5330 = TOROIDAL_SURFACE ( 'NONE', #23827, 5.400000000000002132, 0.4000000000000000222 ) ;
#5331 = CARTESIAN_POINT ( 'NONE',  ( -64.50000000000000000, 2.605762844159070557, -20.00000000000000000 ) ) ;
#5332 = CARTESIAN_POINT ( 'NONE',  ( 37.67499999726881299, 168.2552932293087906, -9.630534252274385310 ) ) ;
#5333 = CARTESIAN_POINT ( 'NONE',  ( -9.680171189290716072, 199.9079932115567146, 101.1988620819214475 ) ) ;
#5334 = AXIS2_PLACEMENT_3D ( 'NONE', #25462, #10141, #20359 ) ;
#5335 = CARTESIAN_POINT ( 'NONE',  ( 69.92499999726881299, 164.1591823560292198, 12.60653300113718167 ) ) ;
#5336 = MECHANICAL_DESIGN_GEOMETRIC_PRESENTATION_REPRESENTATION (  '', ( #21089 ), #32508 ) ;
#5337 = VERTEX_POINT ( 'NONE', #23844 ) ;
#5338 = DIRECTION ( 'NONE',  ( -1.000000000000000000, 0.000000000000000000, 0.000000000000000000 ) ) ;
#5339 = CARTESIAN_POINT ( 'NONE',  ( 34.79999999453762882, 163.5228861582408797, 11.73074641843673049 ) ) ;
#5340 = CARTESIAN_POINT ( 'NONE',  ( 7.456977232089302632, 217.1783343296989131, 94.55113791807855250 ) ) ;
#5341 = DIRECTION ( 'NONE',  ( 1.000000000000000000, 0.000000000000000000, 0.000000000000000000 ) ) ;
#5342 = EDGE_CURVE ( 'NONE', #33380, #29176, #13632, .T. ) ;
#5343 = VECTOR ( 'NONE', #26085, 1000.000000000000000 ) ;
#5344 = ORIENTED_EDGE ( 'NONE', *, *, #32854, .T. ) ;
#5345 = CARTESIAN_POINT ( 'NONE',  ( -9.984503880673420539, 203.7031108863293980, 86.34886208192143897 ) ) ;
#5346 = CARTESIAN_POINT ( 'NONE',  ( -3.662846001189865142, 195.5725841191952838, 22.89886208192143613 ) ) ;
#5347 = DIRECTION ( 'NONE',  ( -1.000000000000000000, -0.000000000000000000, 0.000000000000000000 ) ) ;
#5348 = CARTESIAN_POINT ( 'NONE',  ( 3.135527875058820690, 216.4958274776887492, 46.40113791807857524 ) ) ;
#5349 = ORIENTED_EDGE ( 'NONE', *, *, #43, .T. ) ;
#5350 = CARTESIAN_POINT ( 'NONE',  ( -7.984503880673422316, 204.3529502787951628, 5.348862081921435419 ) ) ;
#5351 = ADVANCED_FACE ( 'NONE', ( #31682 ), #518, .F. ) ;
#5352 = CARTESIAN_POINT ( 'NONE',  ( 74.11132485994281183, 169.2658477444273331, -4.635254915624224203 ) ) ;
#5353 = ORIENTED_EDGE ( 'NONE', *, *, #28885, .F. ) ;
#5354 = CARTESIAN_POINT ( 'NONE',  ( -8.000000000000008882, 206.9523078486584780, 92.49886208192144466 ) ) ;
#5355 = CONICAL_SURFACE ( 'NONE', #29307, 11.99999999999998224, 0.1047197551197030924 ) ;
#5356 = ORIENTED_EDGE ( 'NONE', *, *, #20206, .T. ) ;
#5357 = AXIS2_PLACEMENT_3D ( 'NONE', #16149, #990, #26540 ) ;
#5358 = CARTESIAN_POINT ( 'NONE',  ( 2.426778023690261410, 199.3768101843759837, 29.60113791807856742 ) ) ;
#5359 = CARTESIAN_POINT ( 'NONE',  ( 56.61132485994281893, 159.8737954434936057, 15.00000000000001421 ) ) ;
#5360 = EDGE_LOOP ( 'NONE', ( #22959, #5605, #26874, #27254 ) ) ;
#5361 = CARTESIAN_POINT ( 'NONE',  ( 34.32499999726881157, 145.8408176439707802, 12.60653300113718345 ) ) ;
#5362 = CARTESIAN_POINT ( 'NONE',  ( 87.42499999726881299, 168.2552932293087906, -9.630534252274385310 ) ) ;
#5363 = EDGE_CURVE ( 'NONE', #20140, #14728, #29633, .T. ) ;
#5364 = LINE ( 'NONE', #15250, #32274 ) ;
#5365 = CARTESIAN_POINT ( 'NONE',  ( -0.05014649552807731031, 198.5883022060938572, 89.75113791807858377 ) ) ;
#5366 = AXIS2_PLACEMENT_3D ( 'NONE', #1137, #17143, #30261 ) ;
#5367 = CARTESIAN_POINT ( 'NONE',  ( 45.29999999999999716, 163.5228861582408797, 11.73074641843673049 ) ) ;
#5368 = CARTESIAN_POINT ( 'NONE',  ( 7.984503880673422316, 209.6470497212048372, 66.84886208192143897 ) ) ;
#5369 = CARTESIAN_POINT ( 'NONE',  ( 83.81132485994281467, 159.8737954434936057, -15.00000000000002665 ) ) ;
#5370 = EDGE_CURVE ( 'NONE', #6050, #28898, #26683, .T. ) ;
#5371 = CARTESIAN_POINT ( 'NONE',  ( 51.32499999726881157, 164.1591823560292198, -12.60653300113719766 ) ) ;
#5372 = CARTESIAN_POINT ( 'NONE',  ( 8.062137200540920645, 201.0835637161417822, 5.301137918078566713 ) ) ;
#5373 = DIRECTION ( 'NONE',  ( 0.000000000000000000, 0.000000000000000000, -1.000000000000000000 ) ) ;
#5374 = CARTESIAN_POINT ( 'NONE',  ( 66.42499999726881299, 141.7447067706911810, 9.630534252274376428 ) ) ;
#5375 = CARTESIAN_POINT ( 'NONE',  ( 67.17499999726881299, 145.8408176439707802, -12.60653300113719588 ) ) ;
#5376 = CARTESIAN_POINT ( 'NONE',  ( 3.662846001190051659, 195.5725841191953691, 68.60113791807857808 ) ) ;
#5377 = FACE_BOUND ( 'NONE', #11293, .T. ) ;
#5378 = AXIS2_PLACEMENT_3D ( 'NONE', #563, #727, #13838 ) ;
#5379 = CARTESIAN_POINT ( 'NONE',  ( -10.01549611932653860, 203.7984951890123000, 87.35113791807856387 ) ) ;
#5380 = EDGE_CURVE ( 'NONE', #19088, #22486, #21665, .T. ) ;
#5381 = DIRECTION ( 'NONE',  ( 0.000000000000000000, 0.000000000000000000, -1.000000000000000000 ) ) ;
#5382 = VECTOR ( 'NONE', #17641, 1000.000000000000000 ) ;
#5383 = CARTESIAN_POINT ( 'NONE',  ( 3.662846001189864698, 218.4274158808046593, 54.39886208192143613 ) ) ;
#5384 = CARTESIAN_POINT ( 'NONE',  ( 0.05014649552828275708, 196.4853777576173002, 43.74886208192141623 ) ) ;
#5385 = CARTESIAN_POINT ( 'NONE',  ( -6.139770520408224463, 198.4640165459539105, 53.04886208192142760 ) ) ;
#5386 = CARTESIAN_POINT ( 'NONE',  ( 3.753561863808689836, 218.3979405102790565, 94.40113791807857524 ) ) ;
#5387 = CARTESIAN_POINT ( 'NONE',  ( -67.50001199999999812, 156.1126473981464073, 17.00000000000001066 ) ) ;
#5388 = CARTESIAN_POINT ( 'NONE',  ( -8.118202686958039038, 201.1607312380087080, 9.201137918078565292 ) ) ;
#5389 = CARTESIAN_POINT ( 'NONE',  ( 0.05014649552828275708, 196.4853777576173002, 76.74886208192140202 ) ) ;
#5390 = AXIS2_PLACEMENT_3D ( 'NONE', #24568, #273, #32394 ) ;
#5391 = ORIENTED_EDGE ( 'NONE', *, *, #351, .F. ) ;
#5392 = CARTESIAN_POINT ( 'NONE',  ( 3.662846001189864698, 218.4274158808046593, 78.39886208192143613 ) ) ;
#5393 = CARTESIAN_POINT ( 'NONE',  ( 8.062137200540920645, 201.0835637161417822, 95.30113791807858092 ) ) ;
#5394 = VERTEX_POINT ( 'NONE', #3562 ) ;
#5395 = CARTESIAN_POINT ( 'NONE',  ( 3.500000000000004885, 2.020725942163702715, -0.3126073911696551910 ) ) ;
#5396 = CARTESIAN_POINT ( 'NONE',  ( 6.500168698208244500, 202.3363017425938324, 64.29886208192144181 ) ) ;
#5397 = ORIENTED_EDGE ( 'NONE', *, *, #4252, .T. ) ;
#5398 = EDGE_CURVE ( 'NONE', #19921, #18219, #2644, .T. ) ;
#5399 = CARTESIAN_POINT ( 'NONE',  ( 74.92499999726881299, 145.8408176439707802, -12.60653300113719588 ) ) ;
#5400 = DIRECTION ( 'NONE',  ( 1.000000000000000000, 0.000000000000000000, 0.000000000000000000 ) ) ;
#5401 = DIRECTION ( 'NONE',  ( 0.000000000000000000, 0.000000000000000000, 1.000000000000000000 ) ) ;
#5402 = AXIS2_PLACEMENT_3D ( 'NONE', #32682, #14294, #8844 ) ;
#5403 = CARTESIAN_POINT ( 'NONE',  ( 64.42499999726879878, 141.7447067706911810, 9.630534252274376428 ) ) ;
#5404 = EDGE_CURVE ( 'NONE', #16947, #12552, #15663, .T. ) ;
#5405 = CARTESIAN_POINT ( 'NONE',  ( -7.500000000000000000, -3.948305025207388130, -7.349903712356284480 ) ) ;
#5406 = CARTESIAN_POINT ( 'NONE',  ( 6.139770520408223575, 215.5359834540460611, 51.54886208192142050 ) ) ;
#5407 = ORIENTED_EDGE ( 'NONE', *, *, #20406, .T. ) ;
#5408 = FACE_OUTER_BOUND ( 'NONE', #987, .T. ) ;
#5409 = LINE ( 'NONE', #15794, #15409 ) ;
#5410 = CARTESIAN_POINT ( 'NONE',  ( 2.517493886309087436, 199.4062855549015865, 31.59886208192144252 ) ) ;
#5411 = CARTESIAN_POINT ( 'NONE',  ( 3.044812012440130555, 197.4746971517856764, 80.60113791807857808 ) ) ;
#5412 = FACE_BOUND ( 'NONE', #31743, .T. ) ;
#5413 = CARTESIAN_POINT ( 'NONE',  ( 6.220909254589536808, 215.4770327129947702, 52.55113791807858092 ) ) ;
#5414 = CARTESIAN_POINT ( 'NONE',  ( 3.044812012440130555, 197.4746971517856764, 23.60113791807857098 ) ) ;
#5415 = CARTESIAN_POINT ( 'NONE',  ( -2.426778023690262742, 214.6231898156240163, 13.10113791807856742 ) ) ;
#5416 = DIRECTION ( 'NONE',  ( 0.000000000000000000, 0.000000000000000000, -1.000000000000000000 ) ) ;
#5417 = FACE_OUTER_BOUND ( 'NONE', #16351, .T. ) ;
#5418 = CARTESIAN_POINT ( 'NONE',  ( 38.72499999726881015, 140.1801316387863778, -4.815267126137194431 ) ) ;
#5419 = CARTESIAN_POINT ( 'NONE',  ( 3.662846001190051659, 195.5725841191953691, 38.60113791807855677 ) ) ;
#5420 = CYLINDRICAL_SURFACE ( 'NONE', #15138, 3.500000000000000000 ) ;
#5421 = CARTESIAN_POINT ( 'NONE',  ( 10.00000000000000711, 206.9523078486586201, 83.00113791807856956 ) ) ;
#5422 = CARTESIAN_POINT ( 'NONE',  ( -3.044812012440131443, 216.5253028482142952, 55.10113791807857098 ) ) ;
#5423 = CARTESIAN_POINT ( 'NONE',  ( 9.736236675708031640, 199.9851607334238963, 19.29886208192143471 ) ) ;
#5424 = CARTESIAN_POINT ( 'NONE',  ( 3.044812012439969795, 216.5253028482143520, 33.39886208192143613 ) ) ;
#5425 = CARTESIAN_POINT ( 'NONE',  ( 82.19999999453763451, 163.5228861582408797, -11.73074641843674470 ) ) ;
#5426 = CARTESIAN_POINT ( 'NONE',  ( -0.05014649552807705357, 194.3824533091408000, 65.75113791807856956 ) ) ;
#5427 = CIRCLE ( 'NONE', #5402, 13.00000000000001776 ) ;
#5428 = CARTESIAN_POINT ( 'NONE',  ( 6.500168698208129925, 211.6636982574063381, 91.70113791807857240 ) ) ;
#5429 =( BOUNDED_CURVE ( )  B_SPLINE_CURVE ( 2, ( #22178, #32567, #9238, #19628, #27460, #9403, #7022, #17407, #14845, #22859, #27968 ),
 .UNSPECIFIED., .F., .T. ) 
 B_SPLINE_CURVE_WITH_KNOTS ( ( 3, 2, 2, 2, 2, 3 ),
 ( 0.4821428571428572063, 0.4857142857142857650, 0.4892857142857143238, 0.4928571428571428825, 0.4964285714285714413, 0.5000000000000000000 ),
 .UNSPECIFIED. ) 
 CURVE ( )  GEOMETRIC_REPRESENTATION_ITEM ( )  RATIONAL_B_SPLINE_CURVE ( ( 0.9999999999999992228, 0.9510565162951541973, 1.000000000000000000, 0.9510565162951534202, 1.000000000000000000, 0.9510565162951534202, 1.000000000000000000, 0.9510565162951534202, 1.000000000000000000, 0.9510565162951534202, 1.000000000000000000 ) ) 
 REPRESENTATION_ITEM ( '' )  );
#5430 = CARTESIAN_POINT ( 'NONE',  ( 6.139770520408223575, 215.5359834540460611, 51.54886208192142050 ) ) ;
#5431 = CARTESIAN_POINT ( 'NONE',  ( 0.000000000000000000, 0.000000000000000000, -2.899999999999999911 ) ) ;
#5432 = ORIENTED_EDGE ( 'NONE', *, *, #24927, .T. ) ;
#5433 = CARTESIAN_POINT ( 'NONE',  ( -11.98450388067341876, 203.0532714938636047, 56.34886208192143187 ) ) ;
#5434 = EDGE_LOOP ( 'NONE', ( #26715, #23542, #17197, #8727, #19054 ) ) ;
#5435 = ORIENTED_EDGE ( 'NONE', *, *, #22701, .F. ) ;
#5436 = EDGE_CURVE ( 'NONE', #18269, #18184, #27091, .T. ) ;
#5437 = EDGE_CURVE ( 'NONE', #10401, #5683, #4797, .T. ) ;
#5438 = CARTESIAN_POINT ( 'NONE',  ( 51.08867513459482979, 167.7597621252805880, -9.270509831248443078 ) ) ;
#5439 = CYLINDRICAL_SURFACE ( 'NONE', #21978, 15.00000000000001776 ) ;
#5440 = CARTESIAN_POINT ( 'NONE',  ( 8.015496119326531499, 209.5516654185219636, 46.85113791807857098 ) ) ;
#5441 = PRODUCT_RELATED_PRODUCT_CATEGORY ( 'part', '', ( #25205 ) ) ;
#5442 = EDGE_CURVE ( 'NONE', #20128, #3832, #10270, .T. ) ;
#5443 = FILL_AREA_STYLE_COLOUR ( '', #24313 ) ;
#5444 = CARTESIAN_POINT ( 'NONE',  ( -10.00000000000000711, 206.9523078486584495, 20.49886208192143755 ) ) ;
#5445 = CARTESIAN_POINT ( 'NONE',  ( 64.67499999726879878, 141.7447067706911810, 9.630534252274376428 ) ) ;
#5446 = ORIENTED_EDGE ( 'NONE', *, *, #20018, .F. ) ;
#5447 = CARTESIAN_POINT ( 'NONE',  ( 46.78867513459482552, 155.0000000000000000, -15.00000000000002487 ) ) ;
#5448 = CARTESIAN_POINT ( 'NONE',  ( -4.903702542908436435, 200.1653181626580249, 8.048862081921434708 ) ) ;
#5449 = CARTESIAN_POINT ( 'NONE',  ( -6.139770520408369237, 215.5359834540460042, 39.95113791807857240 ) ) ;
#5450 = CARTESIAN_POINT ( 'NONE',  ( -7.640563834021360018E-16, -9.147862274876560562, -8.047472243342937759 ) ) ;
#5451 = PRODUCT_DEFINITION_SHAPE ( 'NONE', 'NONE',  #33706 ) ;
#5452 = CARTESIAN_POINT ( 'NONE',  ( 10.01549611932653860, 210.2015048109876716, 31.85113791807857453 ) ) ;
#5453 = CARTESIAN_POINT ( 'NONE',  ( 0.05014649552828275014, 196.4853777576173002, 103.7488620819214589 ) ) ;
#5454 = APPLICATION_PROTOCOL_DEFINITION ( 'draft international standard', 'automotive_design', 1998, #16582 ) ;
#5455 = CARTESIAN_POINT ( 'NONE',  ( 8.015496119326595448, 204.4483345814782638, 94.14886208192145034 ) ) ;
#5456 = CARTESIAN_POINT ( 'NONE',  ( 35.92499999726880588, 164.1591823560292198, 12.60653300113718167 ) ) ;
#5457 = CARTESIAN_POINT ( 'NONE',  ( -27.50000000000000000, -15.87713240271474824, -2.456200930618646971 ) ) ;
#5458 = DIRECTION ( 'NONE',  ( -1.000000000000000000, 0.000000000000000000, 0.000000000000000000 ) ) ;
#5459 = B_SPLINE_CURVE_WITH_KNOTS ( 'NONE', 3,
 ( #32209, #3770, #11440, #9217, #22155, #6496 ),
 .UNSPECIFIED., .F., .F.,
 ( 4, 2, 4 ),
 ( 2.380727408877235103E-07, 0.008032766472079745299, 0.01606529487141860474 ),
 .UNSPECIFIED. ) ;
#5460 = CARTESIAN_POINT ( 'NONE',  ( -3.753561863808691168, 195.6020594897209435, 5.901137918078566358 ) ) ;
#5461 = DIRECTION ( 'NONE',  ( 0.000000000000000000, 0.000000000000000000, 1.000000000000000000 ) ) ;
#5462 = CARTESIAN_POINT ( 'NONE',  ( 60.37499999726880873, 155.0000000000000000, 15.58253174999999402 ) ) ;
#5463 = CARTESIAN_POINT ( 'NONE',  ( -3.044812012440131443, 216.5253028482142952, 55.10113791807857098 ) ) ;
#5464 = CARTESIAN_POINT ( 'NONE',  ( 6.220909254589536808, 215.4770327129947987, 31.55113791807856671 ) ) ;
#5465 = CARTESIAN_POINT ( 'NONE',  ( -67.50000000000000000, 155.0000000000000000, 37.00000000000001421 ) ) ;
#5466 = CARTESIAN_POINT ( 'NONE',  ( -63.49999999999884892, 215.0000000000003979, 0.000000000000000000 ) ) ;
#5467 = LINE ( 'NONE', #7867, #2119 ) ;
#5468 = CARTESIAN_POINT ( 'NONE',  ( 61.19999999453762740, 146.4771138417591203, 11.73074641843673227 ) ) ;
#5469 = EDGE_LOOP ( 'NONE', ( #10219, #15728, #33186, #21722, #19459 ) ) ;
#5470 = CARTESIAN_POINT ( 'NONE',  ( -3.753561863808691168, 195.6020594897209435, 35.90113791807856813 ) ) ;
#5471 = CARTESIAN_POINT ( 'NONE',  ( 76.81132485994282888, 150.1262045565065364, 15.00000000000011191 ) ) ;
#5472 = CARTESIAN_POINT ( 'NONE',  ( 0.05014649552828275708, 196.4853777576173002, 22.74886208192142689 ) ) ;
#5473 = LINE ( 'NONE', #31537, #24283 ) ;
#5474 = ORIENTED_EDGE ( 'NONE', *, *, #2117, .T. ) ;
#5475 = CARTESIAN_POINT ( 'NONE',  ( 3.044812012440130555, 197.4746971517856764, 74.60113791807856387 ) ) ;
#5476 = VERTEX_POINT ( 'NONE', #12240 ) ;
#5477 = DIRECTION ( 'NONE',  ( -1.000000000000000000, 0.000000000000000000, 0.000000000000000000 ) ) ;
#5478 = FACE_OUTER_BOUND ( 'NONE', #15118, .T. ) ;
#5479 = ORIENTED_EDGE ( 'NONE', *, *, #29715, .F. ) ;
#5480 = CARTESIAN_POINT ( 'NONE',  ( 6.500168698208129925, 211.6636982574063381, 10.70113791807856529 ) ) ;
#5481 = CARTESIAN_POINT ( 'NONE',  ( 0.05014649552828288198, 194.3824533091408000, 94.74886208192144466 ) ) ;
#5482 = CARTESIAN_POINT ( 'NONE',  ( 42.37499999726881583, 155.0000000000000000, 15.58253174999999402 ) ) ;
#5483 = VERTEX_POINT ( 'NONE', #2023 ) ;
#5484 = CARTESIAN_POINT ( 'NONE',  ( 49.32499999726881157, 164.1591823560292198, -12.60653300113719766 ) ) ;
#5485 = EDGE_CURVE ( 'NONE', #5632, #16267, #29820, .T. ) ;
#5486 = DIRECTION ( 'NONE',  ( 0.000000000000000000, 0.000000000000000000, 1.000000000000000000 ) ) ;
#5487 = CARTESIAN_POINT ( 'NONE',  ( -8.062137200540920645, 212.9164362838581894, 9.801137918078566713 ) ) ;
#5488 = CARTESIAN_POINT ( 'NONE',  ( -6.220909254589682469, 215.4770327129946850, 77.94886208192140487 ) ) ;
#5489 = CARTESIAN_POINT ( 'NONE',  ( 52.77499999726881441, 140.1801316387863778, 4.815267126137185549 ) ) ;
#5490 = DIRECTION ( 'NONE',  ( 1.000000000000000000, -0.000000000000000000, -0.000000000000000000 ) ) ;
#5491 = CARTESIAN_POINT ( 'NONE',  ( -8.118202686958039038, 201.1607312380087080, 15.20113791807856884 ) ) ;
#5492 = CYLINDRICAL_SURFACE ( 'NONE', #21386, 15.00000000000001776 ) ;
#5493 = CARTESIAN_POINT ( 'NONE',  ( 66.80000000000001137, 167.3344367211045096, -8.961492836873482304 ) ) ;
#5494 = CARTESIAN_POINT ( 'NONE',  ( 9.984503880673470277, 203.7031108863295401, 101.1511379180785752 ) ) ;
#5495 = DIRECTION ( 'NONE',  ( 0.000000000000000000, 1.000000000000000000, 0.000000000000000000 ) ) ;
#5496 = CARTESIAN_POINT ( 'NONE',  ( 10.00000000000000711, 206.9523078486586201, 89.00113791807858377 ) ) ;
#5497 = CARTESIAN_POINT ( 'NONE',  ( 57.48867513459482126, 167.7597621252805880, 9.270509831248428867 ) ) ;
#5498 = CARTESIAN_POINT ( 'NONE',  ( 39.67499999726881299, 168.2552932293087906, -9.630534252274385310 ) ) ;
#5499 = CARTESIAN_POINT ( 'NONE',  ( -3.662846001189865142, 195.5725841191952838, 97.89886208192146455 ) ) ;
#5500 = CARTESIAN_POINT ( 'NONE',  ( 71.02499999726882152, 149.9369285172503510, -15.58253175000000823 ) ) ;
#5501 = VERTEX_POINT ( 'NONE', #4066 ) ;
#5502 = CARTESIAN_POINT ( 'NONE',  ( 48.71132485994280614, 155.0000000000000000, 15.00000000000001243 ) ) ;
#5503 = CARTESIAN_POINT ( 'NONE',  ( 42.49999999453763166, 170.2462022514548323, -7.872454543227099337E-15 ) ) ;
#5504 = CARTESIAN_POINT ( 'NONE',  ( -9.680171189290716072, 199.9079932115567146, 2.198862081921433731 ) ) ;
#5505 = CARTESIAN_POINT ( 'NONE',  ( 2.926493552096022466, 2.351840044243029393, -2.761158938895390325 ) ) ;
#5506 = VERTEX_POINT ( 'NONE', #25353 ) ;
#5507 = CARTESIAN_POINT ( 'NONE',  ( 9.984503880673420539, 210.2968891136705736, 93.84886208192143897 ) ) ;
#5508 = CIRCLE ( 'NONE', #15841, 0.6186547224754559426 ) ;
#5509 = CARTESIAN_POINT ( 'NONE',  ( -9.680171189290716072, 199.9079932115567146, 35.19886208192142618 ) ) ;
#5510 = DIRECTION ( 'NONE',  ( 0.000000000000000000, 0.000000000000000000, 1.000000000000000000 ) ) ;
#5511 = CARTESIAN_POINT ( 'NONE',  ( 0.05014649552810505201, 217.5146222423826714, 40.25113791807856956 ) ) ;
#5512 = EDGE_LOOP ( 'NONE', ( #20983, #9749, #20862, #21763 ) ) ;
#5513 = CARTESIAN_POINT ( 'NONE',  ( 6.444103211790928043, 211.7408657792734061, 3.698862081921435063 ) ) ;
#5514 = CARTESIAN_POINT ( 'NONE',  ( -1.750000000000014211, 3.031088913245526317, 0.000000000000000000 ) ) ;
#5515 = VERTEX_POINT ( 'NONE', #33014 ) ;
#5516 = CARTESIAN_POINT ( 'NONE',  ( 8.015496119326595448, 204.4483345814782638, 94.14886208192145034 ) ) ;
#5517 = CARTESIAN_POINT ( 'NONE',  ( 2.426778023690261410, 199.3768101843759837, 32.60113791807857098 ) ) ;
#5518 = DIRECTION ( 'NONE',  ( 1.000000000000000000, 0.000000000000000000, 0.000000000000000000 ) ) ;
#5519 = ORIENTED_EDGE ( 'NONE', *, *, #381, .T. ) ;
#5520 = DIRECTION ( 'NONE',  ( 1.000000000000000000, -0.000000000000000000, -0.000000000000000000 ) ) ;
#5521 = CARTESIAN_POINT ( 'NONE',  ( 87.62499999726880162, 171.3844434931184253, -7.942151717890132712E-15 ) ) ;
#5522 = PLANE ( 'NONE',  #10534 ) ;
#5523 = CARTESIAN_POINT ( 'NONE',  ( 8.000000000000008882, 206.9523078486586485, 89.00113791807858377 ) ) ;
#5524 = EDGE_CURVE ( 'NONE', #9319, #5515, #22381, .T. ) ;
#5525 = VECTOR ( 'NONE', #13656, 1000.000000000000000 ) ;
#5526 = CARTESIAN_POINT ( 'NONE',  ( 0.000000000000000000, 0.000000000000000000, 0.000000000000000000 ) ) ;
#5527 = CARTESIAN_POINT ( 'NONE',  ( 48.20000000000000995, 142.6655632788954620, -8.961492836873480528 ) ) ;
#5528 = CARTESIAN_POINT ( 'NONE',  ( -8.015496119326597224, 209.5516654185217362, 65.64886208192142192 ) ) ;
#5529 = CARTESIAN_POINT ( 'NONE',  ( 84.41132485994282320, 167.7597621252805880, 9.270509831248428867 ) ) ;
#5530 = CARTESIAN_POINT ( 'NONE',  ( 50.12499999726881583, 155.0000000000000000, 15.58253174999999402 ) ) ;
#5532 = EDGE_LOOP ( 'NONE', ( #26013, #2553, #20507, #13710 ) ) ;
#5531 = CARTESIAN_POINT ( 'NONE',  ( 8.062137200540920645, 201.0835637161417822, 14.30113791807856671 ) ) ;
#5533 = DIRECTION ( 'NONE',  ( 0.000000000000000000, 0.000000000000000000, -1.000000000000000000 ) ) ;
#5534 = CONICAL_SURFACE ( 'NONE', #22955, 1.535500000000000087, 1.047197551196590748 ) ;
#5535 = CARTESIAN_POINT ( 'NONE',  ( 61.12499999726880873, 155.0000000000000000, -15.58253175000000823 ) ) ;
#5536 = CARTESIAN_POINT ( 'NONE',  ( 76.27499999726877888, 160.0630714827496206, 15.58253174999999402 ) ) ;
#5537 = CARTESIAN_POINT ( 'NONE',  ( 9.736236675707914401, 214.0148392665762458, 64.70113791807857240 ) ) ;
#5538 = CARTESIAN_POINT ( 'NONE',  ( 87.50000000000001421, 155.0000000000000000, 70.00000000000000000 ) ) ;
#5539 = CARTESIAN_POINT ( 'NONE',  ( 0.05014649552810506589, 217.5146222423826714, 91.25113791807858377 ) ) ;
#5540 = CARTESIAN_POINT ( 'NONE',  ( 84.78867513459482552, 155.0000000000000000, -15.00000000000002487 ) ) ;
#5541 = ORIENTED_EDGE ( 'NONE', *, *, #3976, .F. ) ;
#5542 = CARTESIAN_POINT ( 'NONE',  ( -9.736236675708031640, 214.0148392665760753, 56.79886208192143471 ) ) ;
#5543 = CARTESIAN_POINT ( 'NONE',  ( -6.139770520408224463, 198.4640165459539105, 65.04886208192144181 ) ) ;
#5544 = CARTESIAN_POINT ( 'NONE',  ( -3.662846001190052991, 218.4274158808045740, 97.10113791807857808 ) ) ;
#5545 = CARTESIAN_POINT ( 'NONE',  ( 34.48867513459482126, 142.2402378747194405, -9.270509831248439525 ) ) ;
#5546 = CARTESIAN_POINT ( 'NONE',  ( 3.135527875058820690, 216.4958274776887492, 16.40113791807856813 ) ) ;
#5547 = CARTESIAN_POINT ( 'NONE',  ( 3.135527875058981895, 197.5041725223112792, 79.59886208192143897 ) ) ;
#5548 = ORIENTED_EDGE ( 'NONE', *, *, #30401, .T. ) ;
#5549 = CARTESIAN_POINT ( 'NONE',  ( 6.220909254589536808, 215.4770327129947702, 100.5511379180785809 ) ) ;
#5550 = ORIENTED_EDGE ( 'NONE', *, *, #1853, .F. ) ;
#5551 = CARTESIAN_POINT ( 'NONE',  ( 0.000000000000000000, 0.000000000000000000, 0.000000000000000000 ) ) ;
#5552 = UNCERTAINTY_MEASURE_WITH_UNIT (LENGTH_MEASURE( 1.000000000000000082E-05 ), #29579, 'distance_accuracy_value', 'NONE');
#5553 = CARTESIAN_POINT ( 'NONE',  ( -4.903702542908436435, 200.1653181626580249, 62.04886208192144181 ) ) ;
#5554 = ADVANCED_FACE ( 'NONE', ( #27908 ), #9139, .F. ) ;
#5555 = EDGE_LOOP ( 'NONE', ( #27000, #21510, #4809, #11843 ) ) ;
#5556 = CARTESIAN_POINT ( 'NONE',  ( 78.22499999726881015, 149.9369285172503510, 15.58253174999999580 ) ) ;
#5557 = CARTESIAN_POINT ( 'NONE',  ( -64.50000000000000000, 120.3589838486224437, 20.00000000000000000 ) ) ;
#5558 = DIRECTION ( 'NONE',  ( 0.000000000000000000, 0.000000000000000000, 1.000000000000000000 ) ) ;
#5559 = VECTOR ( 'NONE', #10869, 1000.000000000000000 ) ;
#5560 = AXIS2_PLACEMENT_3D ( 'NONE', #21634, #10924, #23695 ) ;
#5561 = CARTESIAN_POINT ( 'NONE',  ( 72.92499999726881299, 145.8408176439707802, -12.60653300113719588 ) ) ;
#5562 = CARTESIAN_POINT ( 'NONE',  ( -8.015496119326531499, 204.4483345814780364, 63.35113791807857098 ) ) ;
#5563 = LINE ( 'NONE', #22581, #27625 ) ;
#5564 = EDGE_CURVE ( 'NONE', #8437, #19762, #5963, .T. ) ;
#5565 = LINE ( 'NONE', #794, #7813 ) ;
#5566 =( NAMED_UNIT ( * ) PLANE_ANGLE_UNIT ( ) SI_UNIT ( $, .RADIAN. ) );
#5567 = CARTESIAN_POINT ( 'NONE',  ( 59.78867513459481842, 155.0000000000000000, 15.00000000000001243 ) ) ;
#5568 = CARTESIAN_POINT ( 'NONE',  ( 8.015496119326595448, 204.4483345814782638, 37.14886208192143613 ) ) ;
#5569 = CARTESIAN_POINT ( 'NONE',  ( -8.118202686958039038, 201.1607312380087080, 84.20113791807858661 ) ) ;
#5570 = CARTESIAN_POINT ( 'NONE',  ( 6.500000000000000000, 3.752776749732563921, -6.064240316920399110 ) ) ;
#5571 = CARTESIAN_POINT ( 'NONE',  ( -9.984503880673473830, 210.2968891136704315, 63.65113791807857524 ) ) ;
#5572 = ADVANCED_FACE ( 'NONE', ( #25812 ), #30927, .T. ) ;
#5573 = AXIS2_PLACEMENT_3D ( 'NONE', #4273, #27606, #14666 ) ;
#5574 = CARTESIAN_POINT ( 'NONE',  ( 0.05014649552810505201, 217.5146222423826714, 25.25113791807856245 ) ) ;
#5575 = CARTESIAN_POINT ( 'NONE',  ( 4.903702542908601636, 200.1653181626581102, 14.45113791807856707 ) ) ;
#5576 = DIRECTION ( 'NONE',  ( 0.000000000000000000, 0.000000000000000000, -1.000000000000000000 ) ) ;
#5577 = CARTESIAN_POINT ( 'NONE',  ( -5.589124336234651658, 4.278671059406048194, -6.219623095967983240 ) ) ;
#5578 = CARTESIAN_POINT ( 'NONE',  ( 46.32499999726881157, 145.8408176439707802, 12.60653300113718345 ) ) ;
#5579 = CARTESIAN_POINT ( 'NONE',  ( -9.736236675707914401, 199.9851607334237542, 36.20113791807856529 ) ) ;
#5580 = CARTESIAN_POINT ( 'NONE',  ( -130.2500000000000000, -0.6872233929727670221, 35.00001200000000523 ) ) ;
#5581 = CARTESIAN_POINT ( 'NONE',  ( 0.05014649552810505201, 217.5146222423826714, 85.25113791807854113 ) ) ;
#5582 = CARTESIAN_POINT ( 'NONE',  ( -8.118202686958039038, 201.1607312380087080, 60.20113791807857240 ) ) ;
#5583 = CARTESIAN_POINT ( 'NONE',  ( -9.680171189290716072, 199.9079932115567146, 20.19886208192143684 ) ) ;
#5584 = CARTESIAN_POINT ( 'NONE',  ( -9.984503880673420539, 203.7031108863293980, 26.34886208192143187 ) ) ;
#5585 = CARTESIAN_POINT ( 'NONE',  ( 79.09999999453761177, 150.2886644046228639, 14.49999999999999645 ) ) ;
#5586 = VECTOR ( 'NONE', #30769, 1000.000000000000000 ) ;
#5587 = CARTESIAN_POINT ( 'NONE',  ( -3.662846001190052991, 218.4274158808045740, 64.10113791807857808 ) ) ;
#5588 = CARTESIAN_POINT ( 'NONE',  ( -6.500168698208129925, 202.3363017425936050, 93.20113791807858661 ) ) ;
#5589 = VECTOR ( 'NONE', #19251, 1000.000000000000000 ) ;
#5590 = ADVANCED_FACE ( 'NONE', ( #28368 ), #30422, .F. ) ;
#5591 = CARTESIAN_POINT ( 'NONE',  ( 6.139770520408223575, 215.5359834540460611, 54.54886208192144181 ) ) ;
#5592 = CYLINDRICAL_SURFACE ( 'NONE', #4720, 2.500000000000000000 ) ;
#5593 = ORIENTED_EDGE ( 'NONE', *, *, #5342, .F. ) ;
#5594 = CARTESIAN_POINT ( 'NONE',  ( -7.456977232089471386, 217.1783343296987709, 56.94886208192144039 ) ) ;
#5595 = ORIENTED_EDGE ( 'NONE', *, *, #6177, .T. ) ;
#5596 = ADVANCED_FACE ( 'NONE', ( #2304 ), #3689, .T. ) ;
#5597 = VERTEX_POINT ( 'NONE', #31097 ) ;
#5598 = CARTESIAN_POINT ( 'NONE',  ( 77.97499999726881015, 169.8198683612136222, 4.815267126137181997 ) ) ;
#5599 = CARTESIAN_POINT ( 'NONE',  ( 4.000000000000000000, 3.518949890710768802, -4.770489558936219510E-15 ) ) ;
#5600 = AXIS2_PLACEMENT_3D ( 'NONE', #28909, #8299, #29080 ) ;
#5601 = CARTESIAN_POINT ( 'NONE',  ( 56.68867513459484542, 150.1262045565065364, -15.00000000000012434 ) ) ;
#5602 = CARTESIAN_POINT ( 'NONE',  ( -4.903702542908602524, 213.8346818373418898, 42.95113791807857240 ) ) ;
#5603 = CARTESIAN_POINT ( 'NONE',  ( -6.220909254589682469, 215.4770327129946850, 20.94886208192143684 ) ) ;
#5604 = CARTESIAN_POINT ( 'NONE',  ( 62.17499999726882010, 164.1591823560292198, 12.60653300113718167 ) ) ;
#5605 = ORIENTED_EDGE ( 'NONE', *, *, #12415, .F. ) ;
#5606 = CARTESIAN_POINT ( 'NONE',  ( 41.68867513459482410, 159.8737954434936057, 15.00000000000001421 ) ) ;
#5607 = VECTOR ( 'NONE', #14871, 1000.000000000000000 ) ;
#5608 = SURFACE_SIDE_STYLE ('',( #28950 ) ) ;
#5609 = CYLINDRICAL_SURFACE ( 'NONE', #20641, 2.500000000000000000 ) ;
#5610 = CARTESIAN_POINT ( 'NONE',  ( 2.426778023690075337, 214.6231898156240447, 3.398862081921434797 ) ) ;
#5611 = TOROIDAL_SURFACE ( 'NONE', #6690, 6.099999999999999645, 0.4000000000000000222 ) ;
#5612 = CARTESIAN_POINT ( 'NONE',  ( -8.118202686958039038, 201.1607312380087080, 51.20113791807857240 ) ) ;
#5613 = CARTESIAN_POINT ( 'NONE',  ( 87.50000000000002842, 145.7452232778646817, -11.80462230752951136 ) ) ;
#5614 = CARTESIAN_POINT ( 'NONE',  ( 8.062137200540920645, 201.0835637161417822, 29.30113791807857027 ) ) ;
#5615 = CARTESIAN_POINT ( 'NONE',  ( 86.67499999726878457, 141.7447067706911810, 9.630534252274376428 ) ) ;
#5616 = CARTESIAN_POINT ( 'NONE',  ( -0.05014649552828365914, 215.4116977939061144, 93.24886208192143044 ) ) ;
#5617 = CARTESIAN_POINT ( 'NONE',  ( 39.62499999726880162, 171.3844434931184253, -7.942151717890132712E-15 ) ) ;
#5618 = CARTESIAN_POINT ( 'NONE',  ( 36.58867513459482268, 146.1832212156128890, -12.13525491562423042 ) ) ;
#5619 = DIRECTION ( 'NONE',  ( 1.000000000000000000, 0.000000000000000000, 0.000000000000000000 ) ) ;
#5620 = CARTESIAN_POINT ( 'NONE',  ( 9.680171189290831535, 199.9079932115568852, 14.30113791807856849 ) ) ;
#5621 = CARTESIAN_POINT ( 'NONE',  ( 5.088535779737119569, -5.722386535631984295, -7.491772860715834703 ) ) ;
#5622 = CARTESIAN_POINT ( 'NONE',  ( 58.47499999726880304, 149.9369285172503510, 15.58253174999999580 ) ) ;
#5623 = EDGE_CURVE ( 'NONE', #4473, #30739, #9974, .T. ) ;
#5624 = CARTESIAN_POINT ( 'NONE',  ( 3.044812012440130555, 197.4746971517856764, 56.60113791807857098 ) ) ;
#5625 = EDGE_CURVE ( 'NONE', #1291, #31987, #31455, .T. ) ;
#5626 = CARTESIAN_POINT ( 'NONE',  ( 8.118202686958039038, 212.8392687619912635, 28.70113791807856884 ) ) ;
#5627 = CARTESIAN_POINT ( 'NONE',  ( 125.5000000000000000, 80.04668119422662187, 74.95331880577468553 ) ) ;
#5628 = AXIS2_PLACEMENT_3D ( 'NONE', #4176, #19521, #4522 ) ;
#5629 = CARTESIAN_POINT ( 'NONE',  ( -63.50000000000001421, 210.0000000000000000, 0.000000000000000000 ) ) ;
#5630 = CARTESIAN_POINT ( 'NONE',  ( 3.135527875058981895, 197.5041725223112792, 4.598862081921434530 ) ) ;
#5631 = CARTESIAN_POINT ( 'NONE',  ( 58.69999999453762740, 167.3344367211045096, 8.961492836873468093 ) ) ;
#5632 = VERTEX_POINT ( 'NONE', #23085 ) ;
#5633 = CARTESIAN_POINT ( 'NONE',  ( -12.00000000000000711, 207.0476921513413515, 36.50113791807857666 ) ) ;
#5634 = ADVANCED_FACE ( 'NONE', ( #33142 ), #22915, .T. ) ;
#5635 = CARTESIAN_POINT ( 'NONE',  ( -68.50000000000000000, 215.0000000000000000, 0.000000000000000000 ) ) ;
#5636 = CARTESIAN_POINT ( 'NONE',  ( -10.00000000000000711, 206.9523078486584495, 17.49886208192143400 ) ) ;
#5637 = DIRECTION ( 'NONE',  ( 0.000000000000000000, 0.000000000000000000, -1.000000000000000000 ) ) ;
#5638 = VERTEX_POINT ( 'NONE', #15245 ) ;
#5639 = AXIS2_PLACEMENT_3D ( 'NONE', #31026, #25731, #28461 ) ;
#5640 = CARTESIAN_POINT ( 'NONE',  ( -0.05014649552810635652, 196.4853777576173002, 80.75113791807854113 ) ) ;
#5641 = EDGE_CURVE ( 'NONE', #27342, #3282, #12942, .T. ) ;
#5642 = ORIENTED_EDGE ( 'NONE', *, *, #31264, .F. ) ;
#5643 = CIRCLE ( 'NONE', #15449, 2.500000000000000000 ) ;
#5644 = CARTESIAN_POINT ( 'NONE',  ( 65.25000000000000000, 7.347880794884118356E-15, 35.00000000000000000 ) ) ;
#5645 = CARTESIAN_POINT ( 'NONE',  ( 7.940546747334011890, -27.16978800334334565, -17.55088044235630562 ) ) ;
#5646 = VERTEX_POINT ( 'NONE', #4514 ) ;
#5647 = CARTESIAN_POINT ( 'NONE',  ( -4.984841277089726574, 200.2242689037092305, 9.051137918078564937 ) ) ;
#5648 = CARTESIAN_POINT ( 'NONE',  ( -9.736236675708031640, 214.0148392665760753, 101.7988620819214560 ) ) ;
#5649 = CARTESIAN_POINT ( 'NONE',  ( 44.37499999726881583, 155.0000000000000000, 15.58253174999999402 ) ) ;
#5650 = VERTEX_POINT ( 'NONE', #15071 ) ;
#5651 = CARTESIAN_POINT ( 'NONE',  ( 49.62499999726880873, 171.3844434931184253, -7.942151717890132712E-15 ) ) ;
#5652 = DIRECTION ( 'NONE',  ( 1.000000000000000000, 0.000000000000000000, 0.000000000000000000 ) ) ;
#5653 = CARTESIAN_POINT ( 'NONE',  ( -3.044812012440131443, 216.5253028482142952, 7.101137918078566535 ) ) ;
#5654 = AXIS2_PLACEMENT_3D ( 'NONE', #16409, #3467, #751 ) ;
#5655 = CARTESIAN_POINT ( 'NONE',  ( 3.044812012439969795, 216.5253028482143520, 78.39886208192143613 ) ) ;
#5656 = CARTESIAN_POINT ( 'NONE',  ( 51.37499999726881583, 155.0000000000000000, -15.58253175000000823 ) ) ;
#5657 = CARTESIAN_POINT ( 'NONE',  ( -8.062137200540920645, 212.9164362838581894, 21.80113791807856671 ) ) ;
#5658 = CARTESIAN_POINT ( 'NONE',  ( 44.38867513459482694, 140.7341522555726669, -4.635254915624220651 ) ) ;
#5659 = VECTOR ( 'NONE', #2904, 1000.000000000000000 ) ;
#5660 = CARTESIAN_POINT ( 'NONE',  ( 76.20000000000000284, 142.6655632788954620, -8.961492836873480528 ) ) ;
#5661 = CARTESIAN_POINT ( 'NONE',  ( 8.118202686958039038, 212.8392687619912635, 97.70113791807857240 ) ) ;
#5662 = CARTESIAN_POINT ( 'NONE',  ( 89.50000000000002842, 155.0000000000000000, 32.00000000000002842 ) ) ;
#5663 =( BOUNDED_CURVE ( )  B_SPLINE_CURVE ( 2, ( #18418, #2758, #28479, #23528, #16020, #8200, #7535, #13298, #20643, #13461, #12800, #20971, #7699, #17922, #15355, #28970, #31366, #25744, #23691, #18082, #18585, #353, #33586, #5133, #5630, #32186, #29135, #16682, #9020, #24021, #11577, #6470, #32022, #21967, #21794, #8846, #19077, #18909, #29466, #16853, #32355, #5955, #29641, #16344, #19409, #16514, #19246, #6118, #21629, #13623, #6288, #684, #26738, #3400, #27246, #27079, #13796, #18750, #26568, #24190, #3742, #14131, #24525, #11087, #26913, #8686, #852, #8516, #3571, #11244, #1022, #13960, #21467, #3237, #1181, #24355, #29811, #3900, #8360, #14296, #24698, #11417, #1355, #21296, #16179, #31690, #5783, #31851, #29303, #9869, #17020, #32684, #12249, #1860, #27750, #19583, #9352, #4240, #22470, #19748, #30145, #32861, #27414, #9523, #25034, #17189, #4074, #25535, #22637, #1686, #19910, #7324, #12079, #30310, #6977, #6802, #9695, #17364, #4751, #11918, #27574, #30657, #22304, #11743, #4413, #14462, #14799, #7144, #15142, #17700, #25192, #33025, #9193, #17529, #14637, #20087, #22815, #30482, #22130, #20252, #32520, #27917, #4589, #14975, #28088, #25362, #2034, #12421, #33206, #29976, #6634, #24859, #1522, #31325, #7824, #311, #28924, #18212, #2203, #10386, #28769, #15309, #28268, #2374, #23652, #10710, #13094, #33378, #21091, #5584, #25701, #31493, #8160, #10052, #15809, #15648, #5254, #26047, #7991, #31156, #23484, #9740, #33541, #20758, #18542, #26202, #12585, #10554, #12763, #15979, #7489, #15486, #23153, #22978, #20429, #30822, #20599, #17873, #28434, #10217, #13256, #7657, #4923, #31001, #18040, #150, #5091, #18377, #25877, #2543, #2870, #12927, #23322, #28603, #2717, #20933, #5424, #31974, #24144, #24303, #3357, #8803, #13587, #16636, #29424, #6426, #18862, #26868, #29599, #21255, #32141, #29260, #13416, #19035, #24480, #31648, #23980, #3525, #16468, #8644, #483, #8315, #21579, #5911, #26528, #1142, #13748, #18709, #810, #16306, #31808, #29095, #26371, #13918, #26695, #11200, #21917, #6073, #974, #11373, #641, #21752, #29760, #11039, #19200, #6249, #11535, #3199, #3031, #27032, #5743, #3696, #14086, #23811, #32313, #8979, #19366, #10880, #16135, #21422, #8473, #1811, #1986, #17147, #3859, #32982, #12207, #22423, #14932, #9829, #32813, #7102, #17320, #4371, #14595, #14423, #24992, #12376, #17482, #27203, #25146, #11875, #4542, #12035, #27710, #1643, #27533, #9144, #14753, #29934, #22260, #32647, #22773, #22594, #9309, #14252, #22090, #1479, #9646, #24651, #20043, #6588, #9479, #4195, #19702, #4034, #19869, #30095, #30265, #6927, #19541, #32475, #30442, #27868, #25320, #33165, #1317, #20209, #30610, #16807, #11705, #16971, #27367, #24816, #6762, #28044, #33672, #5385, #12545, #28223, #7781, #31118, #23276, #15095, #4880, #33498, #18001, #15268, #25660, #13215, #15770, #28392, #20550, #12716, #22936, #21051, #18171, #30957, #5050, #2830, #7617, #15441, #25837, #2329, #5214, #2499, #277, #7441, #23110, #26163, #7950, #7274, #10347, #33332, #12883, #2675, #10672, #23612, #20718, #28566, #4706, #13055, #10170, #15600, #18333, #26003, #17657, #25491, #2162, #20387, #10003, #23445, #30780, #20891, #110, #10512, #31289, #28726, #17821, #31934, #18503, #16599, #24264, #11332, #8604, #10999, #32107, #19160, #31452, #13704, #26826, #29557, #2997, #18665, #19001, #21544, #24104, #5543, #29055, #23941, #8439, #5708, #16096, #3655, #6210, #771, #18826, #16429, #15934, #26994, #8770, #21379, #29220, #14049, #31772, #5872, #16271, #26491, #29391, #26657, #24445, #31610, #3159, #1109, #11502, #6038, #13376, #440, #11168, #3320, #8121, #28888, #3489, #13881, #26331, #934, #13549, #21717, #23774, #603, #10843, #21216, #8278, #1277, #14218, #22054, #9610, #20006, #32775, #19331, #30406, #7067, #22221, #8941, #4336, #17281, #27500, #17449, #14893, #4157, #12173, #22386, #9447, #19668, #19501, #30060, #27832, #22564, #32275, #30233, #11671, #4502, #17116, #19837, #6726, #32611, #24616, #6890, #32438, #16936, #27332, #25285, #27668, #3997, #29722, #27171, #6553, #14719, #6384, #25111, #1951, #32949, #21880, #9274, #14554, #16772, #1441, #24952, #1610, #12000, #1772, #3826, #9105, #29900, #11836, #14393, #24785, #12340, #28357, #7744, #26132, #17621, #33294, #12845, #2464, #5011, #20172, #9961, #4843, #23070, #20348, #30745, #18294, #20851, #15402, #33462, #31085, #30570, #10474, #13019, #7404, #10133, #7914, #25622, #2290, #20515, #17787, #10311, #12675, #5345, #12512, #28186, #31250, #23411, #33633, #28008, #15059, #25800, #17967, #28686, #30918, #7581, #23238, #9790, #18130, #15234, #20687, #74, #28529, #15734, #22736, #33123, #25454, #4674, #22901, #7233, #2128, #5178, #15563, #25960, #2635, #18627, #23578, #13667, #26619, #23903, #8569, #26782, #568, #11136, #8407, #18793, #16065, #2965, #26454, #29354, #21511, #13180, #5835, #5507, #16390, #13509, #31735, #3120, #29018, #18466, #29182, #28852, #400, #10803, #6002, #16230, #21177, #246, #31413, #23734, #3283, #10637, #24064, #31897, #15896, #5675, #31574, #26293, #10963, #8239, #21338, #735, #13343, #8082, #18961, #3449, #13845, #2799, #21014, #18404, #26077, #17906, #7352, #25733, #23010, #7855, #4953, #30689, #4780, #28300, #10414, #17732, #28628, #20958, #2232, #23513, #28797, #10252, #25901, #15839, #12790, #20627, #5120, #31029, #31186, #28464, #2747, #18, #20283, #5453, #13120, #181, #20787, #23180, #10580 ),
 .UNSPECIFIED., .F., .T. ) 
 B_SPLINE_CURVE_WITH_KNOTS ( ( 3, 2, 2, 2, 2, 2, 2, 2, 2, 2, 2, 2, 2, 2, 2, 2, 2, 2, 2, 2, 2, 2, 2, 2, 2, 2, 2, 2, 2, 2, 2, 2, 2, 2, 2, 2, 2, 2, 2, 2, 2, 2, 2, 2, 2, 2, 2, 2, 2, 2, 2, 2, 2, 2, 2, 2, 2, 2, 2, 2, 2, 2, 2, 2, 2, 2, 2, 2, 2, 2, 2, 2, 2, 2, 2, 2, 2, 2, 2, 2, 2, 2, 2, 2, 2, 2, 2, 2, 2, 2, 2, 2, 2, 2, 2, 2, 2, 2, 2, 2, 2, 2, 2, 2, 2, 2, 2, 2, 2, 2, 2, 2, 2, 2, 2, 2, 2, 2, 2, 2, 2, 2, 2, 2, 2, 2, 2, 2, 2, 2, 2, 2, 2, 2, 2, 2, 2, 2, 2, 2, 2, 2, 2, 2, 2, 2, 2, 2, 2, 2, 2, 2, 2, 2, 2, 2, 2, 2, 2, 2, 2, 2, 2, 2, 2, 2, 2, 2, 2, 2, 2, 2, 2, 2, 2, 2, 2, 2, 2, 2, 2, 2, 2, 2, 2, 2, 2, 2, 2, 2, 2, 2, 2, 2, 2, 2, 2, 2, 2, 2, 2, 2, 2, 2, 2, 2, 2, 2, 2, 2, 2, 2, 2, 2, 2, 2, 2, 2, 2, 2, 2, 2, 2, 2, 2, 2, 2, 2, 2, 2, 2, 2, 2, 2, 2, 2, 2, 2, 2, 2, 2, 2, 2, 2, 2, 2, 2, 2, 2, 2, 2, 2, 2, 2, 2, 2, 2, 2, 2, 2, 2, 2, 2, 2, 2, 2, 2, 2, 2, 2, 2, 2, 2, 2, 2, 2, 2, 2, 2, 2, 2, 2, 2, 2, 2, 2, 2, 2, 2, 2, 2, 2, 2, 2, 2, 2, 2, 2, 2, 2, 2, 2, 2, 2, 2, 2, 2, 2, 2, 2, 2, 2, 2, 2, 2, 2, 2, 2, 2, 2, 2, 2, 2, 2, 2, 2, 2, 2, 2, 2, 2, 2, 2, 2, 2, 2, 2, 2, 2, 2, 2, 2, 2, 2, 2, 3 ),
 ( 0.000000000000000000, 0.002857142857142857140, 0.005714285714285714281, 0.008571428571428571855, 0.01142857142857142856, 0.01428571428571428527, 0.01714285714285714371, 0.02000000000000000042, 0.02285714285714285712, 0.02571428571428571383, 0.02857142857142857054, 0.03142857142857143071, 0.03428571428571428742, 0.03714285714285714413, 0.04000000000000000083, 0.04285714285714285754, 0.04571428571428571425, 0.04857142857142857095, 0.05142857142857142766, 0.05428571428571428437, 0.05714285714285714107, 0.05999999999999999778, 0.06285714285714286143, 0.06571428571428571119, 0.06857142857142857484, 0.07142857142857142461, 0.07428571428571428825, 0.07714285714285713802, 0.08000000000000000167, 0.08285714285714285143, 0.08571428571428571508, 0.08857142857142855097, 0.09142857142857142849, 0.09428571428571429214, 0.09714285714285714191, 0.1000000000000000056, 0.1028571428571428553, 0.1057142857142857190, 0.1085714285714285687, 0.1114285714285714324, 0.1142857142857142821, 0.1171428571428571458, 0.1199999999999999956, 0.1228571428571428592, 0.1257142857142857229, 0.1285714285714285587, 0.1314285714285714224, 0.1342857142857142860, 0.1371428571428571497, 0.1400000000000000133, 0.1428571428571428492, 0.1457142857142857129, 0.1485714285714285765, 0.1514285714285714401, 0.1542857142857142760, 0.1571428571428571397, 0.1600000000000000033, 0.1628571428571428670, 0.1657142857142857029, 0.1685714285714285665, 0.1714285714285714302, 0.1742857142857142938, 0.1771428571428571019, 0.1799999999999999933, 0.1828571428571428570, 0.1857142857142857206, 0.1885714285714285843, 0.1914285714285714202, 0.1942857142857142838, 0.1971428571428571475, 0.2000000000000000111, 0.2028571428571428470, 0.2057142857142857106, 0.2085714285714285743, 0.2114285714285714379, 0.2142857142857142738, 0.2171428571428571375, 0.2200000000000000011, 0.2228571428571428648, 0.2257142857142857006, 0.2285714285714285643, 0.2314285714285714279, 0.2342857142857142916, 0.2371428571428571552, 0.2399999999999999911, 0.2428571428571428548, 0.2457142857142857184, 0.2485714285714285821, 0.2514285714285714457, 0.2542857142857142816, 0.2571428571428571175, 0.2600000000000000089, 0.2628571428571428448, 0.2657142857142857362, 0.2685714285714285721, 0.2714285714285714080, 0.2742857142857142994, 0.2771428571428571352, 0.2800000000000000266, 0.2828571428571428625, 0.2857142857142856984, 0.2885714285714285898, 0.2914285714285714257, 0.2942857142857142616, 0.2971428571428571530, 0.2999999999999999889, 0.3028571428571428803, 0.3057142857142857162, 0.3085714285714285521, 0.3114285714285714435, 0.3142857142857142794, 0.3171428571428571153, 0.3200000000000000067, 0.3228571428571428426, 0.3257142857142857340, 0.3285714285714285698, 0.3314285714285714057, 0.3342857142857142971, 0.3371428571428571330, 0.3400000000000000244, 0.3428571428571428603, 0.3457142857142856962, 0.3485714285714285876, 0.3514285714285714235, 0.3542857142857142039, 0.3571428571428571508, 0.3599999999999999867, 0.3628571428571428781, 0.3657142857142857140, 0.3685714285714285499, 0.3714285714285714413, 0.3742857142857142771, 0.3771428571428571686, 0.3800000000000000044, 0.3828571428571428403, 0.3857142857142857317, 0.3885714285714285676, 0.3914285714285714035, 0.3942857142857142949, 0.3971428571428571308, 0.4000000000000000222, 0.4028571428571428581, 0.4057142857142856940, 0.4085714285714285854, 0.4114285714285714213, 0.4142857142857143127, 0.4171428571428571486, 0.4199999999999999845, 0.4228571428571428759, 0.4257142857142857117, 0.4285714285714285476, 0.4314285714285714390, 0.4342857142857142749, 0.4371428571428571663, 0.4400000000000000022, 0.4428571428571428381, 0.4457142857142857295, 0.4485714285714285654, 0.4514285714285714013, 0.4542857142857142927, 0.4571428571428571286, 0.4600000000000000200, 0.4628571428571428559, 0.4657142857142856918, 0.4685714285714285832, 0.4714285714285714191, 0.4742857142857143105, 0.4771428571428571463, 0.4799999999999999822, 0.4828571428571428736, 0.4857142857142857095, 0.4885714285714285454, 0.4914285714285714368, 0.4942857142857142727, 0.4971428571428571641, 0.5000000000000000000, 0.5028571428571428914, 0.5057142857142856718, 0.5085714285714285632, 0.5114285714285714546, 0.5142857142857142350, 0.5171428571428571264, 0.5200000000000000178, 0.5228571428571429092, 0.5257142857142856895, 0.5285714285714285809, 0.5314285714285714723, 0.5342857142857142527, 0.5371428571428571441, 0.5400000000000000355, 0.5428571428571428159, 0.5457142857142857073, 0.5485714285714285987, 0.5514285714285713791, 0.5542857142857142705, 0.5571428571428571619, 0.5600000000000000533, 0.5628571428571428337, 0.5657142857142857251, 0.5685714285714286165, 0.5714285714285713969, 0.5742857142857142883, 0.5771428571428571797, 0.5799999999999999600, 0.5828571428571428514, 0.5857142857142857428, 0.5885714285714285232, 0.5914285714285714146, 0.5942857142857143060, 0.5971428571428571974, 0.5999999999999999778, 0.6028571428571428692, 0.6057142857142857606, 0.6085714285714285410, 0.6114285714285714324, 0.6142857142857143238, 0.6171428571428571042, 0.6199999999999999956, 0.6228571428571428870, 0.6257142857142856673, 0.6285714285714285587, 0.6314285714285714501, 0.6342857142857142305, 0.6371428571428571219, 0.6400000000000000133, 0.6428571428571429047, 0.6457142857142856851, 0.6485714285714285765, 0.6514285714285714679, 0.6542857142857142483, 0.6571428571428571397, 0.6600000000000000311, 0.6628571428571428115, 0.6657142857142857029, 0.6685714285714285943, 0.6714285714285713746, 0.6742857142857142660, 0.6771428571428571574, 0.6800000000000000488, 0.6828571428571428292, 0.6857142857142857206, 0.6885714285714286120, 0.6914285714285713924, 0.6942857142857142838, 0.6971428571428571752, 0.7000000000000000666, 0.7028571428571428470, 0.7057142857142857384, 0.7085714285714284077, 0.7114285714285714102, 0.7142857142857143016, 0.7171428571428571930, 0.7199999999999999734, 0.7228571428571428648, 0.7257142857142857562, 0.7285714285714285365, 0.7314285714285714279, 0.7342857142857143193, 0.7371428571428570997, 0.7399999999999999911, 0.7428571428571428825, 0.7457142857142856629, 0.7485714285714285543, 0.7514285714285714457, 0.7542857142857143371, 0.7571428571428571175, 0.7600000000000000089, 0.7628571428571429003, 0.7657142857142856807, 0.7685714285714285721, 0.7714285714285714635, 0.7742857142857142438, 0.7771428571428571352, 0.7800000000000000266, 0.7828571428571428070, 0.7857142857142856984, 0.7885714285714285898, 0.7914285714285714812, 0.7942857142857142616, 0.7971428571428571530, 0.8000000000000000444, 0.8028571428571428248, 0.8057142857142857162, 0.8085714285714286076, 0.8114285714285713880, 0.8142857142857142794, 0.8171428571428571708, 0.8199999999999999512, 0.8228571428571428426, 0.8257142857142857340, 0.8285714285714286254, 0.8314285714285714057, 0.8342857142857142971, 0.8371428571428571885, 0.8399999999999999689, 0.8428571428571428603, 0.8457142857142857517, 0.8485714285714285321, 0.8514285714285714235, 0.8542857142857143149, 0.8571428571428570953, 0.8599999999999999867, 0.8628571428571428781, 0.8657142857142857695, 0.8685714285714285499, 0.8714285714285714413, 0.8742857142857143327, 0.8771428571428571130, 0.8800000000000000044, 0.8828571428571428958, 0.8857142857142856762, 0.8885714285714285676, 0.8914285714285714590, 0.8942857142857142394, 0.8971428571428571308, 0.8999999999999999112, 0.9028571428571428026, 0.9057142857142856940, 0.9085714285714285854, 0.9114285714285714768, 0.9142857142857142572, 0.9171428571428571486, 0.9200000000000000400, 0.9228571428571428203, 0.9257142857142857117, 0.9285714285714286031, 0.9314285714285713835, 0.9342857142857142749, 0.9371428571428571663, 0.9399999999999999467, 0.9428571428571428381, 0.9457142857142857295, 0.9485714285714286209, 0.9514285714285714013, 0.9542857142857142927, 0.9571428571428571841, 0.9599999999999999645, 0.9628571428571428559, 0.9657142857142857473, 0.9685714285714285277, 0.9714285714285714191, 0.9742857142857143105, 0.9771428571428570908, 0.9799999999999999822, 0.9828571428571428736, 0.9852555582871577178 ),
 .UNSPECIFIED. ) 
 CURVE ( )  GEOMETRIC_REPRESENTATION_ITEM ( )  RATIONAL_B_SPLINE_CURVE ( ( 1.000000000000000000, 0.9510565162951535312, 1.000000000000000000, 0.9510565162951535312, 1.000000000000000000, 0.9510565162951535312, 1.000000000000000000, 0.9510565162951535312, 1.000000000000000000, 0.9510565162951535312, 1.000000000000000000, 0.9510565162951535312, 1.000000000000000000, 0.9510565162951535312, 1.000000000000000000, 0.9510565162951535312, 1.000000000000000000, 0.9510565162951535312, 1.000000000000000000, 0.9510565162951535312, 1.000000000000000000, 0.9510565162951535312, 1.000000000000000000, 0.9510565162951535312, 1.000000000000000000, 0.9510565162951535312, 1.000000000000000000, 0.9510565162951535312, 1.000000000000000000, 0.9510565162951535312, 1.000000000000000000, 0.9510565162951535312, 1.000000000000000000, 0.9510565162951535312, 1.000000000000000000, 0.9510565162951535312, 1.000000000000000000, 0.9510565162951535312, 1.000000000000000000, 0.9510565162951535312, 1.000000000000000000, 0.9510565162951535312, 1.000000000000000000, 0.9510565162951535312, 1.000000000000000000, 0.9510565162951535312, 1.000000000000000000, 0.9510565162951535312, 1.000000000000000000, 0.9510565162951535312, 1.000000000000000000, 0.9510565162951535312, 1.000000000000000000, 0.9510565162951535312, 1.000000000000000000, 0.9510565162951535312, 1.000000000000000000, 0.9510565162951535312, 1.000000000000000000, 0.9510565162951535312, 1.000000000000000000, 0.9510565162951535312, 1.000000000000000000, 0.9510565162951535312, 1.000000000000000000, 0.9510565162951535312, 1.000000000000000000, 0.9510565162951535312, 1.000000000000000000, 0.9510565162951535312, 1.000000000000000000, 0.9510565162951535312, 1.000000000000000000, 0.9510565162951535312, 1.000000000000000000, 0.9510565162951535312, 1.000000000000000000, 0.9510565162951535312, 1.000000000000000000, 0.9510565162951535312, 1.000000000000000000, 0.9510565162951535312, 1.000000000000000000, 0.9510565162951535312, 1.000000000000000000, 0.9510565162951535312, 1.000000000000000000, 0.9510565162951535312, 1.000000000000000000, 0.9510565162951535312, 1.000000000000000000, 0.9510565162951535312, 1.000000000000000000, 0.9510565162951535312, 1.000000000000000000, 0.9510565162951535312, 1.000000000000000000, 0.9510565162951535312, 1.000000000000000000, 0.9510565162951535312, 1.000000000000000000, 0.9510565162951535312, 1.000000000000000000, 0.9510565162951535312, 1.000000000000000000, 0.9510565162951535312, 1.000000000000000000, 0.9510565162951535312, 1.000000000000000000, 0.9510565162951535312, 1.000000000000000000, 0.9510565162951535312, 1.000000000000000000, 0.9510565162951535312, 1.000000000000000000, 0.9510565162951535312, 1.000000000000000000, 0.9510565162951535312, 1.000000000000000000, 0.9510565162951535312, 1.000000000000000000, 0.9510565162951535312, 1.000000000000000000, 0.9510565162951535312, 1.000000000000000000, 0.9510565162951535312, 1.000000000000000000, 0.9510565162951535312, 1.000000000000000000, 0.9510565162951535312, 1.000000000000000000, 0.9510565162951535312, 1.000000000000000000, 0.9510565162951535312, 1.000000000000000000, 0.9510565162951535312, 1.000000000000000000, 0.9510565162951535312, 1.000000000000000000, 0.9510565162951535312, 1.000000000000000000, 0.9510565162951535312, 1.000000000000000000, 0.9510565162951535312, 1.000000000000000000, 0.9510565162951535312, 1.000000000000000000, 0.9510565162951535312, 1.000000000000000000, 0.9510565162951535312, 1.000000000000000000, 0.9510565162951535312, 1.000000000000000000, 0.9510565162951535312, 1.000000000000000000, 0.9510565162951535312, 1.000000000000000000, 0.9510565162951535312, 1.000000000000000000, 0.9510565162951535312, 1.000000000000000000, 0.9510565162951535312, 1.000000000000000000, 0.9510565162951535312, 1.000000000000000000, 0.9510565162951535312, 1.000000000000000000, 0.9510565162951535312, 1.000000000000000000, 0.9510565162951535312, 1.000000000000000000, 0.9510565162951535312, 1.000000000000000000, 0.9510565162951535312, 1.000000000000000000, 0.9510565162951535312, 1.000000000000000000, 0.9510565162951535312, 1.000000000000000000, 0.9510565162951535312, 1.000000000000000000, 0.9510565162951535312, 1.000000000000000000, 0.9510565162951535312, 1.000000000000000000, 0.9510565162951535312, 1.000000000000000000, 0.9510565162951535312, 1.000000000000000000, 0.9510565162951535312, 1.000000000000000000, 0.9510565162951535312, 1.000000000000000000, 0.9510565162951535312, 1.000000000000000000, 0.9510565162951535312, 1.000000000000000000, 0.9510565162951535312, 1.000000000000000000, 0.9510565162951535312, 1.000000000000000000, 0.9510565162951535312, 1.000000000000000000, 0.9510565162951535312, 1.000000000000000000, 0.9510565162951535312, 1.000000000000000000, 0.9510565162951535312, 1.000000000000000000, 0.9510565162951535312, 1.000000000000000000, 0.9510565162951535312, 1.000000000000000000, 0.9510565162951535312, 1.000000000000000000, 0.9510565162951535312, 1.000000000000000000, 0.9510565162951535312, 1.000000000000000000, 0.9510565162951535312, 1.000000000000000000, 0.9510565162951535312, 1.000000000000000000, 0.9510565162951535312, 1.000000000000000000, 0.9510565162951535312, 1.000000000000000000, 0.9510565162951535312, 1.000000000000000000, 0.9510565162951535312, 1.000000000000000000, 0.9510565162951535312, 1.000000000000000000, 0.9510565162951535312, 1.000000000000000000, 0.9510565162951535312, 1.000000000000000000, 0.9510565162951535312, 1.000000000000000000, 0.9510565162951535312, 1.000000000000000000, 0.9510565162951535312, 1.000000000000000000, 0.9510565162951535312, 1.000000000000000000, 0.9510565162951535312, 1.000000000000000000, 0.9510565162951535312, 1.000000000000000000, 0.9510565162951535312, 1.000000000000000000, 0.9510565162951535312, 1.000000000000000000, 0.9510565162951535312, 1.000000000000000000, 0.9510565162951535312, 1.000000000000000000, 0.9510565162951535312, 1.000000000000000000, 0.9510565162951535312, 1.000000000000000000, 0.9510565162951535312, 1.000000000000000000, 0.9510565162951535312, 1.000000000000000000, 0.9510565162951535312, 1.000000000000000000, 0.9510565162951535312, 1.000000000000000000, 0.9510565162951535312, 1.000000000000000000, 0.9510565162951535312, 1.000000000000000000, 0.9510565162951535312, 1.000000000000000000, 0.9510565162951535312, 1.000000000000000000, 0.9510565162951535312, 1.000000000000000000, 0.9510565162951535312, 1.000000000000000000, 0.9510565162951535312, 1.000000000000000000, 0.9510565162951535312, 1.000000000000000000, 0.9510565162951535312, 1.000000000000000000, 0.9510565162951535312, 1.000000000000000000, 0.9510565162951535312, 1.000000000000000000, 0.9510565162951535312, 1.000000000000000000, 0.9510565162951535312, 1.000000000000000000, 0.9510565162951535312, 1.000000000000000000, 0.9510565162951535312, 1.000000000000000000, 0.9510565162951535312, 1.000000000000000000, 0.9510565162951535312, 1.000000000000000000, 0.9510565162951535312, 1.000000000000000000, 0.9510565162951535312, 1.000000000000000000, 0.9510565162951535312, 1.000000000000000000, 0.9510565162951535312, 1.000000000000000000, 0.9510565162951535312, 1.000000000000000000, 0.9510565162951535312, 1.000000000000000000, 0.9510565162951535312, 1.000000000000000000, 0.9510565162951535312, 1.000000000000000000, 0.9510565162951535312, 1.000000000000000000, 0.9510565162951535312, 1.000000000000000000, 0.9510565162951535312, 1.000000000000000000, 0.9510565162951535312, 1.000000000000000000, 0.9510565162951535312, 1.000000000000000000, 0.9510565162951535312, 1.000000000000000000, 0.9510565162951535312, 1.000000000000000000, 0.9510565162951535312, 1.000000000000000000, 0.9510565162951535312, 1.000000000000000000, 0.9510565162951535312, 1.000000000000000000, 0.9510565162951535312, 1.000000000000000000, 0.9510565162951535312, 1.000000000000000000, 0.9510565162951535312, 1.000000000000000000, 0.9510565162951535312, 1.000000000000000000, 0.9510565162951535312, 1.000000000000000000, 0.9510565162951535312, 1.000000000000000000, 0.9510565162951535312, 1.000000000000000000, 0.9510565162951535312, 1.000000000000000000, 0.9510565162951535312, 1.000000000000000000, 0.9510565162951535312, 1.000000000000000000, 0.9510565162951535312, 1.000000000000000000, 0.9510565162951535312, 1.000000000000000000, 0.9510565162951535312, 1.000000000000000000, 0.9510565162951535312, 1.000000000000000000, 0.9510565162951535312, 1.000000000000000000, 0.9510565162951535312, 1.000000000000000000, 0.9510565162951535312, 1.000000000000000000, 0.9510565162951535312, 1.000000000000000000, 0.9510565162951535312, 1.000000000000000000, 0.9510565162951535312, 1.000000000000000000, 0.9510565162951535312, 1.000000000000000000, 0.9510565162951535312, 1.000000000000000000, 0.9510565162951535312, 1.000000000000000000, 0.9510565162951535312, 1.000000000000000000, 0.9510565162951535312, 1.000000000000000000, 0.9510565162951535312, 1.000000000000000000, 0.9510565162951535312, 1.000000000000000000, 0.9510565162951535312, 1.000000000000000000, 0.9510565162951535312, 1.000000000000000000, 0.9510565162951535312, 1.000000000000000000, 0.9510565162951535312, 1.000000000000000000, 0.9510565162951535312, 1.000000000000000000, 0.9510565162951535312, 1.000000000000000000, 0.9510565162951535312, 1.000000000000000000, 0.9510565162951535312, 1.000000000000000000, 0.9510565162951535312, 1.000000000000000000, 0.9510565162951535312, 1.000000000000000000, 0.9510565162951535312, 1.000000000000000000, 0.9510565162951535312, 1.000000000000000000, 0.9510565162951535312, 1.000000000000000000, 0.9510565162951535312, 1.000000000000000000, 0.9510565162951535312, 1.000000000000000000, 0.9510565162951535312, 1.000000000000000000, 0.9510565162951535312, 1.000000000000000000, 0.9510565162951535312, 1.000000000000000000, 0.9510565162951535312, 1.000000000000000000, 0.9510565162951535312, 1.000000000000000000, 0.9510565162951535312, 1.000000000000000000, 0.9510565162951535312, 1.000000000000000000, 0.9510565162951535312, 1.000000000000000000, 0.9510565162951535312, 1.000000000000000000, 0.9510565162951535312, 1.000000000000000000, 0.9510565162951535312, 1.000000000000000000, 0.9510565162951535312, 1.000000000000000000, 0.9510565162951535312, 1.000000000000000000, 0.9510565162951535312, 1.000000000000000000, 0.9510565162951535312, 1.000000000000000000, 0.9510565162951535312, 1.000000000000000000, 0.9510565162951535312, 1.000000000000000000, 0.9510565162951535312, 1.000000000000000000, 0.9510565162951535312, 1.000000000000000000, 0.9510565162951535312, 1.000000000000000000, 0.9510565162951535312, 1.000000000000000000, 0.9510565162951535312, 1.000000000000000000, 0.9510565162951535312, 1.000000000000000000, 0.9510565162951535312, 1.000000000000000000, 0.9510565162951535312, 1.000000000000000000, 0.9510565162951535312, 1.000000000000000000, 0.9510565162951535312, 1.000000000000000000, 0.9510565162951535312, 1.000000000000000000, 0.9510565162951535312, 1.000000000000000000, 0.9510565162951535312, 1.000000000000000000, 0.9510565162951535312, 1.000000000000000000, 0.9510565162951535312, 1.000000000000000000, 0.9510565162951535312, 1.000000000000000000, 0.9510565162951535312, 1.000000000000000000, 0.9510565162951535312, 1.000000000000000000, 0.9510565162951535312, 1.000000000000000000, 0.9510565162951535312, 1.000000000000000000, 0.9510565162951535312, 1.000000000000000000, 0.9510565162951535312, 1.000000000000000000, 0.9510565162951535312, 1.000000000000000000, 0.9510565162951535312, 1.000000000000000000, 0.9510565162951535312, 1.000000000000000000, 0.9510565162951535312, 1.000000000000000000, 0.9510565162951535312, 1.000000000000000000, 0.9510565162951535312, 1.000000000000000000, 0.9510565162951535312, 1.000000000000000000, 0.9510565162951535312, 1.000000000000000000, 0.9510565162951535312, 1.000000000000000000, 0.9510565162951535312, 1.000000000000000000, 0.9510565162951535312, 1.000000000000000000, 0.9510565162951535312, 1.000000000000000000, 0.9510565162951535312, 1.000000000000000000, 0.9510565162951535312, 1.000000000000000000, 0.9510565162951535312, 1.000000000000000000, 0.9510565162951535312, 1.000000000000000000, 0.9510565162951535312, 1.000000000000000000, 0.9510565162951535312, 1.000000000000000000, 0.9510565162951535312, 1.000000000000000000, 0.9510565162951535312, 1.000000000000000000, 0.9510565162951535312, 1.000000000000000000, 0.9510565162951535312, 1.000000000000000000, 0.9510565162951535312, 1.000000000000000000, 0.9510565162951535312, 1.000000000000000000, 0.9510565162951535312, 1.000000000000000000, 0.9510565162951535312, 1.000000000000000000, 0.9510565162951535312, 1.000000000000000000, 0.9510565162951535312, 1.000000000000000000, 0.9510565162951535312, 1.000000000000000000, 0.9510565162951535312, 1.000000000000000000, 0.9510565162951535312, 1.000000000000000000, 0.9510565162951535312, 1.000000000000000000, 0.9510565162951535312, 1.000000000000000000, 0.9510565162951535312, 1.000000000000000000, 0.9510565162951535312, 1.000000000000000000, 0.9510565162951535312, 1.000000000000000000, 0.9510565162951535312, 1.000000000000000000, 0.9510565162951535312, 1.000000000000000000, 0.9510565162951535312, 1.000000000000000000, 0.9510565162951535312, 1.000000000000000000, 0.9510565162951535312, 1.000000000000000000, 0.9510565162951535312, 1.000000000000000000, 0.9510565162951535312, 1.000000000000000000, 0.9510565162951535312, 1.000000000000000000, 0.9510565162951535312, 1.000000000000000000, 0.9510565162951535312, 1.000000000000000000, 0.9510565162951535312, 1.000000000000000000, 0.9510565162951535312, 1.000000000000000000, 0.9510565162951535312, 1.000000000000000000, 0.9510565162951535312, 1.000000000000000000, 0.9510565162951535312, 1.000000000000000000, 0.9510565162951535312, 1.000000000000000000, 0.9510565162951535312, 1.000000000000000000, 0.9510565162951535312, 1.000000000000000000, 0.9510565162951535312, 1.000000000000000000, 0.9510565162951535312, 1.000000000000000000, 0.9510565162951535312, 1.000000000000000000, 0.9510565162951535312, 1.000000000000000000, 0.9510565162951535312, 1.000000000000000000, 0.9510565162951535312, 1.000000000000000000, 0.9510565162951535312, 1.000000000000000000, 0.9510565162951535312, 1.000000000000000000, 0.9510565162951535312, 1.000000000000000000, 0.9510565162951535312, 1.000000000000000000, 0.9510565162951535312, 1.000000000000000000, 0.9510565162951535312, 1.000000000000000000, 0.9510565162951535312, 1.000000000000000000, 0.9510565162951535312, 1.000000000000000000, 0.9510565162951535312, 1.000000000000000000, 0.9510565162951535312, 1.000000000000000000, 0.9510565162951535312, 1.000000000000000000, 0.9510565162951535312, 1.000000000000000000, 0.9510565162951535312, 1.000000000000000000, 0.9510565162951535312, 1.000000000000000000, 0.9510565162951535312, 1.000000000000000000, 0.9510565162951535312, 1.000000000000000000, 0.9510565162951535312, 1.000000000000000000, 0.9510565162951535312, 1.000000000000000000, 0.9510565162951535312, 1.000000000000000000, 0.9510565162951535312, 1.000000000000000000, 0.9510565162951535312, 1.000000000000000000, 0.9510565162951535312, 1.000000000000000000, 0.9510565162951535312, 1.000000000000000000, 0.9510565162951535312, 1.000000000000000000, 0.9510565162951535312, 1.000000000000000000, 0.9510565162951535312, 1.000000000000000000, 0.9510565162951535312, 1.000000000000000000, 0.9510565162951535312, 1.000000000000000000, 0.9510565162951535312, 1.000000000000000000, 0.9510565162951535312, 1.000000000000000000, 0.9510565162951535312, 1.000000000000000000, 0.9510565162951535312, 1.000000000000000000, 0.9510565162951535312, 1.000000000000000000, 0.9510565162951535312, 1.000000000000000000, 0.9589146177192661158, 0.9868071058056508971 ) ) 
 REPRESENTATION_ITEM ( '' )  );
#5664 = CARTESIAN_POINT ( 'NONE',  ( 8.062137200540920645, 201.0835637161417822, 86.30113791807856671 ) ) ;
#5665 = DIRECTION ( 'NONE',  ( -0.000000000000000000, -0.000000000000000000, -1.000000000000000000 ) ) ;
#5666 = CARTESIAN_POINT ( 'NONE',  ( 38.07499999726880446, 168.2552932293087906, 9.630534252274372875 ) ) ;
#5667 = CARTESIAN_POINT ( 'NONE',  ( -11.98450388067341876, 203.0532714938636047, 92.34886208192143897 ) ) ;
#5668 = CARTESIAN_POINT ( 'NONE',  ( 75.62499999726881583, 171.3844434931184253, -7.942151717890132712E-15 ) ) ;
#5669 = ORIENTED_EDGE ( 'NONE', *, *, #29910, .T. ) ;
#5670 = DIRECTION ( 'NONE',  ( -1.000000000000000000, -0.000000000000000000, -0.000000000000000000 ) ) ;
#5671 = CARTESIAN_POINT ( 'NONE',  ( 40.09999999453762598, 159.7113355953771077, -14.50000000000000888 ) ) ;
#5672 = CARTESIAN_POINT ( 'NONE',  ( 40.31132485994280756, 169.2658477444273331, 4.635254915624208216 ) ) ;
#5673 = CARTESIAN_POINT ( 'NONE',  ( 0.04725809328185039127, -9.175759667312528123, -8.057670357645362103 ) ) ;
#5674 = ORIENTED_EDGE ( 'NONE', *, *, #2525, .F. ) ;
#5675 = CARTESIAN_POINT ( 'NONE',  ( 10.01549611932659367, 203.7984951890124421, 97.14886208192145034 ) ) ;
#5676 = CARTESIAN_POINT ( 'NONE',  ( 9.736236675708031640, 199.9851607334238963, 34.29886208192143471 ) ) ;
#5677 = CARTESIAN_POINT ( 'NONE',  ( -7.907996613752304782, -3.055722423191990611, -7.792112796859422374 ) ) ;
#5678 = CARTESIAN_POINT ( 'NONE',  ( 0.05014649552810505201, 217.5146222423826714, 43.25113791807856956 ) ) ;
#5679 = VERTEX_POINT ( 'NONE', #23250 ) ;
#5680 = CARTESIAN_POINT ( 'NONE',  ( 4.903702542908435547, 213.8346818373419751, 6.548862081921434708 ) ) ;
#5681 = CARTESIAN_POINT ( 'NONE',  ( 125.5000000000000000, 229.9533188057739039, -74.95331880577418815 ) ) ;
#5682 = AXIS2_PLACEMENT_3D ( 'NONE', #22806, #18204, #33196 ) ;
#5683 = VERTEX_POINT ( 'NONE', #22575 ) ;
#5684 = CARTESIAN_POINT ( 'NONE',  ( 0.05014649552828262524, 198.5883022060938572, 94.74886208192144466 ) ) ;
#5685 = CARTESIAN_POINT ( 'NONE',  ( -6.444103211791042618, 211.7408657792732356, 33.80113791807857382 ) ) ;
#5686 = CARTESIAN_POINT ( 'NONE',  ( 0.000000000000000000, 0.000000000000000000, 2.066666666667000385 ) ) ;
#5687 = ORIENTED_EDGE ( 'NONE', *, *, #25979, .T. ) ;
#5688 = CARTESIAN_POINT ( 'NONE',  ( -0.3483149870578547969, 8.861353789385022495, -7.493854785173811983 ) ) ;
#5689 = CARTESIAN_POINT ( 'NONE',  ( 35.17499999726881299, 145.8408176439707802, -12.60653300113719588 ) ) ;
#5690 = DIRECTION ( 'NONE',  ( 0.000000000000000000, 0.000000000000000000, 1.000000000000000000 ) ) ;
#5691 = CARTESIAN_POINT ( 'NONE',  ( 4.903702542908601636, 200.1653181626581102, 86.45113791807858661 ) ) ;
#5692 = CARTESIAN_POINT ( 'NONE',  ( 0.000000000000000000, 0.000000000000000000, 0.000000000000000000 ) ) ;
#5693 = CARTESIAN_POINT ( 'NONE',  ( 57.40000000000000568, 159.7113355953771077, 14.49999999999999289 ) ) ;
#5694 = CARTESIAN_POINT ( 'NONE',  ( 2.426778023690075337, 214.6231898156240447, 69.39886208192143613 ) ) ;
#5695 = CARTESIAN_POINT ( 'NONE',  ( -125.0000000000000000, -95.00000000000000000, 270.4495957273638282 ) ) ;
#5696 = CARTESIAN_POINT ( 'NONE',  ( 48.62499999726880873, 138.6155565068815463, -3.929120461958505118E-15 ) ) ;
#5698 = ORIENTED_EDGE ( 'NONE', *, *, #6828, .F. ) ;
#5697 = CARTESIAN_POINT ( 'NONE',  ( -8.118202686958039038, 201.1607312380087080, 6.201137918078566180 ) ) ;
#5699 = CARTESIAN_POINT ( 'NONE',  ( 18.00000000000000355, 0.000000000000000000, -18.00000000000000000 ) ) ;
#5700 = CARTESIAN_POINT ( 'NONE',  ( 63.92499999726880588, 164.1591823560292198, 12.60653300113718167 ) ) ;
#5701 = CARTESIAN_POINT ( 'NONE',  ( 78.17499999726881299, 164.1591823560292198, 12.60653300113718167 ) ) ;
#5702 = CARTESIAN_POINT ( 'NONE',  ( 7.375838497908181246, 196.7627149292499666, 77.45113791807855819 ) ) ;
#5703 = LINE ( 'NONE', #16091, #28231 ) ;
#5704 = CARTESIAN_POINT ( 'NONE',  ( 6.220909254589536808, 215.4770327129947987, 97.55113791807856671 ) ) ;
#5705 = CARTESIAN_POINT ( 'NONE',  ( 84.48867513459482836, 142.2402378747194405, -9.270509831248439525 ) ) ;
#5706 = ORIENTED_EDGE ( 'NONE', *, *, #3963, .F. ) ;
#5707 = CARTESIAN_POINT ( 'NONE',  ( 3.753561863808876797, 195.6020594897209719, 61.59886208192143897 ) ) ;
#5708 = CARTESIAN_POINT ( 'NONE',  ( -10.01549611932659545, 210.2015048109875011, 65.64886208192143613 ) ) ;
#5709 = CARTESIAN_POINT ( 'NONE',  ( -3.662846001189865142, 195.5725841191952838, 7.898862081921435241 ) ) ;
#5710 = DIRECTION ( 'NONE',  ( 1.000000000000000000, -0.000000000000000000, -0.000000000000000000 ) ) ;
#5711 = CARTESIAN_POINT ( 'NONE',  ( 6.139770520408368348, 198.4640165459539674, 17.45113791807855819 ) ) ;
#5712 = CARTESIAN_POINT ( 'NONE',  ( 0.05014649552828275708, 196.4853777576173002, 82.74886208192143044 ) ) ;
#5713 = EDGE_CURVE ( 'NONE', #4391, #22743, #16746, .T. ) ;
#5714 = ORIENTED_EDGE ( 'NONE', *, *, #5436, .T. ) ;
#5715 = CARTESIAN_POINT ( 'NONE',  ( 6.139770520408368348, 198.4640165459539674, 101.4511379180785866 ) ) ;
#5716 = ORIENTED_EDGE ( 'NONE', *, *, #15535, .T. ) ;
#5717 = SURFACE_STYLE_USAGE ( .BOTH. , #452 ) ;
#5718 = CARTESIAN_POINT ( 'NONE',  ( 4.984841277089891776, 200.2242689037093726, 64.44886208192143329 ) ) ;
#5719 = ORIENTED_EDGE ( 'NONE', *, *, #3737, .F. ) ;
#5720 = CARTESIAN_POINT ( 'NONE',  ( 76.92499999726881299, 145.8408176439707802, -12.60653300113719588 ) ) ;
#5721 = DIRECTION ( 'NONE',  ( 0.000000000000000000, 0.000000000000000000, -1.000000000000000000 ) ) ;
#5722 = CARTESIAN_POINT ( 'NONE',  ( 0.000000000000000000, 0.000000000000000000, 9.480888224575629408 ) ) ;
#5723 = CARTESIAN_POINT ( 'NONE',  ( 71.32499999726881867, 164.1591823560292198, -12.60653300113719766 ) ) ;
#5724 = CARTESIAN_POINT ( 'NONE',  ( -6.444103211791042618, 211.7408657792732356, 63.80113791807858092 ) ) ;
#5725 =( NAMED_UNIT ( * ) PLANE_ANGLE_UNIT ( ) SI_UNIT ( $, .RADIAN. ) );
#5726 = DIRECTION ( 'NONE',  ( -0.9945218953682717355, 1.280104479605409178E-17, -0.1045284632676676817 ) ) ;
#5727 = PRESENTATION_STYLE_ASSIGNMENT (( #29243 ) ) ;
#5728 = LINE ( 'NONE', #23795, #8523 ) ;
#5729 = CARTESIAN_POINT ( 'NONE',  ( 6.500168698208244500, 202.3363017425938324, 40.29886208192144181 ) ) ;
#5730 = CARTESIAN_POINT ( 'NONE',  ( 8.062137200540920645, 201.0835637161417822, 77.30113791807858092 ) ) ;
#5731 = CARTESIAN_POINT ( 'NONE',  ( 63.48867513459483547, 167.7597621252805880, 9.270509831248428867 ) ) ;
#5732 = CARTESIAN_POINT ( 'NONE',  ( 6.139770520408368348, 198.4640165459539674, 62.45113791807857950 ) ) ;
#5733 = DIRECTION ( 'NONE',  ( 1.000000000000000000, -0.000000000000000000, -0.000000000000000000 ) ) ;
#5734 = CARTESIAN_POINT ( 'NONE',  ( 4.903702542908601636, 200.1653181626581102, 17.45113791807856174 ) ) ;
#5735 = CARTESIAN_POINT ( 'NONE',  ( -5.357619327558936585E-16, 7.505553499465137612, -8.000000000000000000 ) ) ;
#5736 = CARTESIAN_POINT ( 'NONE',  ( 6.500000000000000000, -3.752776749732574135, -6.064240316920400886 ) ) ;
#5737 = CARTESIAN_POINT ( 'NONE',  ( 43.72499999726881015, 169.8198683612136222, 4.815267126137181997 ) ) ;
#5738 = CARTESIAN_POINT ( 'NONE',  ( 3.753561863808689836, 218.3979405102790565, 46.40113791807856813 ) ) ;
#5739 = DIRECTION ( 'NONE',  ( -0.1461455375466716444, 0.9854922318508084755, -0.08629335326029916042 ) ) ;
#5740 = CARTESIAN_POINT ( 'NONE',  ( 10.01549611932653860, 210.2015048109876716, 91.85113791807853545 ) ) ;
#5741 = CARTESIAN_POINT ( 'NONE',  ( 8.062137200540920645, 201.0835637161417822, 68.30113791807856671 ) ) ;
#5742 = CARTESIAN_POINT ( 'NONE',  ( -7.456977232089471386, 217.1783343296987709, 26.94886208192142973 ) ) ;
#5743 = CARTESIAN_POINT ( 'NONE',  ( -10.00000000000000711, 206.9523078486584495, 41.49886208192143044 ) ) ;
#5744 = CARTESIAN_POINT ( 'NONE',  ( 79.49999999453764588, 139.7537977485451393, -4.138211985947621020E-15 ) ) ;
#5745 = CARTESIAN_POINT ( 'NONE',  ( -3.662846001190052991, 218.4274158808045740, 73.10113791807857808 ) ) ;
#5746 = CARTESIAN_POINT ( 'NONE',  ( 8.015496119326531499, 209.5516654185219636, 91.85113791807857808 ) ) ;
#5747 = CARTESIAN_POINT ( 'NONE',  ( -8.062137200540822946, 201.0835637161416400, 50.19886208192144039 ) ) ;
#5748 = EDGE_CURVE ( 'NONE', #28277, #6898, #21106, .T. ) ;
#5749 = DIRECTION ( 'NONE',  ( 0.000000000000000000, 0.000000000000000000, -1.000000000000000000 ) ) ;
#5750 = VERTEX_POINT ( 'NONE', #20697 ) ;
#5751 = CARTESIAN_POINT ( 'NONE',  ( 3.662846001189864698, 218.4274158808046593, 48.39886208192143613 ) ) ;
#5752 = VERTEX_POINT ( 'NONE', #30756 ) ;
#5753 = ORIENTED_EDGE ( 'NONE', *, *, #1070, .T. ) ;
#5754 = CARTESIAN_POINT ( 'NONE',  ( 78.87499999726880162, 138.6155565068815747, -3.929120461958505118E-15 ) ) ;
#5755 = CARTESIAN_POINT ( 'NONE',  ( 86.98867513459482836, 163.8167787843871110, -12.13525491562423397 ) ) ;
#5756 = ADVANCED_FACE ( 'NONE', ( #5190 ), #5330, .F. ) ;
#5757 = CARTESIAN_POINT ( 'NONE',  ( 10.40000000000000036, 0.000000000000000000, 0.000000000000000000 ) ) ;
#5758 = CARTESIAN_POINT ( 'NONE',  ( 6.500168698208129925, 211.6636982574063381, 55.70113791807857240 ) ) ;
#5759 = CARTESIAN_POINT ( 'NONE',  ( 125.0000000000000000, 4.592425496802574367E-14, 35.00000000000000000 ) ) ;
#5760 = CARTESIAN_POINT ( 'NONE',  ( 3.135527875058981895, 197.5041725223112792, 31.59886208192143187 ) ) ;
#5761 = CARTESIAN_POINT ( 'NONE',  ( 61.07499999726881157, 141.7447067706911810, -9.630534252274387086 ) ) ;
#5762 = VERTEX_POINT ( 'NONE', #17800 ) ;
#5763 = LINE ( 'NONE', #8339, #17293 ) ;
#5764 = DIRECTION ( 'NONE',  ( 1.000000000000000000, 0.000000000000000000, 0.000000000000000000 ) ) ;
#5765 = CARTESIAN_POINT ( 'NONE',  ( 6.444103211790928043, 211.7408657792734061, 9.698862081921433287 ) ) ;
#5766 = CARTESIAN_POINT ( 'NONE',  ( -0.05014649552810635652, 196.4853777576173002, 53.75113791807857666 ) ) ;
#5767 = CARTESIAN_POINT ( 'NONE',  ( 82.98867513459481415, 163.8167787843871110, -12.13525491562423397 ) ) ;
#5768 = EDGE_CURVE ( 'NONE', #697, #7491, #2484, .T. ) ;
#5769 = CARTESIAN_POINT ( 'NONE',  ( -10.01549611932653860, 203.7984951890123284, 39.35113791807857098 ) ) ;
#5770 = CARTESIAN_POINT ( 'NONE',  ( 82.97499999726881015, 140.1801316387863778, -4.815267126137194431 ) ) ;
#5771 = CARTESIAN_POINT ( 'NONE',  ( -2.426778023690076225, 199.3768101843759553, 88.89886208192143613 ) ) ;
#5772 = CARTESIAN_POINT ( 'NONE',  ( 40.32499999726881157, 145.8408176439707802, 12.60653300113718345 ) ) ;
#5773 = CARTESIAN_POINT ( 'NONE',  ( 36.38867513459481984, 140.7341522555726669, -4.635254915624220651 ) ) ;
#5774 = DIRECTION ( 'NONE',  ( 0.000000000000000000, 1.000000000000000000, 0.000000000000000000 ) ) ;
#5775 = CARTESIAN_POINT ( 'NONE',  ( 11.98450388067348271, 203.0532714938637753, 8.151137918078566358 ) ) ;
#5776 = CARTESIAN_POINT ( 'NONE',  ( 2.558993250143296372, -7.638875775590942219, -7.593821156097518177 ) ) ;
#5777 = CARTESIAN_POINT ( 'NONE',  ( 58.97499999726881015, 140.1801316387863778, -4.815267126137194431 ) ) ;
#5778 = EDGE_CURVE ( 'NONE', #8601, #31418, #8571, .T. ) ;
#5779 = CARTESIAN_POINT ( 'NONE',  ( 6.220909254589536808, 215.4770327129947702, 64.55113791807858092 ) ) ;
#5780 = CARTESIAN_POINT ( 'NONE',  ( 3.135527875058820690, 216.4958274776887492, 31.40113791807857524 ) ) ;
#5781 = CARTESIAN_POINT ( 'NONE',  ( 79.50000000000000000, 155.0000000000000000, 13.50000000000000355 ) ) ;
#5782 = CARTESIAN_POINT ( 'NONE',  ( 54.98867513459482126, 163.8167787843871110, -12.13525491562423397 ) ) ;
#5783 = CARTESIAN_POINT ( 'NONE',  ( -3.044812012439970683, 197.4746971517856196, 13.89886208192143613 ) ) ;
#5784 = CARTESIAN_POINT ( 'NONE',  ( 57.39999999453762314, 141.2096805137202580, 4.480746418436733158 ) ) ;
#5785 = ORIENTED_EDGE ( 'NONE', *, *, #3474, .F. ) ;
#5786 = CARTESIAN_POINT ( 'NONE',  ( -11.98450388067348804, 210.9467285061362247, 39.65113791807857524 ) ) ;
#5787 = DIRECTION ( 'NONE',  ( 0.000000000000000000, -1.000000000000000000, 9.682177540335733218E-15 ) ) ;
#5788 = CARTESIAN_POINT ( 'NONE',  ( 9.984503880673420539, 210.2968891136705167, 21.84886208192143542 ) ) ;
#5789 = CARTESIAN_POINT ( 'NONE',  ( 59.31132485994280756, 140.7341522555726669, -4.635254915624220651 ) ) ;
#5790 = AXIS2_PLACEMENT_3D ( 'NONE', #30636, #2184, #12569 ) ;
#5791 = EDGE_LOOP ( 'NONE', ( #18595, #33002, #16146, #33387 ) ) ;
#5792 = CARTESIAN_POINT ( 'NONE',  ( -3.044812012440131443, 216.5253028482142952, 82.10113791807857808 ) ) ;
#5793 = ORIENTED_EDGE ( 'NONE', *, *, #14291, .F. ) ;
#5794 = DIRECTION ( 'NONE',  ( -1.000000000000000000, -0.000000000000000000, 0.000000000000000000 ) ) ;
#5795 = CARTESIAN_POINT ( 'NONE',  ( 4.000000000000000000, 0.000000000000000000, 0.000000000000000000 ) ) ;
#5796 = VERTEX_POINT ( 'NONE', #15747 ) ;
#5797 = CARTESIAN_POINT ( 'NONE',  ( 4.903702542908601636, 200.1653181626581102, 14.45113791807856707 ) ) ;
#5798 = B_SPLINE_CURVE_WITH_KNOTS ( 'NONE', 3,
 ( #4161, #22226, #9452, #9279, #30237, #12177 ),
 .UNSPECIFIED., .F., .F.,
 ( 4, 2, 4 ),
 ( 0.002044882221487520201, 0.003063384235218497183, 0.004081886248949473731 ),
 .UNSPECIFIED. ) ;
#5799 = ADVANCED_FACE ( 'NONE', ( #2810, #413 ), #3295, .T. ) ;
#5800 = CARTESIAN_POINT ( 'NONE',  ( -58.66318290517560996, 194.9217985566783113, -2.499999999999999556 ) ) ;
#5801 = VECTOR ( 'NONE', #16860, 1000.000000000000000 ) ;
#5802 = CARTESIAN_POINT ( 'NONE',  ( 11.98450388067341876, 210.9467285061363953, 96.84886208192143897 ) ) ;
#5803 = CARTESIAN_POINT ( 'NONE',  ( 43.67499999726881299, 168.2552932293087906, -9.630534252274387086 ) ) ;
#5804 = ORIENTED_EDGE ( 'NONE', *, *, #7261, .T. ) ;
#5805 = CARTESIAN_POINT ( 'NONE',  ( 50.72499999726881725, 140.1801316387863778, -4.815267126137194431 ) ) ;
#5806 = FACE_OUTER_BOUND ( 'NONE', #11322, .T. ) ;
#5807 = DIRECTION ( 'NONE',  ( 1.000000000000000000, 0.000000000000000000, 0.000000000000000000 ) ) ;
#5808 = AXIS2_PLACEMENT_3D ( 'NONE', #30844, #10725, #2560 ) ;
#5809 = CARTESIAN_POINT ( 'NONE',  ( 92.60208470531341618, 155.0000000000000000, 12.10452846326766441 ) ) ;
#5810 = CARTESIAN_POINT ( 'NONE',  ( -10.01549611932659722, 210.2015048109875011, 83.64886208192143613 ) ) ;
#5811 = CARTESIAN_POINT ( 'NONE',  ( 55.27499999726881441, 149.9369285172503510, -15.58253175000000823 ) ) ;
#5812 = CARTESIAN_POINT ( 'NONE',  ( -9.984503880673473830, 210.2968891136704315, 24.65113791807856103 ) ) ;
#5813 = CARTESIAN_POINT ( 'NONE',  ( 73.58867513459482268, 163.8167787843871110, 12.13525491562421621 ) ) ;
#5814 = EDGE_CURVE ( 'NONE', #25971, #22347, #33642, .T. ) ;
#5815 = CARTESIAN_POINT ( 'NONE',  ( 3.753561863808876797, 195.6020594897209719, 79.59886208192143897 ) ) ;
#5816 = CIRCLE ( 'NONE', #16147, 12.00000000000001066 ) ;
#5817 = CARTESIAN_POINT ( 'NONE',  ( 75.09999999999999432, 168.7903194862797420, 4.480746418436729606 ) ) ;
#5818 = CARTESIAN_POINT ( 'NONE',  ( 65.48867513459484258, 167.7597621252805880, 9.270509831248428867 ) ) ;
#5819 = DIRECTION ( 'NONE',  ( 0.000000000000000000, 0.000000000000000000, 1.000000000000000000 ) ) ;
#5820 = CARTESIAN_POINT ( 'NONE',  ( 10.01549611932653860, 210.2015048109876716, 85.85113791807857808 ) ) ;
#5821 = CARTESIAN_POINT ( 'NONE',  ( 27.50000000000001066, -15.87713240271473580, -15.54379906938135214 ) ) ;
#5822 = CARTESIAN_POINT ( 'NONE',  ( 36.77499999726881441, 140.1801316387863778, 4.815267126137185549 ) ) ;
#5823 = EDGE_CURVE ( 'NONE', #7737, #17237, #33073, .T. ) ;
#5824 = CARTESIAN_POINT ( 'NONE',  ( -7.375838497908014268, 196.7627149292498530, 98.04886208192144181 ) ) ;
#5825 = CARTESIAN_POINT ( 'NONE',  ( 74.52499999726880731, 140.1801316387863778, 4.815267126137185549 ) ) ;
#5826 = VERTEX_POINT ( 'NONE', #21025 ) ;
#5827 = CARTESIAN_POINT ( 'NONE',  ( 1.500000000000001332, 0.000000000000000000, 0.000000000000000000 ) ) ;
#5828 = CARTESIAN_POINT ( 'NONE',  ( 39.69999999453763451, 142.6655632788954620, -8.961492836873480528 ) ) ;
#5829 = CARTESIAN_POINT ( 'NONE',  ( -7.375838497908182134, 217.2372850707499765, 12.95113791807856707 ) ) ;
#5830 = VECTOR ( 'NONE', #7513, 1000.000000000000000 ) ;
#5831 = CARTESIAN_POINT ( 'NONE',  ( 3.500000000000004885, 2.020725942163702715, -2.587392608830344720 ) ) ;
#5832 = CARTESIAN_POINT ( 'NONE',  ( 3.500000000000004885, -0.3414694520252363752, -3.023060588750597910E-15 ) ) ;
#5833 = ORIENTED_EDGE ( 'NONE', *, *, #6366, .F. ) ;
#5834 = VECTOR ( 'NONE', #19885, 1000.000000000000000 ) ;
#5835 = CARTESIAN_POINT ( 'NONE',  ( 8.062137200540822946, 212.9164362838583315, 93.69886208192143329 ) ) ;
#5836 = CARTESIAN_POINT ( 'NONE',  ( -9.736236675708031640, 214.0148392665760753, 35.79886208192143471 ) ) ;
#5837 = CARTESIAN_POINT ( 'NONE',  ( -10.47863426674271814, 207.9189531262114770, 102.6635298682156758 ) ) ;
#5838 = CARTESIAN_POINT ( 'NONE',  ( -6.220909254589537696, 198.5229672870051161, 51.05113791807856671 ) ) ;
#5839 = ORIENTED_EDGE ( 'NONE', *, *, #1992, .F. ) ;
#5840 = CARTESIAN_POINT ( 'NONE',  ( -7.984503880673422316, 204.3529502787951628, 2.348862081921434974 ) ) ;
#5841 = CIRCLE ( 'NONE', #30342, 18.00000000000000000 ) ;
#5842 = CARTESIAN_POINT ( 'NONE',  ( 79.28867513459482552, 170.7719333635740497, -7.904646289410545231E-15 ) ) ;
#5843 = ORIENTED_EDGE ( 'NONE', *, *, #21234, .F. ) ;
#5844 = CARTESIAN_POINT ( 'NONE',  ( -2.426778023690076225, 199.3768101843759553, 88.89886208192143613 ) ) ;
#5845 = EDGE_CURVE ( 'NONE', #2840, #25792, #21193, .T. ) ;
#5846 = CARTESIAN_POINT ( 'NONE',  ( -8.015496119326531499, 204.4483345814780364, 30.35113791807856742 ) ) ;
#5847 = DIRECTION ( 'NONE',  ( 0.000000000000000000, 0.000000000000000000, -1.000000000000000000 ) ) ;
#5848 = VERTEX_POINT ( 'NONE', #21521 ) ;
#5849 = DIRECTION ( 'NONE',  ( 0.000000000000000000, 0.000000000000000000, -1.000000000000000000 ) ) ;
#5850 = VECTOR ( 'NONE', #31344, 1000.000000000000000 ) ;
#5851 = CARTESIAN_POINT ( 'NONE',  ( 86.22499999726882436, 149.9369285172503510, 15.58253174999999580 ) ) ;
#5852 = DIRECTION ( 'NONE',  ( 0.000000000000000000, 0.000000000000000000, -1.000000000000000000 ) ) ;
#5853 = CARTESIAN_POINT ( 'NONE',  ( -8.000000000000008882, 207.0476921513413515, 102.5011379180785696 ) ) ;
#5854 = EDGE_CURVE ( 'NONE', #5679, #27924, #29031, .T. ) ;
#5855 = CARTESIAN_POINT ( 'NONE',  ( 52.39999999999999858, 150.2886644046228639, -14.50000000000000888 ) ) ;
#5856 = CARTESIAN_POINT ( 'NONE',  ( -0.05014649552828365914, 215.4116977939061144, 75.24886208192143044 ) ) ;
#5857 = LINE ( 'NONE', #14380, #30890 ) ;
#5858 = AXIS2_PLACEMENT_3D ( 'NONE', #27282, #27120, #11616 ) ;
#5859 = CARTESIAN_POINT ( 'NONE',  ( 55.72499999726881015, 169.8198683612136222, 4.815267126137181997 ) ) ;
#5861 = ORIENTED_EDGE ( 'NONE', *, *, #8546, .T. ) ;
#5860 = CARTESIAN_POINT ( 'NONE',  ( 8.062137200540920645, 201.0835637161417822, 11.30113791807856671 ) ) ;
#5862 = DIRECTION ( 'NONE',  ( 0.000000000000000000, 1.000000000000000000, -3.227392513445223895E-15 ) ) ;
#5863 = CARTESIAN_POINT ( 'NONE',  ( 61.82499999726881157, 168.2552932293087906, 9.630534252274372875 ) ) ;
#5864 = CARTESIAN_POINT ( 'NONE',  ( 77.67499999726879878, 168.2552932293087906, -9.630534252274385310 ) ) ;
#5865 = CARTESIAN_POINT ( 'NONE',  ( 11.98450388067348271, 203.0532714938637753, 80.15113791807857524 ) ) ;
#5866 = DIRECTION ( 'NONE',  ( 0.000000000000000000, 0.000000000000000000, 1.000000000000000000 ) ) ;
#5867 = CARTESIAN_POINT ( 'NONE',  ( 9.984503880673473830, 203.7031108863295401, 95.15113791807857524 ) ) ;
#5868 = CYLINDRICAL_SURFACE ( 'NONE', #2026, 112.0000000000000426 ) ;
#5869 = VERTEX_POINT ( 'NONE', #7927 ) ;
#5870 = CARTESIAN_POINT ( 'NONE',  ( -3.753561863808878130, 218.3979405102790281, 102.0988620819214532 ) ) ;
#5871 = CARTESIAN_POINT ( 'NONE',  ( -9.736236675708031640, 214.0148392665760753, 59.79886208192143471 ) ) ;
#5872 = CARTESIAN_POINT ( 'NONE',  ( 0.05014649552828275014, 196.4853777576173002, 67.74886208192141623 ) ) ;
#5873 = CARTESIAN_POINT ( 'NONE',  ( 0.05014649552828288198, 194.3824533091408000, 1.748862081921433775 ) ) ;
#5874 = CARTESIAN_POINT ( 'NONE',  ( 32.50000000000000000, 155.0000000000000000, -15.00000000000002487 ) ) ;
#5875 = AXIS2_PLACEMENT_3D ( 'NONE', #9804, #33475, #22748 ) ;
#5876 = CARTESIAN_POINT ( 'NONE',  ( 3.135527875058820690, 216.4958274776887492, 25.40113791807856813 ) ) ;
#5877 = CARTESIAN_POINT ( 'NONE',  ( -9.984503880673420539, 203.7031108863293980, 80.34886208192143897 ) ) ;
#5878 = AXIS2_PLACEMENT_3D ( 'NONE', #21765, #824, #31663 ) ;
#5879 = ORIENTED_EDGE ( 'NONE', *, *, #31797, .T. ) ;
#5880 = CIRCLE ( 'NONE', #24423, 1.000000000000000888 ) ;
#5881 = CARTESIAN_POINT ( 'NONE',  ( 3.135527875058820690, 216.4958274776887492, 97.40113791807858945 ) ) ;
#5882 = ORIENTED_EDGE ( 'NONE', *, *, #8451, .F. ) ;
#5883 = CARTESIAN_POINT ( 'NONE',  ( 6.444103211790928043, 211.7408657792734061, 57.69886208192144039 ) ) ;
#5884 = ORIENTED_EDGE ( 'NONE', *, *, #9752, .T. ) ;
#5885 = CARTESIAN_POINT ( 'NONE',  ( 74.72499999726881015, 140.1801316387863778, -4.815267126137194431 ) ) ;
#5886 = ORIENTED_EDGE ( 'NONE', *, *, #27285, .T. ) ;
#5887 = FACE_OUTER_BOUND ( 'NONE', #9103, .T. ) ;
#5888 = UNCERTAINTY_MEASURE_WITH_UNIT (LENGTH_MEASURE( 1.000000000000000082E-05 ), #26387, 'distance_accuracy_value', 'NONE');
#5889 = CARTESIAN_POINT ( 'NONE',  ( 70.32499999726881867, 145.8408176439707802, 12.60653300113718345 ) ) ;
#5890 = CARTESIAN_POINT ( 'NONE',  ( -4.984841277089726574, 200.2242689037092305, 72.05113791807858092 ) ) ;
#5891 = DIRECTION ( 'NONE',  ( 1.000000000000000000, 0.000000000000000000, -0.000000000000000000 ) ) ;
#5892 = CARTESIAN_POINT ( 'NONE',  ( 2.000000000000000000, 1.329782007511004727, -0.7677500000000019309 ) ) ;
#5893 =( NAMED_UNIT ( * ) PLANE_ANGLE_UNIT ( ) SI_UNIT ( $, .RADIAN. ) );
#5894 = CARTESIAN_POINT ( 'NONE',  ( 35.70000000000000284, 146.4771138417591203, 11.73074641843673227 ) ) ;
#5895 = CARTESIAN_POINT ( 'NONE',  ( 7.984503880673422316, 209.6470497212048372, 39.84886208192144608 ) ) ;
#5896 = AXIS2_PLACEMENT_3D ( 'NONE', #20590, #23802, #5576 ) ;
#5897 = CARTESIAN_POINT ( 'NONE',  ( -9.984503880673473830, 210.2968891136704315, 81.65113791807857524 ) ) ;
#5898 = CARTESIAN_POINT ( 'NONE',  ( 6.139770520408368348, 198.4640165459539674, 68.45113791807858661 ) ) ;
#5899 = CIRCLE ( 'NONE', #26060, 2.466666666666999408 ) ;
#5900 = CARTESIAN_POINT ( 'NONE',  ( 127.5000000000000000, 228.4330392262239116, 76.47359838532422316 ) ) ;
#5901 = CARTESIAN_POINT ( 'NONE',  ( -7.984503880673488041, 209.6470497212046098, 24.65113791807857169 ) ) ;
#5902 = CARTESIAN_POINT ( 'NONE',  ( -27.50000000000001066, 1.342284157770889275, -18.00000000000000355 ) ) ;
#5903 = DIRECTION ( 'NONE',  ( 0.000000000000000000, 0.000000000000000000, 1.000000000000000000 ) ) ;
#5904 = CARTESIAN_POINT ( 'NONE',  ( 45.72499999726881015, 169.8198683612136222, 4.815267126137181997 ) ) ;
#5905 = CARTESIAN_POINT ( 'NONE',  ( 12.00000000000000711, 206.9523078486586485, 50.00113791807856956 ) ) ;
#5906 = CARTESIAN_POINT ( 'NONE',  ( 127.5000000000000000, 48.99999999999998579, 2.149999999999971489 ) ) ;
#5907 = CARTESIAN_POINT ( 'NONE',  ( -9.984503880673473830, 210.2968891136704315, 99.65113791807853261 ) ) ;
#5908 = CARTESIAN_POINT ( 'NONE',  ( 10.00000000000000711, 206.9523078486586201, 71.00113791807858377 ) ) ;
#5909 = CIRCLE ( 'NONE', #5390, 5.200000000000009948 ) ;
#5910 = CARTESIAN_POINT ( 'NONE',  ( 11.98450388067341876, 210.9467285061363953, 30.84886208192143542 ) ) ;
#5911 = CARTESIAN_POINT ( 'NONE',  ( 6.220909254589680693, 198.5229672870052582, 37.44886208192143329 ) ) ;
#5912 = CARTESIAN_POINT ( 'NONE',  ( 77.69999999453762030, 142.6655632788954620, -8.961492836873480528 ) ) ;
#5913 = CARTESIAN_POINT ( 'NONE',  ( -7.375838497908182134, 217.2372850707499765, 75.95113791807857240 ) ) ;
#5914 = CARTESIAN_POINT ( 'NONE',  ( -6.444103211791042618, 211.7408657792732356, 90.80113791807858092 ) ) ;
#5915 = CARTESIAN_POINT ( 'NONE',  ( -3.135527875058982783, 216.4958274776886924, 48.09886208192143187 ) ) ;
#5916 = DIRECTION ( 'NONE',  ( 0.000000000000000000, -0.7071067811865540120, -0.7071067811865411334 ) ) ;
#5917 = ORIENTED_EDGE ( 'NONE', *, *, #26515, .F. ) ;
#5918 = CARTESIAN_POINT ( 'NONE',  ( -3.662846001189865142, 195.5725841191952838, 58.89886208192143613 ) ) ;
#5919 = ORIENTED_EDGE ( 'NONE', *, *, #24563, .F. ) ;
#5920 = CARTESIAN_POINT ( 'NONE',  ( 2.517493886309087436, 199.4062855549015865, 28.59886208192143897 ) ) ;
#5921 = CIRCLE ( 'NONE', #7584, 2.149999999999984812 ) ;
#5922 = ORIENTED_EDGE ( 'NONE', *, *, #19778, .F. ) ;
#5923 = CARTESIAN_POINT ( 'NONE',  ( 73.87499999726881583, 171.3844434931184253, -7.942151717890134290E-15 ) ) ;
#5924 = CARTESIAN_POINT ( 'NONE',  ( 53.61132485994281183, 150.1262045565062806, -14.99999999999993072 ) ) ;
#5925 = AXIS2_PLACEMENT_3D ( 'NONE', #4946, #26393, #15334 ) ;
#5926 = FACE_OUTER_BOUND ( 'NONE', #26057, .T. ) ;
#5927 = CARTESIAN_POINT ( 'NONE',  ( -2.426778023690262742, 214.6231898156240163, 52.10113791807857808 ) ) ;
#5928 = DIRECTION ( 'NONE',  ( -1.000000000000000000, 0.000000000000000000, 0.000000000000000000 ) ) ;
#5929 =( REPRESENTATION_RELATIONSHIP ('NONE','NONE', #25663, #1289 ) REPRESENTATION_RELATIONSHIP_WITH_TRANSFORMATION ( #25864 )SHAPE_REPRESENTATION_RELATIONSHIP( ) );
#5930 = CARTESIAN_POINT ( 'NONE',  ( -6.220909254589682469, 215.4770327129946850, 29.94886208192142973 ) ) ;
#5931 = CARTESIAN_POINT ( 'NONE',  ( 66.67499999726881299, 141.7447067706911810, 9.630534252274376428 ) ) ;
#5932 = VERTEX_POINT ( 'NONE', #13355 ) ;
#5933 = CARTESIAN_POINT ( 'NONE',  ( 40.78867513459481842, 155.0000000000000000, -15.00000000000002487 ) ) ;
#5934 = CARTESIAN_POINT ( 'NONE',  ( -58.50000000000001421, -88.00000000000000000, -20.00000000000000000 ) ) ;
#5935 = CARTESIAN_POINT ( 'NONE',  ( 0.05014649552828262524, 198.5883022060938572, 10.74886208192143577 ) ) ;
#5936 = CARTESIAN_POINT ( 'NONE',  ( -0.05014649552810635652, 196.4853777576173002, 47.75113791807855534 ) ) ;
#5937 = CARTESIAN_POINT ( 'NONE',  ( 80.11132485994279762, 169.2658477444273331, -4.635254915624224203 ) ) ;
#5938 = EDGE_CURVE ( 'NONE', #29827, #8405, #10789, .T. ) ;
#5939 = CARTESIAN_POINT ( 'NONE',  ( -3.135527875058821579, 197.5041725223112223, 35.90113791807856813 ) ) ;
#5940 = CARTESIAN_POINT ( 'NONE',  ( 82.57499999726880446, 145.8408176439707802, 12.60653300113718345 ) ) ;
#5941 = APPLICATION_PROTOCOL_DEFINITION ( 'draft international standard', 'automotive_design', 1998, #6585 ) ;
#5942 = CARTESIAN_POINT ( 'NONE',  ( 6.500168698208244500, 202.3363017425938324, 103.2988620819214560 ) ) ;
#5943 = CARTESIAN_POINT ( 'NONE',  ( 37.72499999726881015, 169.8198683612136222, 4.815267126137181997 ) ) ;
#5944 = CARTESIAN_POINT ( 'NONE',  ( 36.78867513459482552, 155.0000000000000000, -15.00000000000002487 ) ) ;
#5945 = DIRECTION ( 'NONE',  ( 8.584654849926598947E-16, -1.000000000000000000, 0.000000000000000000 ) ) ;
#5946 = CARTESIAN_POINT ( 'NONE',  ( 11.98450388067348271, 203.0532714938637753, 17.15113791807856458 ) ) ;
#5947 = AXIS2_PLACEMENT_3D ( 'NONE', #4286, #14675, #25069 ) ;
#5948 = CARTESIAN_POINT ( 'NONE',  ( 4.419133455864432847, -6.108866147516184952, -7.026396753507086146 ) ) ;
#5949 = CARTESIAN_POINT ( 'NONE',  ( 56.87499999726880162, 138.6155565068815463, -3.929120461958505118E-15 ) ) ;
#5950 = CARTESIAN_POINT ( 'NONE',  ( -8.062137200540920645, 212.9164362838581894, 66.80113791807858092 ) ) ;
#5951 = CARTESIAN_POINT ( 'NONE',  ( -6.220909254589537696, 198.5229672870051445, 36.05113791807857382 ) ) ;
#5952 = DIRECTION ( 'NONE',  ( -1.000000000000000000, -0.000000000000000000, -0.000000000000000000 ) ) ;
#5953 = EDGE_CURVE ( 'NONE', #21331, #2045, #25465, .T. ) ;
#5954 = DIRECTION ( 'NONE',  ( 0.000000000000000000, -0.04769215134144032253, 0.9988620819214358848 ) ) ;
#5955 = CARTESIAN_POINT ( 'NONE',  ( 10.01549611932659367, 203.7984951890124421, 7.148862081921434353 ) ) ;
#5956 = CARTESIAN_POINT ( 'NONE',  ( 58.09999999453763309, 159.7113355953771077, -14.50000000000000888 ) ) ;
#5957 = ORIENTED_EDGE ( 'NONE', *, *, #27883, .F. ) ;
#5958 = CARTESIAN_POINT ( 'NONE',  ( 9.680171189290831535, 199.9079932115568852, 53.30113791807857382 ) ) ;
#5959 = FACE_OUTER_BOUND ( 'NONE', #15281, .T. ) ;
#5960 = CARTESIAN_POINT ( 'NONE',  ( -0.05014649552828403384, 217.5146222423826714, 24.24886208192143044 ) ) ;
#5961 = CARTESIAN_POINT ( 'NONE',  ( 72.31132485994281467, 169.2658477444273331, 4.635254915624208216 ) ) ;
#5962 = ORIENTED_EDGE ( 'NONE', *, *, #10995, .T. ) ;
#5963 =( BOUNDED_CURVE ( )  B_SPLINE_CURVE ( 2, ( #32347, #9514, #27564, #22459, #3891, #14790, #17010, #9011, #19400, #1348, #14286, #11735, #27404, #4231, #14629, #30300, #32851, #17356, #27742, #31148, #26196, #25869, #7985, #31319, #20926, #15302, #5082, #30647, #18369, #20243, #15636, #25527, #28596, #26040, #2710, #22971, #7815, #20422, #12755, #5247, #22807, #28761, #15803, #2196, #33197, #10378, #15478, #2535, #28079, #18032, #33370, #17692, #13088, #2864, #30815, #28427, #5418, #17863, #4740, #12578, #30993, #12918, #7478, #20592, #18205, #10545, #23314, #23477, #9861, #17921, #144, #23146, #28261, #7650, #4915, #7315, #15132, #10044, #25694, #2365, #33534, #10207, #20751, #10873, #3519, #29089, #6242, #23804, #18536, #18700, #6067, #21248, #13249, #31486, #476, #8468, #26520, #26689, #16461, #15971, #23645, #13912, #8309, #31641, #3350, #26859, #5737, #13740, #16630, #24297, #16128, #305, #3192, #965, #10704, #24137, #13581, #8153, #23972, #804, #11194, #21082, #19194, #634, #29591, #32135, #5904, #11033, #21415, #21573, #31802, #28918, #5578, #18856, #27026, #11365, #29252, #26365, #16298, #21745, #3024, #13410, #31965, #8797, #8636, #19029, #29417, #32805, #6920, #14417, #30258, #32307, #32639, #17140, #16965, #20034, #3686, #14245, #30087, #32973, #22082, #27360, #1803, #6752, #22587, #12200, #9639, #29928, #19694, #11528, #30434, #1135, #17311, #6417, #9472, #27701, #4363, #3853, #12027, #1310, #4026, #16800, #7094, #17475, #14079, #27197, #24474, #24984, #27526, #4187, #8969, #9302, #24644, #19359, #14746, #21910, #11699, #14583, #29754, #32468, #9135, #1635, #25139, #22415, #19534, #1470, #19860, #6581, #24810, #11865, #22252, #10160, #18164, #17815, #25481, #25653, #9993, #7941, #14925, #25994, #12538, #22928, #33323, #102, #2492, #17994, #13047, #27860, #4532, #20380, #22764, #33663, #4698, #28558, #2664, #15088, #5206, #20543, #10504, #7434, #4872, #30601, #25313, #28037, #20883, #30772, #28213, #10339, #15261, #2320, #5042, #2155, #23437, #15592, #9820, #12707, #31281, #23103, #1977, #33491, #30945, #28385, #15432, #7610, #25828, #20711, #7266, #12368, #12875, #33157, #23268, #31111, #7773, #20201, #17649, #29211, #28879, #16420, #8596, #270, #5535, #15762, #8431, #8268, #2823, #15925, #18817, #5863, #594, #13538, #18656, #10665, #23932, #11160, #13368, #26323, #761, #13694, #21535, #29046, #31925, #11324, #18992, #2988, #21041, #10990, #29382, #16088, #5700, #23765, #16260, #26482, #26816, #21369, #3480, #13871, #24256, #10832, #31765, #26157, #926, #26646, #21708, #3310, #3151, #24094, #13207, #6028, #18494, #32099, #18323, #31444, #28718, #5374, #23606, #8112, #430, #21207, #31601, #14041, #19150, #3646, #8762, #16590, #24437, #1101, #26982, #6201, #29547, #11494, #21872, #7293, #22787, #13068, #12898, #4896, #33180, #31130, #25334, #4721, #28405, #7795, #30795, #15112, #15282, #22952, #20905, #27885, #5228, #25506, #14947, #33349, #30625, #18185, #10021, #2176, #28578, #20402, #124, #17672, #12393, #33686, #12560, #7116, #2002, #28060, #2345, #7457, #20569, #17839, #28239, #9843, #15614, #25676, #4559, #23458, #12735, #10526, #26019, #33512, #23124, #23293, #2512, #10360, #10186, #20733, #20224, #30972, #7632, #18014, #17496, #5064, #15457, #25851, #2690, #15950, #5885, #947, #5399, #31623, #6051, #29402, #23787, #13564, #15782, #16442, #28739, #24118, #288, #3332, #785, #11178, #31466, #16282, #28900, #21228, #13717, #31301, #5720, #21555, #18838, #7963, #29233, #23953, #11013, #2843, #26504, #8133, #26175, #31948, #11347, #5556, #3173, #13894, #26345, #13230, #10682, #18517, #23625, #3503, #8618, #26671, #19013, #614, #26840, #24275, #21395, #18348, #8290, #3009, #29068, #13388, #21065, #457, #10855, #18680, #16108, #31785, #8452, #32788, #14230, #6904, #1784, #21728, #6398, #16612, #27514, #32292, #22397, #19848, #8953, #12011, #14406, #4348, #1293, #32450, #19342, #19516, #1621, #9461, #16784, #22067, #4172, #9119, #24628, #32624, #29735, #30245, #17297, #3668, #27183, #27685, #16948, #8781, #14732, #32118, #3839, #27343, #25122, #11684, #27007, #19175, #1454, #11850, #29572, #29912, #6738, #6223, #4011, #14567, #14062, #24798, #24458, #6566, #22235, #9286, #19680, #1121, #11513, #21893, #30072, #17128, #24968, #18146, #20525 ),
 .UNSPECIFIED., .F., .F. ) 
 B_SPLINE_CURVE_WITH_KNOTS ( ( 3, 2, 2, 2, 2, 2, 2, 2, 2, 2, 2, 2, 2, 2, 2, 2, 2, 2, 2, 2, 2, 2, 2, 2, 2, 2, 2, 2, 2, 2, 2, 2, 2, 2, 2, 2, 2, 2, 2, 2, 2, 2, 2, 2, 2, 2, 2, 2, 2, 2, 2, 2, 2, 2, 2, 2, 2, 2, 2, 2, 2, 2, 2, 2, 2, 2, 2, 2, 2, 2, 2, 2, 2, 2, 2, 2, 2, 2, 2, 2, 2, 2, 2, 2, 2, 2, 2, 2, 2, 2, 2, 2, 2, 2, 2, 2, 2, 2, 2, 2, 2, 2, 2, 2, 2, 2, 2, 2, 2, 2, 2, 2, 2, 2, 2, 2, 2, 2, 2, 2, 2, 2, 2, 2, 2, 2, 2, 2, 2, 2, 2, 2, 2, 2, 2, 2, 2, 2, 2, 2, 2, 2, 2, 2, 2, 2, 2, 2, 2, 2, 2, 2, 2, 2, 2, 2, 2, 2, 2, 2, 2, 2, 2, 2, 2, 2, 2, 2, 2, 2, 2, 2, 2, 2, 2, 2, 2, 2, 2, 2, 2, 2, 2, 2, 2, 2, 2, 2, 2, 2, 2, 2, 2, 2, 2, 2, 2, 2, 2, 2, 2, 2, 2, 2, 2, 2, 2, 2, 2, 2, 2, 2, 2, 2, 2, 2, 2, 2, 2, 2, 2, 2, 2, 2, 2, 2, 2, 2, 2, 2, 2, 2, 2, 2, 2, 2, 2, 2, 2, 2, 2, 2, 2, 2, 2, 2, 2, 2, 2, 2, 2, 2, 2, 2, 2, 2, 2, 2, 2, 2, 2, 2, 2, 2, 2, 2, 2, 2, 2, 2, 2, 2, 3 ),
 ( 0.000000000000000000, 0.003571428571428571317, 0.007142857142857142634, 0.01071428571428571438, 0.01428571428571428527, 0.01785714285714285615, 0.02142857142857142877, 0.02500000000000000139, 0.02857142857142857054, 0.03214285714285713969, 0.03571428571428571230, 0.03928571428571428492, 0.04285714285714285754, 0.04642857142857143016, 0.05000000000000000278, 0.05357142857142856845, 0.05714285714285714107, 0.06071428571428571369, 0.06428571428571427937, 0.06785714285714285199, 0.07142857142857142461, 0.07499999999999999722, 0.07857142857142856984, 0.08214285714285714246, 0.08571428571428571508, 0.08928571428571428770, 0.09285714285714286031, 0.09642857142857143293, 0.1000000000000000056, 0.1035714285714285782, 0.1071428571428571369, 0.1107142857142857095, 0.1142857142857142821, 0.1178571428571428548, 0.1214285714285714274, 0.1250000000000000000, 0.1285714285714285587, 0.1321428571428571452, 0.1357142857142857040, 0.1392857142857142905, 0.1428571428571428492, 0.1464285714285714357, 0.1499999999999999944, 0.1535714285714285809, 0.1571428571428571397, 0.1607142857142856984, 0.1642857142857142849, 0.1678571428571428437, 0.1714285714285714302, 0.1749999999999999889, 0.1785714285714285754, 0.1821428571428571341, 0.1857142857142857206, 0.1892857142857142794, 0.1928571428571428659, 0.1964285714285714524, 0.2000000000000000111, 0.2035714285714285698, 0.2071428571428571563, 0.2107142857142857151, 0.2142857142857142738, 0.2178571428571428603, 0.2214285714285714191, 0.2250000000000000056, 0.2285714285714285643, 0.2321428571428571230, 0.2357142857142857095, 0.2392857142857142960, 0.2428571428571428548, 0.2464285714285714413, 0.2500000000000000000, 0.2535714285714285587, 0.2571428571428571175, 0.2607142857142857317, 0.2642857142857142905, 0.2678571428571428492, 0.2714285714285714080, 0.2750000000000000222, 0.2785714285714285809, 0.2821428571428571397, 0.2857142857142856984, 0.2892857142857143127, 0.2928571428571428714, 0.2964285714285714302, 0.2999999999999999889, 0.3035714285714285476, 0.3071428571428571619, 0.3107142857142857206, 0.3142857142857142794, 0.3178571428571428381, 0.3214285714285713969, 0.3250000000000000111, 0.3285714285714285698, 0.3321428571428571286, 0.3357142857142856873, 0.3392857142857143016, 0.3428571428571428603, 0.3464285714285714191, 0.3499999999999999778, 0.3535714285714285920, 0.3571428571428571508, 0.3607142857142857095, 0.3642857142857142683, 0.3678571428571428825, 0.3714285714285714413, 0.3750000000000000000, 0.3785714285714285587, 0.3821428571428571175, 0.3857142857142857317, 0.3892857142857142905, 0.3928571428571429047, 0.3964285714285714080, 0.4000000000000000222, 0.4035714285714285809, 0.4071428571428571397, 0.4107142857142856984, 0.4142857142857143127, 0.4178571428571428714, 0.4214285714285714302, 0.4249999999999999889, 0.4285714285714285476, 0.4321428571428571619, 0.4357142857142857206, 0.4392857142857142794, 0.4428571428571428381, 0.4464285714285714524, 0.4500000000000000111, 0.4535714285714285698, 0.4571428571428571286, 0.4607142857142856873, 0.4642857142857142461, 0.4678571428571428603, 0.4714285714285714191, 0.4749999999999999778, 0.4785714285714285920, 0.4821428571428571508, 0.4857142857142857095, 0.4892857142857142683, 0.4928571428571428825, 0.4964285714285714413, 0.5000000000000000000, 0.5035714285714285587, 0.5071428571428571175, 0.5107142857142856762, 0.5142857142857142350, 0.5178571428571429047, 0.5214285714285714635, 0.5250000000000000222, 0.5285714285714285809, 0.5321428571428571397, 0.5357142857142856984, 0.5392857142857142572, 0.5428571428571428159, 0.5464285714285713746, 0.5500000000000000444, 0.5535714285714286031, 0.5571428571428571619, 0.5607142857142857206, 0.5642857142857142794, 0.5678571428571428381, 0.5714285714285713969, 0.5749999999999999556, 0.5785714285714286254, 0.5821428571428571841, 0.5857142857142857428, 0.5892857142857143016, 0.5928571428571428603, 0.5964285714285714191, 0.5999999999999999778, 0.6035714285714285365, 0.6071428571428570953, 0.6107142857142857650, 0.6142857142857143238, 0.6178571428571428825, 0.6214285714285714413, 0.6250000000000000000, 0.6285714285714285587, 0.6321428571428571175, 0.6357142857142856762, 0.6392857142857141239, 0.6428571428571427937, 0.6464285714285714635, 0.6500000000000000222, 0.6535714285714285809, 0.6571428571428571397, 0.6607142857142856984, 0.6642857142857142572, 0.6678571428571428159, 0.6714285714285713746, 0.6750000000000000444, 0.6785714285714286031, 0.6821428571428571619, 0.6857142857142857206, 0.6892857142857142794, 0.6928571428571428381, 0.6964285714285713969, 0.6999999999999999556, 0.7035714285714286254, 0.7071428571428571841, 0.7107142857142857428, 0.7142857142857143016, 0.7178571428571428603, 0.7214285714285714191, 0.7249999999999999778, 0.7285714285714285365, 0.7321428571428570953, 0.7357142857142857650, 0.7392857142857143238, 0.7428571428571428825, 0.7464285714285714413, 0.7500000000000000000, 0.7535714285714285587, 0.7571428571428571175, 0.7607142857142856762, 0.7642857142857142350, 0.7678571428571429047, 0.7714285714285714635, 0.7750000000000000222, 0.7785714285714285809, 0.7821428571428571397, 0.7857142857142858094, 0.7892857142857142572, 0.7928571428571428159, 0.7964285714285713746, 0.8000000000000000444, 0.8035714285714286031, 0.8071428571428571619, 0.8107142857142857206, 0.8142857142857142794, 0.8178571428571428381, 0.8214285714285713969, 0.8249999999999999556, 0.8285714285714286254, 0.8321428571428571841, 0.8357142857142857428, 0.8392857142857143016, 0.8428571428571428603, 0.8464285714285714191, 0.8499999999999999778, 0.8535714285714285365, 0.8571428571428570953, 0.8607142857142857650, 0.8642857142857143238, 0.8678571428571428825, 0.8714285714285714413, 0.8750000000000000000, 0.8785714285714285587, 0.8821428571428571175, 0.8857142857142856762, 0.8892857142857142350, 0.8928571428571429047, 0.8964285714285714635, 0.9000000000000000222, 0.9035714285714285809, 0.9071428571428571397, 0.9107142857142856984, 0.9142857142857142572, 0.9178571428571428159, 0.9214285714285713746, 0.9250000000000000444, 0.9285714285714284921, 0.9321428571428571619, 0.9357142857142857206, 0.9392857142857142794, 0.9428571428571428381, 0.9464285714285713969, 0.9499999999999999556, 0.9535714285714286254, 0.9571428571428571841, 0.9607142857142857428, 0.9642857142857143016, 0.9678571428571428603, 0.9709674003564926492 ),
 .UNSPECIFIED. ) 
 CURVE ( )  GEOMETRIC_REPRESENTATION_ITEM ( )  RATIONAL_B_SPLINE_CURVE ( ( 1.000000000000000000, 0.9510565162951535312, 1.000000000000000000, 0.9510565162951535312, 1.000000000000000000, 0.9510565162951535312, 1.000000000000000000, 0.9510565162951535312, 1.000000000000000000, 0.9510565162951535312, 1.000000000000000000, 0.9510565162951535312, 1.000000000000000000, 0.9510565162951535312, 1.000000000000000000, 0.9510565162951535312, 1.000000000000000000, 0.9510565162951535312, 1.000000000000000000, 0.9510565162951535312, 1.000000000000000000, 0.9510565162951535312, 1.000000000000000000, 0.9510565162951535312, 1.000000000000000000, 0.9510565162951535312, 1.000000000000000000, 0.9510565162951535312, 1.000000000000000000, 0.9510565162951535312, 1.000000000000000000, 0.9510565162951535312, 1.000000000000000000, 0.9510565162951535312, 1.000000000000000000, 0.9510565162951535312, 1.000000000000000000, 0.9510565162951535312, 1.000000000000000000, 0.9510565162951535312, 1.000000000000000000, 0.9510565162951535312, 1.000000000000000000, 0.9510565162951535312, 1.000000000000000000, 0.9510565162951535312, 1.000000000000000000, 0.9510565162951535312, 1.000000000000000000, 0.9510565162951535312, 1.000000000000000000, 0.9510565162951535312, 1.000000000000000000, 0.9510565162951535312, 1.000000000000000000, 0.9510565162951535312, 1.000000000000000000, 0.9510565162951535312, 1.000000000000000000, 0.9510565162951535312, 1.000000000000000000, 0.9510565162951535312, 1.000000000000000000, 0.9510565162951535312, 1.000000000000000000, 0.9510565162951535312, 1.000000000000000000, 0.9510565162951535312, 1.000000000000000000, 0.9510565162951535312, 1.000000000000000000, 0.9510565162951535312, 1.000000000000000000, 0.9510565162951535312, 1.000000000000000000, 0.9510565162951535312, 1.000000000000000000, 0.9510565162951535312, 1.000000000000000000, 0.9510565162951535312, 1.000000000000000000, 0.9510565162951535312, 1.000000000000000000, 0.9510565162951535312, 1.000000000000000000, 0.9510565162951535312, 1.000000000000000000, 0.9510565162951535312, 1.000000000000000000, 0.9510565162951535312, 1.000000000000000000, 0.9510565162951535312, 1.000000000000000000, 0.9510565162951535312, 1.000000000000000000, 0.9510565162951535312, 1.000000000000000000, 0.9510565162951535312, 1.000000000000000000, 0.9510565162951535312, 1.000000000000000000, 0.9510565162951535312, 1.000000000000000000, 0.9510565162951535312, 1.000000000000000000, 0.9510565162951535312, 1.000000000000000000, 0.9510565162951535312, 1.000000000000000000, 0.9510565162951535312, 1.000000000000000000, 0.9510565162951535312, 1.000000000000000000, 0.9510565162951535312, 1.000000000000000000, 0.9510565162951535312, 1.000000000000000000, 0.9510565162951535312, 1.000000000000000000, 0.9510565162951535312, 1.000000000000000000, 0.9510565162951535312, 1.000000000000000000, 0.9510565162951535312, 1.000000000000000000, 0.9510565162951535312, 1.000000000000000000, 0.9510565162951535312, 1.000000000000000000, 0.9510565162951535312, 1.000000000000000000, 0.9510565162951535312, 1.000000000000000000, 0.9510565162951535312, 1.000000000000000000, 0.9510565162951535312, 1.000000000000000000, 0.9510565162951535312, 1.000000000000000000, 0.9510565162951535312, 1.000000000000000000, 0.9510565162951535312, 1.000000000000000000, 0.9510565162951535312, 1.000000000000000000, 0.9510565162951535312, 1.000000000000000000, 0.9510565162951535312, 1.000000000000000000, 0.9510565162951535312, 1.000000000000000000, 0.9510565162951535312, 1.000000000000000000, 0.9510565162951535312, 1.000000000000000000, 0.9510565162951535312, 1.000000000000000000, 0.9510565162951535312, 1.000000000000000000, 0.9510565162951535312, 1.000000000000000000, 0.9510565162951535312, 1.000000000000000000, 0.9510565162951535312, 1.000000000000000000, 0.9510565162951535312, 1.000000000000000000, 0.9510565162951535312, 1.000000000000000000, 0.9510565162951535312, 1.000000000000000000, 0.9510565162951535312, 1.000000000000000000, 0.9510565162951535312, 1.000000000000000000, 0.9510565162951535312, 1.000000000000000000, 0.9510565162951535312, 1.000000000000000000, 0.9510565162951535312, 1.000000000000000000, 0.9510565162951535312, 1.000000000000000000, 0.9510565162951535312, 1.000000000000000000, 0.9510565162951535312, 1.000000000000000000, 0.9510565162951535312, 1.000000000000000000, 0.9510565162951535312, 1.000000000000000000, 0.9510565162951535312, 1.000000000000000000, 0.9510565162951535312, 1.000000000000000000, 0.9510565162951535312, 1.000000000000000000, 0.9510565162951535312, 1.000000000000000000, 0.9510565162951535312, 1.000000000000000000, 0.9510565162951535312, 1.000000000000000000, 0.9510565162951535312, 1.000000000000000000, 0.9510565162951535312, 1.000000000000000000, 0.9510565162951535312, 1.000000000000000000, 0.9510565162951535312, 1.000000000000000000, 0.9510565162951535312, 1.000000000000000000, 0.9510565162951535312, 1.000000000000000000, 0.9510565162951535312, 1.000000000000000000, 0.9510565162951535312, 1.000000000000000000, 0.9510565162951535312, 1.000000000000000000, 0.9510565162951535312, 1.000000000000000000, 0.9510565162951535312, 1.000000000000000000, 0.9510565162951535312, 1.000000000000000000, 0.9510565162951535312, 1.000000000000000000, 0.9510565162951535312, 1.000000000000000000, 0.9510565162951535312, 1.000000000000000000, 0.9510565162951535312, 1.000000000000000000, 0.9510565162951535312, 1.000000000000000000, 0.9510565162951535312, 1.000000000000000000, 0.9510565162951535312, 1.000000000000000000, 0.9510565162951535312, 1.000000000000000000, 0.9510565162951535312, 1.000000000000000000, 0.9510565162951535312, 1.000000000000000000, 0.9510565162951535312, 1.000000000000000000, 0.9510565162951535312, 1.000000000000000000, 0.9510565162951535312, 1.000000000000000000, 0.9510565162951535312, 1.000000000000000000, 0.9510565162951535312, 1.000000000000000000, 0.9510565162951535312, 1.000000000000000000, 0.9510565162951535312, 1.000000000000000000, 0.9510565162951535312, 1.000000000000000000, 0.9510565162951535312, 1.000000000000000000, 0.9510565162951535312, 1.000000000000000000, 0.9510565162951535312, 1.000000000000000000, 0.9510565162951535312, 1.000000000000000000, 0.9510565162951535312, 1.000000000000000000, 0.9510565162951535312, 1.000000000000000000, 0.9510565162951535312, 1.000000000000000000, 0.9510565162951535312, 1.000000000000000000, 0.9510565162951535312, 1.000000000000000000, 0.9510565162951535312, 1.000000000000000000, 0.9510565162951535312, 1.000000000000000000, 0.9510565162951535312, 1.000000000000000000, 0.9510565162951535312, 1.000000000000000000, 0.9510565162951535312, 1.000000000000000000, 0.9510565162951535312, 1.000000000000000000, 0.9510565162951535312, 1.000000000000000000, 0.9510565162951535312, 1.000000000000000000, 0.9510565162951535312, 1.000000000000000000, 0.9510565162951535312, 1.000000000000000000, 0.9510565162951535312, 1.000000000000000000, 0.9510565162951535312, 1.000000000000000000, 0.9510565162951535312, 1.000000000000000000, 0.9510565162951535312, 1.000000000000000000, 0.9510565162951535312, 1.000000000000000000, 0.9510565162951535312, 1.000000000000000000, 0.9510565162951535312, 1.000000000000000000, 0.9510565162951535312, 1.000000000000000000, 0.9510565162951535312, 1.000000000000000000, 0.9510565162951535312, 1.000000000000000000, 0.9510565162951535312, 1.000000000000000000, 0.9510565162951535312, 1.000000000000000000, 0.9510565162951535312, 1.000000000000000000, 0.9510565162951535312, 1.000000000000000000, 0.9510565162951535312, 1.000000000000000000, 0.9510565162951535312, 1.000000000000000000, 0.9510565162951535312, 1.000000000000000000, 0.9510565162951535312, 1.000000000000000000, 0.9510565162951535312, 1.000000000000000000, 0.9510565162951535312, 1.000000000000000000, 0.9510565162951535312, 1.000000000000000000, 0.9510565162951535312, 1.000000000000000000, 0.9510565162951535312, 1.000000000000000000, 0.9510565162951535312, 1.000000000000000000, 0.9510565162951535312, 1.000000000000000000, 0.9510565162951535312, 1.000000000000000000, 0.9510565162951535312, 1.000000000000000000, 0.9510565162951535312, 1.000000000000000000, 0.9510565162951535312, 1.000000000000000000, 0.9510565162951535312, 1.000000000000000000, 0.9510565162951535312, 1.000000000000000000, 0.9510565162951535312, 1.000000000000000000, 0.9510565162951535312, 1.000000000000000000, 0.9510565162951535312, 1.000000000000000000, 0.9510565162951535312, 1.000000000000000000, 0.9510565162951535312, 1.000000000000000000, 0.9510565162951535312, 1.000000000000000000, 0.9510565162951535312, 1.000000000000000000, 0.9510565162951535312, 1.000000000000000000, 0.9510565162951535312, 1.000000000000000000, 0.9510565162951535312, 1.000000000000000000, 0.9510565162951535312, 1.000000000000000000, 0.9510565162951535312, 1.000000000000000000, 0.9510565162951535312, 1.000000000000000000, 0.9510565162951535312, 1.000000000000000000, 0.9510565162951535312, 1.000000000000000000, 0.9510565162951535312, 1.000000000000000000, 0.9510565162951535312, 1.000000000000000000, 0.9510565162951535312, 1.000000000000000000, 0.9510565162951535312, 1.000000000000000000, 0.9510565162951535312, 1.000000000000000000, 0.9510565162951535312, 1.000000000000000000, 0.9510565162951535312, 1.000000000000000000, 0.9510565162951535312, 1.000000000000000000, 0.9510565162951535312, 1.000000000000000000, 0.9510565162951535312, 1.000000000000000000, 0.9510565162951535312, 1.000000000000000000, 0.9510565162951535312, 1.000000000000000000, 0.9510565162951535312, 1.000000000000000000, 0.9510565162951535312, 1.000000000000000000, 0.9510565162951535312, 1.000000000000000000, 0.9510565162951535312, 1.000000000000000000, 0.9510565162951535312, 1.000000000000000000, 0.9510565162951535312, 1.000000000000000000, 0.9510565162951535312, 1.000000000000000000, 0.9510565162951535312, 1.000000000000000000, 0.9510565162951535312, 1.000000000000000000, 0.9510565162951535312, 1.000000000000000000, 0.9510565162951535312, 1.000000000000000000, 0.9510565162951535312, 1.000000000000000000, 0.9510565162951535312, 1.000000000000000000, 0.9510565162951535312, 1.000000000000000000, 0.9510565162951535312, 1.000000000000000000, 0.9510565162951535312, 1.000000000000000000, 0.9510565162951535312, 1.000000000000000000, 0.9510565162951535312, 1.000000000000000000, 0.9510565162951535312, 1.000000000000000000, 0.9510565162951535312, 1.000000000000000000, 0.9510565162951535312, 1.000000000000000000, 0.9510565162951535312, 1.000000000000000000, 0.9510565162951535312, 1.000000000000000000, 0.9510565162951535312, 1.000000000000000000, 0.9510565162951535312, 1.000000000000000000, 0.9510565162951535312, 1.000000000000000000, 0.9510565162951535312, 1.000000000000000000, 0.9510565162951535312, 1.000000000000000000, 0.9510565162951535312, 1.000000000000000000, 0.9510565162951535312, 1.000000000000000000, 0.9510565162951535312, 1.000000000000000000, 0.9510565162951535312, 1.000000000000000000, 0.9510565162951535312, 1.000000000000000000, 0.9510565162951535312, 1.000000000000000000, 0.9510565162951535312, 1.000000000000000000, 0.9510565162951535312, 1.000000000000000000, 0.9510565162951535312, 1.000000000000000000, 0.9510565162951535312, 1.000000000000000000, 0.9510565162951535312, 1.000000000000000000, 0.9510565162951535312, 1.000000000000000000, 0.9510565162951535312, 1.000000000000000000, 0.9510565162951535312, 1.000000000000000000, 0.9510565162951535312, 1.000000000000000000, 0.9510565162951535312, 1.000000000000000000, 0.9510565162951535312, 1.000000000000000000, 0.9510565162951535312, 1.000000000000000000, 0.9510565162951535312, 1.000000000000000000, 0.9510565162951535312, 1.000000000000000000, 0.9510565162951535312, 1.000000000000000000, 0.9510565162951535312, 1.000000000000000000, 0.9510565162951535312, 1.000000000000000000, 0.9510565162951535312, 1.000000000000000000, 0.9510565162951535312, 1.000000000000000000, 0.9510565162951535312, 1.000000000000000000, 0.9510565162951535312, 1.000000000000000000, 0.9510565162951535312, 1.000000000000000000, 0.9510565162951535312, 1.000000000000000000, 0.9510565162951535312, 1.000000000000000000, 0.9510565162951535312, 1.000000000000000000, 0.9510565162951535312, 1.000000000000000000, 0.9510565162951535312, 1.000000000000000000, 0.9510565162951535312, 1.000000000000000000, 0.9510565162951535312, 1.000000000000000000, 0.9573764855735550361, 0.9889922301674671790 ) ) 
 REPRESENTATION_ITEM ( '' )  );
#5964 = CARTESIAN_POINT ( 'NONE',  ( 8.118202686958039038, 212.8392687619912635, 82.70113791807857240 ) ) ;
#5965 = ORIENTED_EDGE ( 'NONE', *, *, #20724, .F. ) ;
#5966 = FACE_OUTER_BOUND ( 'NONE', #25364, .T. ) ;
#5967 = CARTESIAN_POINT ( 'NONE',  ( 0.2259792476677697226, -7.636022678937403718, -6.470294263593365791 ) ) ;
#5968 = ORIENTED_EDGE ( 'NONE', *, *, #10643, .F. ) ;
#5969 = CARTESIAN_POINT ( 'NONE',  ( 2.517493886308900919, 214.5937144450984420, 22.40113791807856813 ) ) ;
#5970 = ADVANCED_FACE ( 'NONE', ( #16403 ), #26030, .T. ) ;
#5971 = CARTESIAN_POINT ( 'NONE',  ( -59.60814253741918378, 194.9368883388851259, -2.246975524854183170 ) ) ;
#5972 = CARTESIAN_POINT ( 'NONE',  ( 0.05014649552828288198, 194.3824533091408000, 103.7488620819214304 ) ) ;
#5973 = CARTESIAN_POINT ( 'NONE',  ( 48.17499999726881299, 164.1591823560292198, 12.60653300113718167 ) ) ;
#5974 = EDGE_LOOP ( 'NONE', ( #14432, #4083, #28401, #9374, #13970, #33637, #21138 ) ) ;
#5975 = CARTESIAN_POINT ( 'NONE',  ( 60.32499999726881157, 145.8408176439707802, 12.60653300113718345 ) ) ;
#5976 = DIRECTION ( 'NONE',  ( 0.000000000000000000, -1.000000000000000000, 6.454785026890489601E-15 ) ) ;
#5977 = CARTESIAN_POINT ( 'NONE',  ( 92.60208470531341618, 155.0000000000000000, 0.000000000000000000 ) ) ;
#5978 = DIRECTION ( 'NONE',  ( 1.000000000000000000, -0.000000000000000000, -0.000000000000000000 ) ) ;
#5979 = CARTESIAN_POINT ( 'NONE',  ( 10.00000000000000711, 207.0476921513415220, 93.99886208192144466 ) ) ;
#5980 = CARTESIAN_POINT ( 'NONE',  ( 55.37499999726881583, 155.0000000000000000, -15.58253175000000823 ) ) ;
#5981 = CARTESIAN_POINT ( 'NONE',  ( -3.044812012440131443, 216.5253028482142952, 25.10113791807856742 ) ) ;
#5982 = FACE_OUTER_BOUND ( 'NONE', #23453, .T. ) ;
#5983 = EDGE_CURVE ( 'NONE', #8169, #8276, #19476, .T. ) ;
#5984 = CARTESIAN_POINT ( 'NONE',  ( 3.662846001189864698, 218.4274158808046593, 78.39886208192143613 ) ) ;
#5985 = VECTOR ( 'NONE', #2751, 1000.000000000000000 ) ;
#5986 = CARTESIAN_POINT ( 'NONE',  ( 73.79999999999999716, 142.6655632788954620, 8.961492836873471646 ) ) ;
#5987 = CARTESIAN_POINT ( 'NONE',  ( 40.78867513459481842, 155.0000000000000000, -15.00000000000002487 ) ) ;
#5988 = CARTESIAN_POINT ( 'NONE',  ( 125.5000000000000000, 155.0000000000000000, -6.938893903907228378E-15 ) ) ;
#5989 = CARTESIAN_POINT ( 'NONE',  ( -9.984503880673473830, 210.2968891136704315, 90.65113791807854682 ) ) ;
#5990 = CARTESIAN_POINT ( 'NONE',  ( 125.5000000000000000, 229.9533188057749555, 74.95331880577313655 ) ) ;
#5991 = CARTESIAN_POINT ( 'NONE',  ( 38.87499999726880873, 138.6155565068815463, -3.929120461958505118E-15 ) ) ;
#5992 = CARTESIAN_POINT ( 'NONE',  ( -3.135527875058821579, 197.5041725223112223, 38.90113791807857524 ) ) ;
#5993 = CARTESIAN_POINT ( 'NONE',  ( 78.02499999726879309, 160.0630714827496206, 15.58253174999999402 ) ) ;
#5994 = ADVANCED_FACE ( 'NONE', ( #10816 ), #6957, .F. ) ;
#5995 = ORIENTED_EDGE ( 'NONE', *, *, #5713, .T. ) ;
#5996 = DIRECTION ( 'NONE',  ( 1.000000000000000000, 0.000000000000000000, 0.000000000000000000 ) ) ;
#5997 = CARTESIAN_POINT ( 'NONE',  ( 43.79999999453762172, 146.4771138417591203, -11.73074641843674470 ) ) ;
#5998 = CARTESIAN_POINT ( 'NONE',  ( -3.753561863808691168, 195.6020594897209435, 23.90113791807857169 ) ) ;
#5999 = CARTESIAN_POINT ( 'NONE',  ( 40.41132485994280898, 167.7597621252805880, 9.270509831248428867 ) ) ;
#6000 = DIRECTION ( 'NONE',  ( 1.000000000000000000, 0.000000000000000000, 0.000000000000000000 ) ) ;
#6001 = ORIENTED_EDGE ( 'NONE', *, *, #12243, .F. ) ;
#6002 = CARTESIAN_POINT ( 'NONE',  ( -10.00000000000000711, 206.9523078486584495, 95.49886208192144466 ) ) ;
#6003 = CARTESIAN_POINT ( 'NONE',  ( 3.753561863808876797, 195.6020594897209719, 31.59886208192143187 ) ) ;
#6004 = DIRECTION ( 'NONE',  ( 0.000000000000000000, 0.000000000000000000, -1.000000000000000000 ) ) ;
#6005 = CARTESIAN_POINT ( 'NONE',  ( 3.044812012440130555, 197.4746971517856764, 47.60113791807857098 ) ) ;
#6006 = ORIENTED_EDGE ( 'NONE', *, *, #28033, .T. ) ;
#6007 = EDGE_CURVE ( 'NONE', #13631, #13221, #28196, .T. ) ;
#6008 = CARTESIAN_POINT ( 'NONE',  ( -4.903702542908436435, 200.1653181626580249, 14.04886208192143471 ) ) ;
#6009 = CARTESIAN_POINT ( 'NONE',  ( 70.78867513459482552, 155.0000000000000000, -15.00000000000002487 ) ) ;
#6010 = ORIENTED_EDGE ( 'NONE', *, *, #9130, .F. ) ;
#6011 = CARTESIAN_POINT ( 'NONE',  ( 6.444103211790928043, 211.7408657792734061, 102.6988620819214475 ) ) ;
#6012 = CARTESIAN_POINT ( 'NONE',  ( -8.015496119326531499, 204.4483345814780364, 42.35113791807857098 ) ) ;
#6013 = CARTESIAN_POINT ( 'NONE',  ( 3.499999999999999556, 0.000000000000000000, -2.899999999999999911 ) ) ;
#6014 = ORIENTED_EDGE ( 'NONE', *, *, #18714, .T. ) ;
#6015 = CARTESIAN_POINT ( 'NONE',  ( -62.70000000000000284, -88.00000000000000000, -20.00000000000000000 ) ) ;
#6016 = CARTESIAN_POINT ( 'NONE',  ( -6.220909254589682469, 215.4770327129946850, 50.94886208192141908 ) ) ;
#6017 = CARTESIAN_POINT ( 'NONE',  ( 33.87499999726881583, 171.3844434931184253, -7.942151717890132712E-15 ) ) ;
#6018 =( LENGTH_UNIT ( ) NAMED_UNIT ( * ) SI_UNIT ( .MILLI., .METRE. ) );
#6019 = CARTESIAN_POINT ( 'NONE',  ( 8.000000000000008882, 206.9523078486586485, 101.0011379180785696 ) ) ;
#6020 = CARTESIAN_POINT ( 'NONE',  ( 58.50000000000001421, -88.00000000000000000, 37.99999999999999289 ) ) ;
#6021 = CARTESIAN_POINT ( 'NONE',  ( 53.69999999999999574, 146.4771138417591203, 11.73074641843673227 ) ) ;
#6022 = CARTESIAN_POINT ( 'NONE',  ( -2.517493886309087880, 214.5937144450984135, 72.09886208192142476 ) ) ;
#6023 = DIRECTION ( 'NONE',  ( -0.08583835255247916629, -0.09953364313786493278, -0.9913247858874408847 ) ) ;
#6024 = CARTESIAN_POINT ( 'NONE',  ( 60.42499999726881299, 141.7447067706911810, 9.630534252274376428 ) ) ;
#6025 = CARTESIAN_POINT ( 'NONE',  ( -0.05014649552810635652, 196.4853777576173002, 11.75113791807856600 ) ) ;
#6026 = CARTESIAN_POINT ( 'NONE',  ( 115.4999999999999858, 63.20130719884917170, -52.99999999999946709 ) ) ;
#6027 = CONICAL_SURFACE ( 'NONE', #19101, 7.500000000000001776, 0.8594454914424796144 ) ;
#6028 = CARTESIAN_POINT ( 'NONE',  ( 65.82499999726883289, 168.2552932293087906, 9.630534252274372875 ) ) ;
#6029 = CARTESIAN_POINT ( 'NONE',  ( 75.97499999726881015, 169.8198683612136222, 4.815267126137181997 ) ) ;
#6030 = CARTESIAN_POINT ( 'NONE',  ( 12.00000000000000711, 206.9523078486586485, 80.00113791807856956 ) ) ;
#6031 = EDGE_CURVE ( 'NONE', #20901, #28279, #1530, .T. ) ;
#6032 = EDGE_CURVE ( 'NONE', #27878, #26666, #27144, .T. ) ;
#6033 = CARTESIAN_POINT ( 'NONE',  ( 3.135527875058820690, 216.4958274776887492, 97.40113791807858945 ) ) ;
#6034 = CARTESIAN_POINT ( 'NONE',  ( -10.34113947703223424, 207.9902438215976872, 102.7420191180251692 ) ) ;
#6035 = ORIENTED_EDGE ( 'NONE', *, *, #28476, .T. ) ;
#6036 = CARTESIAN_POINT ( 'NONE',  ( 7.375838497908012492, 217.2372850707501186, 102.5488620819214560 ) ) ;
#6037 = CARTESIAN_POINT ( 'NONE',  ( -12.00000000000000711, 206.9523078486584780, 59.49886208192143044 ) ) ;
#6038 = CARTESIAN_POINT ( 'NONE',  ( -0.05014649552828402690, 217.5146222423826714, 69.24886208192143044 ) ) ;
#6039 = CARTESIAN_POINT ( 'NONE',  ( -9.736236675708031640, 214.0148392665760753, 2.798862081921433820 ) ) ;
#6040 = DIRECTION ( 'NONE',  ( 0.000000000000000000, 0.000000000000000000, 1.000000000000000000 ) ) ;
#6041 = CARTESIAN_POINT ( 'NONE',  ( 3.044812012440130555, 197.4746971517856764, 26.60113791807856742 ) ) ;
#6042 = EDGE_CURVE ( 'NONE', #17930, #11179, #13495, .T. ) ;
#6043 = CARTESIAN_POINT ( 'NONE',  ( 10.00000000000000711, 207.0476921513415220, 90.99886208192144466 ) ) ;
#6044 = ORIENTED_EDGE ( 'NONE', *, *, #10231, .T. ) ;
#6045 = DIRECTION ( 'NONE',  ( 0.000000000000000000, 0.000000000000000000, 1.000000000000000000 ) ) ;
#6046 = ORIENTED_EDGE ( 'NONE', *, *, #19905, .F. ) ;
#6047 = DIRECTION ( 'NONE',  ( -1.000000000000000000, 0.000000000000000000, 0.000000000000000000 ) ) ;
#6048 = CARTESIAN_POINT ( 'NONE',  ( 6.500168698208244500, 202.3363017425938324, 58.29886208192143471 ) ) ;
#6049 = EDGE_CURVE ( 'NONE', #4673, #5750, #30358, .T. ) ;
#6050 = VERTEX_POINT ( 'NONE', #22358 ) ;
#6051 = CARTESIAN_POINT ( 'NONE',  ( 75.12499999726881583, 155.0000000000000000, -15.58253175000000823 ) ) ;
#6052 = ORIENTED_EDGE ( 'NONE', *, *, #8738, .F. ) ;
#6053 = CARTESIAN_POINT ( 'NONE',  ( -1.058054217398698871, 6.894685612232779981, -0.3576316571898437990 ) ) ;
#6054 = VECTOR ( 'NONE', #385, 1000.000000000000000 ) ;
#6055 = CARTESIAN_POINT ( 'NONE',  ( 68.82499999726880446, 141.7447067706911810, -9.630534252274385310 ) ) ;
#6056 = CARTESIAN_POINT ( 'NONE',  ( -0.05014649552807731031, 198.5883022060938572, 68.75113791807856956 ) ) ;
#6057 = FILL_AREA_STYLE ('',( #29407 ) ) ;
#6058 = CYLINDRICAL_SURFACE ( 'NONE', #19763, 3.399999999999999911 ) ;
#6059 = CARTESIAN_POINT ( 'NONE',  ( 37.59999999999999432, 150.2886644046228639, 14.49999999999999645 ) ) ;
#6060 = CARTESIAN_POINT ( 'NONE',  ( 4.903702542908435547, 213.8346818373419751, 45.54886208192144181 ) ) ;
#6061 = CARTESIAN_POINT ( 'NONE',  ( 3.135527875058820690, 216.4958274776887492, 82.40113791807857524 ) ) ;
#6062 = CARTESIAN_POINT ( 'NONE',  ( -3.044812012440131443, 216.5253028482142952, 70.10113791807857808 ) ) ;
#6063 = DIRECTION ( 'NONE',  ( 0.000000000000000000, 0.000000000000000000, -1.000000000000000000 ) ) ;
#6064 = CARTESIAN_POINT ( 'NONE',  ( -6.444103211791042618, 211.7408657792732356, 21.80113791807856671 ) ) ;
#6065 = CARTESIAN_POINT ( 'NONE',  ( 3.749999999999998224, 6.495190528383290918, -6.991905250253753756 ) ) ;
#6066 = CARTESIAN_POINT ( 'NONE',  ( 60.58867513459482979, 146.1832212156128890, -12.13525491562423042 ) ) ;
#6067 = CARTESIAN_POINT ( 'NONE',  ( 42.12499999726881583, 155.0000000000000000, 15.58253174999999402 ) ) ;
#6068 = CARTESIAN_POINT ( 'NONE',  ( -7.375838497908182134, 217.2372850707499765, 45.95113791807857950 ) ) ;
#6069 = DIRECTION ( 'NONE',  ( 0.8191520442889907994, 1.003171929053523514E-16, -0.5735764363510474917 ) ) ;
#6070 = CARTESIAN_POINT ( 'NONE',  ( -6.220909254589537696, 198.5229672870051161, 93.05113791807853829 ) ) ;
#6071 = CARTESIAN_POINT ( 'NONE',  ( -8.062137200540920645, 212.9164362838581894, 69.80113791807856671 ) ) ;
#6072 = CARTESIAN_POINT ( 'NONE',  ( -9.680171189290716072, 199.9079932115567146, 35.19886208192142618 ) ) ;
#6073 = CARTESIAN_POINT ( 'NONE',  ( 6.139770520408223575, 215.5359834540460611, 39.54886208192143471 ) ) ;
#6074 = CARTESIAN_POINT ( 'NONE',  ( 85.09999999453764019, 150.2886644046228639, 14.49999999999999645 ) ) ;
#6075 = CARTESIAN_POINT ( 'NONE',  ( 11.98450388067348271, 203.0532714938637753, 80.15113791807857524 ) ) ;
#6076 = CARTESIAN_POINT ( 'NONE',  ( -4.903702542908602524, 213.8346818373418898, 96.95113791807857240 ) ) ;
#6077 = CARTESIAN_POINT ( 'NONE',  ( -10.01549611932659722, 210.2015048109875011, 56.64886208192142902 ) ) ;
#6078 = CARTESIAN_POINT ( 'NONE',  ( 4.606548227981508425, 6.456511556909250160, -7.591235721156633254 ) ) ;
#6079 = ORIENTED_EDGE ( 'NONE', *, *, #26985, .T. ) ;
#6080 = CARTESIAN_POINT ( 'NONE',  ( 12.01549611932659367, 203.1486557965466773, 58.14886208192143613 ) ) ;
#6081 = CIRCLE ( 'NONE', #4442, 31.00000000000000000 ) ;
#6082 = ORIENTED_EDGE ( 'NONE', *, *, #235, .F. ) ;
#6083 = CARTESIAN_POINT ( 'NONE',  ( -4.903702542908436435, 200.1653181626580249, 35.04886208192144181 ) ) ;
#6084 = ORIENTED_EDGE ( 'NONE', *, *, #32854, .F. ) ;
#6085 = CARTESIAN_POINT ( 'NONE',  ( 78.97499999726881015, 140.1801316387863778, -4.815267126137194431 ) ) ;
#6086 = DIRECTION ( 'NONE',  ( 1.000000000000000000, 0.000000000000000000, 0.000000000000000000 ) ) ;
#6087 = DIRECTION ( 'NONE',  ( 1.000000000000000000, -0.000000000000000000, -0.000000000000000000 ) ) ;
#6088 = CARTESIAN_POINT ( 'NONE',  ( 8.000000000000008882, 206.9523078486586485, 47.00113791807856956 ) ) ;
#6089 = DIRECTION ( 'NONE',  ( 0.000000000000000000, 0.000000000000000000, -1.000000000000000000 ) ) ;
#6090 = CARTESIAN_POINT ( 'NONE',  ( -10.01549611932659722, 210.2015048109875011, 35.64886208192143613 ) ) ;
#6091 = CARTESIAN_POINT ( 'NONE',  ( 69.47499999726882436, 160.0630714827496206, -15.58253175000000823 ) ) ;
#6092 = ORIENTED_EDGE ( 'NONE', *, *, #16655, .T. ) ;
#6093 = CARTESIAN_POINT ( 'NONE',  ( 61.98867513459482836, 146.1832212156128890, 12.13525491562421976 ) ) ;
#6094 = AXIS2_PLACEMENT_3D ( 'NONE', #12114, #29375, #26805 ) ;
#6095 =( NAMED_UNIT ( * ) PLANE_ANGLE_UNIT ( ) SI_UNIT ( $, .RADIAN. ) );
#6096 = CARTESIAN_POINT ( 'NONE',  ( 52.18867513459482410, 140.7341522555726669, 4.635254915624211769 ) ) ;
#6097 = DIRECTION ( 'NONE',  ( -1.000000000000000000, -0.000000000000000000, -0.000000000000000000 ) ) ;
#6098 = CARTESIAN_POINT ( 'NONE',  ( 4.984841277089891776, 200.2242689037093726, 13.44886208192143684 ) ) ;
#6099 = CARTESIAN_POINT ( 'NONE',  ( 3.044812012440130555, 197.4746971517856764, 53.60113791807857098 ) ) ;
#6100 = DIRECTION ( 'NONE',  ( 1.000000000000000000, -0.000000000000000000, -0.000000000000000000 ) ) ;
#6101 = CARTESIAN_POINT ( 'NONE',  ( 8.062137200540920645, 201.0835637161417822, 41.30113791807857382 ) ) ;
#6102 = CARTESIAN_POINT ( 'NONE',  ( 83.57499999726880446, 164.1591823560292198, -12.60653300113719766 ) ) ;
#6103 = SHAPE_DEFINITION_REPRESENTATION ( #24933, #12832 ) ;
#6104 = CARTESIAN_POINT ( 'NONE',  ( 4.984841277089891776, 200.2242689037093726, 97.44886208192143329 ) ) ;
#6105 = VECTOR ( 'NONE', #18772, 1000.000000000000000 ) ;
#6106 = CARTESIAN_POINT ( 'NONE',  ( 40.92499999726881299, 145.8408176439707802, -12.60653300113719588 ) ) ;
#6107 = DIRECTION ( 'NONE',  ( 0.000000000000000000, 1.000000000000000000, 0.000000000000000000 ) ) ;
#6108 = DIRECTION ( 'NONE',  ( -0.9891821073486152249, -0.1466927349985428231, 0.000000000000000000 ) ) ;
#6109 = CARTESIAN_POINT ( 'NONE',  ( 7.456977232089302632, 217.1783343296989131, 16.55113791807857027 ) ) ;
#6110 = CARTESIAN_POINT ( 'NONE',  ( 1.249327701954825010, -8.410337540182549532, -7.776713651265369620 ) ) ;
#6111 = CARTESIAN_POINT ( 'NONE',  ( 60.57499999726881157, 145.8408176439707802, 12.60653300113718345 ) ) ;
#6112 = AXIS2_PLACEMENT_3D ( 'NONE', #22939, #14935, #9482 ) ;
#6113 = CARTESIAN_POINT ( 'NONE',  ( 9.984503880673470277, 203.7031108863295401, 62.15113791807856813 ) ) ;
#6114 = CARTESIAN_POINT ( 'NONE',  ( 3.044812012440130555, 197.4746971517856764, 38.60113791807857098 ) ) ;
#6115 = CARTESIAN_POINT ( 'NONE',  ( 0.3999999999999975797, 0.000000000000000000, 0.000000000000000000 ) ) ;
#6116 = DIRECTION ( 'NONE',  ( -1.000000000000000000, 0.000000000000000000, 0.000000000000000000 ) ) ;
#6117 = CARTESIAN_POINT ( 'NONE',  ( -0.05014649552828442242, 219.6175466908591716, 3.248862081921433997 ) ) ;
#6118 = CARTESIAN_POINT ( 'NONE',  ( -6.139770520408224463, 198.4640165459539105, 8.048862081921434708 ) ) ;
#6119 = CARTESIAN_POINT ( 'NONE',  ( 65.99999999453761745, 155.0000000000000000, -14.50000000000000711 ) ) ;
#6120 = EDGE_LOOP ( 'NONE', ( #24074, #20729, #30226, #21111 ) ) ;
#6121 = CARTESIAN_POINT ( 'NONE',  ( -0.05014649552807705357, 194.3824533091408000, 47.75113791807856245 ) ) ;
#6122 = CARTESIAN_POINT ( 'NONE',  ( -6.500168698208129925, 202.3363017425936050, 72.20113791807857240 ) ) ;
#6123 = LINE ( 'NONE', #25494, #21344 ) ;
#6124 = CARTESIAN_POINT ( 'NONE',  ( -6.220909254589682469, 215.4770327129946850, 20.94886208192143684 ) ) ;
#6125 = DIRECTION ( 'NONE',  ( 0.000000000000000000, 0.000000000000000000, 1.000000000000000000 ) ) ;
#6126 = EDGE_LOOP ( 'NONE', ( #14367, #2554, #28780 ) ) ;
#6127 = CARTESIAN_POINT ( 'NONE',  ( 8.062137200540920645, 201.0835637161417822, 80.30113791807858092 ) ) ;
#6128 = EDGE_LOOP ( 'NONE', ( #40, #27379, #2175, #1726 ) ) ;
#6129 = ADVANCED_FACE ( 'NONE', ( #24588 ), #31476, .T. ) ;
#6130 =( REPRESENTATION_RELATIONSHIP ('NONE','NONE', #25663, #32415 ) REPRESENTATION_RELATIONSHIP_WITH_TRANSFORMATION ( #10739 )SHAPE_REPRESENTATION_RELATIONSHIP( ) );
#6131 = DIRECTION ( 'NONE',  ( -0.000000000000000000, -0.000000000000000000, 1.000000000000000000 ) ) ;
#6132 = CARTESIAN_POINT ( 'NONE',  ( -1.649999999999999911, 2.020667218593133001E-16, 2.066666666667000385 ) ) ;
#6133 = ORIENTED_EDGE ( 'NONE', *, *, #32062, .F. ) ;
#6134 = AXIS2_PLACEMENT_3D ( 'NONE', #9099, #7064, #25108 ) ;
#6135 = CARTESIAN_POINT ( 'NONE',  ( -4.984841277089726574, 200.2242689037092305, 21.05113791807857027 ) ) ;
#6136 = VECTOR ( 'NONE', #28364, 1000.000000000000000 ) ;
#6137 = CARTESIAN_POINT ( 'NONE',  ( -58.50000000000002132, 194.9217985566782829, -2.500000000000000000 ) ) ;
#6138 = CARTESIAN_POINT ( 'NONE',  ( 10.00000000000000711, 207.0476921513415220, 6.998862081921434886 ) ) ;
#6139 = AXIS2_PLACEMENT_3D ( 'NONE', #21230, #9074, #31625 ) ;
#6140 = CARTESIAN_POINT ( 'NONE',  ( 47.77499999726881441, 169.8198683612136222, -4.815267126137197984 ) ) ;
#6141 = ORIENTED_EDGE ( 'NONE', *, *, #3918, .F. ) ;
#6142 = CARTESIAN_POINT ( 'NONE',  ( 56.92499999726881299, 145.8408176439707802, -12.60653300113719588 ) ) ;
#6143 = FACE_OUTER_BOUND ( 'NONE', #15317, .T. ) ;
#6144 = CYLINDRICAL_SURFACE ( 'NONE', #21582, 13.00000000000002487 ) ;
#6145 = FACE_OUTER_BOUND ( 'NONE', #2468, .T. ) ;
#6146 = CARTESIAN_POINT ( 'NONE',  ( 10.01549611932659545, 203.7984951890123853, 91.14886208192140771 ) ) ;
#6147 = CARTESIAN_POINT ( 'NONE',  ( 62.57499999726881867, 145.8408176439707802, 12.60653300113718345 ) ) ;
#6148 = CARTESIAN_POINT ( 'NONE',  ( 3.135527875058820690, 216.4958274776887492, 19.40113791807856813 ) ) ;
#6149 = DIRECTION ( 'NONE',  ( -0.000000000000000000, -0.000000000000000000, 1.000000000000000000 ) ) ;
#6150 = CARTESIAN_POINT ( 'NONE',  ( -3.753561863808878130, 218.3979405102790281, 75.09886208192142476 ) ) ;
#6151 = VECTOR ( 'NONE', #8100, 1000.000000000000000 ) ;
#6152 = CARTESIAN_POINT ( 'NONE',  ( 71.80000000000001137, 142.6655632788954620, 8.961492836873471646 ) ) ;
#6153 = CARTESIAN_POINT ( 'NONE',  ( 65.38867513459483405, 169.2658477444273331, 4.635254915624208216 ) ) ;
#6154 = DIRECTION ( 'NONE',  ( 0.000000000000000000, 0.000000000000000000, 1.000000000000000000 ) ) ;
#6155 = CARTESIAN_POINT ( 'NONE',  ( 8.118202686958039038, 212.8392687619912635, 91.70113791807857240 ) ) ;
#6156 = CARTESIAN_POINT ( 'NONE',  ( 33.08867513459482979, 167.7597621252805880, -9.270509831248443078 ) ) ;
#6157 = CARTESIAN_POINT ( 'NONE',  ( 42.47499999726880304, 149.9369285172503510, 15.58253174999999580 ) ) ;
#6158 = CARTESIAN_POINT ( 'NONE',  ( 3.044812012440130555, 197.4746971517856764, 35.60113791807857098 ) ) ;
#6159 = CARTESIAN_POINT ( 'NONE',  ( 78.72499999726881015, 140.1801316387863778, -4.815267126137194431 ) ) ;
#6160 = ORIENTED_EDGE ( 'NONE', *, *, #19153, .F. ) ;
#6161 = CARTESIAN_POINT ( 'NONE',  ( 48.21132485994281325, 170.7719333635740497, -7.904646289410545231E-15 ) ) ;
#6162 = AXIS2_PLACEMENT_3D ( 'NONE', #16045, #59, #8063 ) ;
#6163 = CARTESIAN_POINT ( 'NONE',  ( 38.29999999453762882, 167.3344367211045096, -8.961492836873482304 ) ) ;
#6164 =( BOUNDED_CURVE ( )  B_SPLINE_CURVE ( 2, ( #26716, #8179, #23833, #24169, #18564, #19224, #31999, #28949, #6093, #16491, #29621 ),
 .UNSPECIFIED., .F., .T. ) 
 B_SPLINE_CURVE_WITH_KNOTS ( ( 3, 2, 2, 2, 2, 3 ),
 ( 0.4464285714285712858, 0.4499999999999998446, 0.4535714285714284588, 0.4571428571428570176, 0.4607142857142856318, 0.4642857142857141906 ),
 .UNSPECIFIED. ) 
 CURVE ( )  GEOMETRIC_REPRESENTATION_ITEM ( )  RATIONAL_B_SPLINE_CURVE ( ( 1.000000000000001554, 0.9510565162951518658, 1.000000000000000000, 0.9510565162951534202, 1.000000000000000000, 0.9510565162951534202, 1.000000000000000000, 0.9510565162951534202, 1.000000000000000000, 0.9510565162951534202, 1.000000000000000000 ) ) 
 REPRESENTATION_ITEM ( '' )  );
#6165 = CARTESIAN_POINT ( 'NONE',  ( 12.00000000000000711, 206.9523078486586485, 23.00113791807856600 ) ) ;
#6166 = EDGE_CURVE ( 'NONE', #26131, #24999, #20581, .T. ) ;
#6167 = CIRCLE ( 'NONE', #12722, 5.000000000000001776 ) ;
#6168 = CARTESIAN_POINT ( 'NONE',  ( -58.50000000000001421, -88.00000000000000000, 20.00000000000000000 ) ) ;
#6169 = VECTOR ( 'NONE', #6516, 1000.000000000000000 ) ;
#6170 = CARTESIAN_POINT ( 'NONE',  ( -3.080866544137490504, -6.881514909249304424, -7.026396753507435200 ) ) ;
#6171 = ORIENTED_EDGE ( 'NONE', *, *, #31618, .F. ) ;
#6172 = CARTESIAN_POINT ( 'NONE',  ( -3.753561863808878130, 218.3979405102790281, 30.09886208192144252 ) ) ;
#6173 = DIRECTION ( 'NONE',  ( -0.000000000000000000, -0.000000000000000000, 1.000000000000000000 ) ) ;
#6174 = CARTESIAN_POINT ( 'NONE',  ( 6.139770520408368348, 198.4640165459539674, 53.45113791807855108 ) ) ;
#6175 = EDGE_LOOP ( 'NONE', ( #13013, #3911 ) ) ;
#6176 = CARTESIAN_POINT ( 'NONE',  ( -6.500168698208244500, 211.6636982574061676, 14.79886208192143471 ) ) ;
#6177 = EDGE_CURVE ( 'NONE', #26453, #17290, #17884, .T. ) ;
#6178 = AXIS2_PLACEMENT_3D ( 'NONE', #13035, #31270, #7931 ) ;
#6179 = CARTESIAN_POINT ( 'NONE',  ( 79.78867513459482552, 155.0000000000000000, 15.00000000000001243 ) ) ;
#6180 = EDGE_LOOP ( 'NONE', ( #24709, #24755, #27302 ) ) ;
#6182 = CARTESIAN_POINT ( 'NONE',  ( -4.903702542908436435, 200.1653181626580249, 98.04886208192144181 ) ) ;
#6181 =( GEOMETRIC_REPRESENTATION_CONTEXT ( 3 ) GLOBAL_UNCERTAINTY_ASSIGNED_CONTEXT ( ( #16903 ) ) GLOBAL_UNIT_ASSIGNED_CONTEXT ( ( #8959, #19524, #29408 ) ) REPRESENTATION_CONTEXT ( 'NONE', 'WORKASPACE' ) );
#6183 = CARTESIAN_POINT ( 'NONE',  ( 2.517493886308900919, 214.5937144450984420, 40.40113791807857524 ) ) ;
#6184 = CARTESIAN_POINT ( 'NONE',  ( 33.67499999726881299, 168.2552932293087906, -9.630534252274387086 ) ) ;
#6185 = VERTEX_POINT ( 'NONE', #11307 ) ;
#6186 = CARTESIAN_POINT ( 'NONE',  ( 35.42499999726880588, 168.2552932293087906, -9.630534252274385310 ) ) ;
#6187 = ADVANCED_FACE ( 'NONE', ( #14021 ), #9417, .T. ) ;
#6188 = AXIS2_PLACEMENT_3D ( 'NONE', #19777, #9222, #6662 ) ;
#6189 = CARTESIAN_POINT ( 'NONE',  ( -10.00000000000000711, 206.9523078486584495, 62.49886208192143755 ) ) ;
#6190 = AXIS2_PLACEMENT_3D ( 'NONE', #15158, #19761, #14650 ) ;
#6191 = CARTESIAN_POINT ( 'NONE',  ( 40.57499999726881157, 145.8408176439707802, 12.60653300113718345 ) ) ;
#6192 = CYLINDRICAL_SURFACE ( 'NONE', #12172, 2.500000000000000000 ) ;
#6193 = CARTESIAN_POINT ( 'NONE',  ( -4.903702542908602524, 213.8346818373418898, 99.95113791807860082 ) ) ;
#6194 = CARTESIAN_POINT ( 'NONE',  ( 56.30000000000000426, 146.4771138417591203, -11.73074641843674470 ) ) ;
#6195 = CARTESIAN_POINT ( 'NONE',  ( -4.984841277089891776, 213.7757310962905990, 74.94886208192143329 ) ) ;
#6196 = DIRECTION ( 'NONE',  ( 1.000000000000000000, 0.000000000000000000, 0.000000000000000000 ) ) ;
#6197 = ADVANCED_FACE ( 'NONE', ( #21854 ), #19812, .F. ) ;
#6198 = CARTESIAN_POINT ( 'NONE',  ( 57.02499999726882152, 149.9369285172503510, -15.58253175000000823 ) ) ;
#6199 = CARTESIAN_POINT ( 'NONE',  ( 3.044812012440130555, 197.4746971517856764, 8.601137918078565647 ) ) ;
#6200 = CYLINDRICAL_SURFACE ( 'NONE', #16792, 2.149999999999999023 ) ;
#6201 = CARTESIAN_POINT ( 'NONE',  ( 67.82499999726881867, 168.2552932293087906, 9.630534252274372875 ) ) ;
#6202 = CARTESIAN_POINT ( 'NONE',  ( 74.67499999726879878, 141.7447067706911810, 9.630534252274376428 ) ) ;
#6203 = CARTESIAN_POINT ( 'NONE',  ( 9.680171189290831535, 199.9079932115568852, 74.30113791807858092 ) ) ;
#6204 = ADVANCED_FACE ( 'NONE', ( #11973 ), #9163, .F. ) ;
#6205 = CARTESIAN_POINT ( 'NONE',  ( 8.118202686958039038, 212.8392687619912635, 94.70113791807857240 ) ) ;
#6206 = DIRECTION ( 'NONE',  ( 1.000000000000000000, 0.000000000000000000, 0.000000000000000000 ) ) ;
#6207 = VERTEX_POINT ( 'NONE', #14522 ) ;
#6208 = CARTESIAN_POINT ( 'NONE',  ( -6.139770520408224463, 198.4640165459539389, 5.048862081921435596 ) ) ;
#6209 = CARTESIAN_POINT ( 'NONE',  ( -7.456977232089471386, 217.1783343296987709, 59.94886208192143329 ) ) ;
#6210 = CARTESIAN_POINT ( 'NONE',  ( -3.135527875058982783, 216.4958274776886924, 66.09886208192143897 ) ) ;
#6211 = VECTOR ( 'NONE', #27403, 1000.000000000000000 ) ;
#6212 = CARTESIAN_POINT ( 'NONE',  ( 11.98450388067341876, 210.9467285061363953, 3.848862081921433642 ) ) ;
#6213 = CARTESIAN_POINT ( 'NONE',  ( 27.50000000000001066, -15.87713240271473580, -15.54379906938135214 ) ) ;
#6214 = CARTESIAN_POINT ( 'NONE',  ( -10.00000000000000711, 207.0476921513413515, 27.50113791807856600 ) ) ;
#6215 = AXIS2_PLACEMENT_3D ( 'NONE', #31991, #19049, #29438 ) ;
#6216 = CARTESIAN_POINT ( 'NONE',  ( -3.044812012439970683, 197.4746971517856196, 85.89886208192143613 ) ) ;
#6217 = ORIENTED_EDGE ( 'NONE', *, *, #19362, .T. ) ;
#6218 = CARTESIAN_POINT ( 'NONE',  ( 5.000000000000000000, -4.685197434473814759, 3.903127820947815962E-15 ) ) ;
#6219 = ORIENTED_EDGE ( 'NONE', *, *, #29106, .F. ) ;
#6220 = DIRECTION ( 'NONE',  ( 0.000000000000000000, 0.000000000000000000, -1.000000000000000000 ) ) ;
#6221 = CARTESIAN_POINT ( 'NONE',  ( -6.444103211790928043, 202.2591342207265939, 71.19886208192144750 ) ) ;
#6222 = VERTEX_POINT ( 'NONE', #6862 ) ;
#6223 = CARTESIAN_POINT ( 'NONE',  ( 85.82499999726879025, 168.2552932293087906, 9.630534252274372875 ) ) ;
#6224 = ORIENTED_EDGE ( 'NONE', *, *, #16821, .T. ) ;
#6225 = CARTESIAN_POINT ( 'NONE',  ( 69.11132485994281183, 140.7341522555726669, 4.635254915624211769 ) ) ;
#6226 = COLOUR_RGB ( '', 0.08235294, 0.09019608, 0.10196078) ;
#6227 = CARTESIAN_POINT ( 'NONE',  ( 71.92499999726881299, 164.1591823560292198, 12.60653300113718167 ) ) ;
#6228 = CARTESIAN_POINT ( 'NONE',  ( 6.500168698208129925, 211.6636982574063381, 64.70113791807857240 ) ) ;
#6229 = ADVANCED_FACE ( 'NONE', ( #908 ), #26572, .T. ) ;
#6230 = EDGE_CURVE ( 'NONE', #4391, #17930, #19504, .T. ) ;
#6231 = CYLINDRICAL_SURFACE ( 'NONE', #12692, 3.000000000000002665 ) ;
#6232 = CARTESIAN_POINT ( 'NONE',  ( 37.90000000000000568, 141.2096805137202580, 4.480746418436733158 ) ) ;
#6233 = CARTESIAN_POINT ( 'NONE',  ( -6.444103211790928043, 202.2591342207265939, 47.19886208192144750 ) ) ;
#6234 = CARTESIAN_POINT ( 'NONE',  ( 3.135527875058820690, 216.4958274776887492, 85.40113791807857524 ) ) ;
#6235 = PRODUCT_DEFINITION ( 'UNKNOWN', '', #7214, #9070 ) ;
#6236 = ADVANCED_FACE ( 'NONE', ( #24242 ), #5355, .F. ) ;
#6237 = CARTESIAN_POINT ( 'NONE',  ( 10.01549611932653860, 210.2015048109876716, 67.85113791807857808 ) ) ;
#6238 = DIRECTION ( 'NONE',  ( 0.000000000000000000, 0.000000000000000000, 1.000000000000000000 ) ) ;
#6239 = CARTESIAN_POINT ( 'NONE',  ( 4.984841277089725686, 213.7757310962907411, 22.55113791807857027 ) ) ;
#6240 = CYLINDRICAL_SURFACE ( 'NONE', #467, 4.250000000000000000 ) ;
#6241 = CARTESIAN_POINT ( 'NONE',  ( -6.725979247667768668, 3.622307570260310694, -6.470294263593358686 ) ) ;
#6242 = CARTESIAN_POINT ( 'NONE',  ( 41.72499999726881015, 169.8198683612136222, 4.815267126137181997 ) ) ;
#6243 = CARTESIAN_POINT ( 'NONE',  ( -0.05014649552807705357, 194.3824533091408000, 47.75113791807856245 ) ) ;
#6244 = CARTESIAN_POINT ( 'NONE',  ( 7.500000000000000000, -3.202733125947433201, -7.213074474936314928 ) ) ;
#6245 = ADVANCED_FACE ( 'NONE', ( #22193 ), #32582, .F. ) ;
#6246 = CARTESIAN_POINT ( 'NONE',  ( -8.062137200540920645, 212.9164362838581894, 90.80113791807858092 ) ) ;
#6247 = CARTESIAN_POINT ( 'NONE',  ( -8.062137200540920645, 212.9164362838581894, 72.80113791807856671 ) ) ;
#6248 = CARTESIAN_POINT ( 'NONE',  ( 9.680171189290716072, 214.0920067884432854, 36.69886208192142618 ) ) ;
#6249 = CARTESIAN_POINT ( 'NONE',  ( 0.05014649552828275014, 196.4853777576173002, 40.74886208192143044 ) ) ;
#6250 = CARTESIAN_POINT ( 'NONE',  ( 88.79999999453764303, 163.5228861582408797, 11.73074641843673049 ) ) ;
#6251 = CARTESIAN_POINT ( 'NONE',  ( -9.736236675707914401, 199.9851607334237542, 78.20113791807857240 ) ) ;
#6252 = CARTESIAN_POINT ( 'NONE',  ( -7.898309971686851227, 224.1054302408387287, 103.4854814124441447 ) ) ;
#6253 = CARTESIAN_POINT ( 'NONE',  ( -6.139770520408224463, 198.4640165459539389, 59.04886208192143471 ) ) ;
#6254 = SURFACE_STYLE_FILL_AREA ( #3530 ) ;
#6255 = ORIENTED_EDGE ( 'NONE', *, *, #2441, .T. ) ;
#6256 = CARTESIAN_POINT ( 'NONE',  ( -7.375838497908014268, 196.7627149292498530, 65.04886208192144181 ) ) ;
#6257 = ORIENTED_EDGE ( 'NONE', *, *, #29497, .T. ) ;
#6258 = CARTESIAN_POINT ( 'NONE',  ( 73.17499999726881299, 145.8408176439707802, -12.60653300113719588 ) ) ;
#6259 = CARTESIAN_POINT ( 'NONE',  ( -6.500168698208244500, 211.6636982574061676, 41.79886208192144181 ) ) ;
#6260 = ORIENTED_EDGE ( 'NONE', *, *, #31980, .F. ) ;
#6261 = CARTESIAN_POINT ( 'NONE',  ( 79.37499999726881583, 155.0000000000000000, -15.58253175000000823 ) ) ;
#6262 = CARTESIAN_POINT ( 'NONE',  ( 2.000000000000000000, -1.877893248421449134E-15, -1.535500000000000087 ) ) ;
#6263 = DIRECTION ( 'NONE',  ( 0.000000000000000000, 0.000000000000000000, -1.000000000000000000 ) ) ;
#6264 = CARTESIAN_POINT ( 'NONE',  ( 7.984503880673485376, 204.3529502787953902, 50.15113791807857524 ) ) ;
#6265 = EDGE_CURVE ( 'NONE', #28846, #9319, #9648, .T. ) ;
#6266 = CARTESIAN_POINT ( 'NONE',  ( 10.01549611932659545, 203.7984951890123853, 31.14886208192142902 ) ) ;
#6267 = CARTESIAN_POINT ( 'NONE',  ( 70.07499999726881867, 168.2552932293087906, 9.630534252274372875 ) ) ;
#6268 = ORIENTED_EDGE ( 'NONE', *, *, #33328, .F. ) ;
#6269 = CARTESIAN_POINT ( 'NONE',  ( 68.18867513459483121, 140.7341522555726669, 4.635254915624211769 ) ) ;
#6270 = CARTESIAN_POINT ( 'NONE',  ( 117.5000000000000000, 127.5651812191323557, -102.3881375866411645 ) ) ;
#6271 = CARTESIAN_POINT ( 'NONE',  ( 43.38867513459481984, 169.2658477444273331, 4.635254915624208216 ) ) ;
#6272 = CARTESIAN_POINT ( 'NONE',  ( -8.015496119326597224, 209.5516654185217362, 11.64886208192143613 ) ) ;
#6273 = CARTESIAN_POINT ( 'NONE',  ( 10.00000000000000711, 206.9523078486586201, 50.00113791807856956 ) ) ;
#6274 = PRODUCT_DEFINITION_SHAPE ( 'NONE', 'NONE',  #33699 ) ;
#6275 = CARTESIAN_POINT ( 'NONE',  ( -8.118202686958039038, 201.1607312380087080, 36.20113791807857240 ) ) ;
#6276 = CARTESIAN_POINT ( 'NONE',  ( 85.67499999726879878, 168.2552932293087906, -9.630534252274385310 ) ) ;
#6277 = CARTESIAN_POINT ( 'NONE',  ( -2.426778023690076225, 199.3768101843759553, 100.8988620819214361 ) ) ;
#6278 = CARTESIAN_POINT ( 'NONE',  ( 43.52499999726881441, 169.8198683612136222, -4.815267126137197984 ) ) ;
#6279 = CARTESIAN_POINT ( 'NONE',  ( -64.50000000000000000, -2.605762844159085212, 20.00000000000000000 ) ) ;
#6280 = DIRECTION ( 'NONE',  ( 0.000000000000000000, 1.000000000000000000, -1.295896757998781572E-15 ) ) ;
#6281 = CARTESIAN_POINT ( 'NONE',  ( 12.01549611932652972, 210.8513442034534933, 22.85113791807856742 ) ) ;
#6282 = DIRECTION ( 'NONE',  ( 0.000000000000000000, 0.000000000000000000, 1.000000000000000000 ) ) ;
#6283 = CARTESIAN_POINT ( 'NONE',  ( -9.984503880673473830, 210.2968891136704315, 69.65113791807854682 ) ) ;
#6284 = CARTESIAN_POINT ( 'NONE',  ( 8.118202686958039038, 212.8392687619912635, 43.70113791807857240 ) ) ;
#6285 = DIRECTION ( 'NONE',  ( -0.8191520442889923537, 1.003171929053525363E-16, 0.5735764363510453823 ) ) ;
#6286 = CARTESIAN_POINT ( 'NONE',  ( 10.40000000000000036, 6.613092715395709439E-16, 5.400000000000002132 ) ) ;
#6287 = CARTESIAN_POINT ( 'NONE',  ( 0.05014649552828288198, 194.3824533091408000, 4.748862081921433109 ) ) ;
#6288 = CARTESIAN_POINT ( 'NONE',  ( -10.00000000000000711, 206.9523078486584495, 8.498862081921433997 ) ) ;
#6289 = CARTESIAN_POINT ( 'NONE',  ( 67.19999999453763451, 146.4771138417591203, 11.73074641843673227 ) ) ;
#6290 = VERTEX_POINT ( 'NONE', #31317 ) ;
#6291 = CARTESIAN_POINT ( 'NONE',  ( -11.98450388067348804, 210.9467285061362247, 45.65113791807856813 ) ) ;
#6292 = CARTESIAN_POINT ( 'NONE',  ( 6.444103211791042618, 202.2591342207267644, 71.30113791807856671 ) ) ;
#6293 = LINE ( 'NONE', #24531, #1236 ) ;
#6294 = CARTESIAN_POINT ( 'NONE',  ( 10.01549611932659545, 203.7984951890123853, 31.14886208192142902 ) ) ;
#6295 = CARTESIAN_POINT ( 'NONE',  ( 5.450967621166010524, -4.358435876041012236, -0.3607371497494579193 ) ) ;
#6296 = ORIENTED_EDGE ( 'NONE', *, *, #2261, .T. ) ;
#6297 = CARTESIAN_POINT ( 'NONE',  ( -8.062137200540920645, 212.9164362838581894, 78.80113791807858092 ) ) ;
#6298 = VERTEX_POINT ( 'NONE', #18367 ) ;
#6299 = B_SPLINE_CURVE_WITH_KNOTS ( 'NONE', 3,
 ( #1910, #22345, #6683, #32397, #14179, #9566 ),
 .UNSPECIFIED., .F., .F.,
 ( 4, 2, 4 ),
 ( -6.634491363447954936E-06, 0.0006892677013496626174, 0.001385169894062773148 ),
 .UNSPECIFIED. ) ;
#6300 = CARTESIAN_POINT ( 'NONE',  ( -2.428571428571428381, 2.974142226500714333E-16, 9.480888224575629408 ) ) ;
#6301 = CARTESIAN_POINT ( 'NONE',  ( -2.055025722541619970, -6.319083845364135144, -5.720331885005373707 ) ) ;
#6302 = ORIENTED_EDGE ( 'NONE', *, *, #19789, .T. ) ;
#6303 = CARTESIAN_POINT ( 'NONE',  ( 6.500168698208129925, 211.6636982574063381, 25.70113791807857240 ) ) ;
#6304 =( BOUNDED_CURVE ( )  B_SPLINE_CURVE ( 2, ( #29962, #6961, #6618, #17003, #17175, #14450, #24844, #1507, #33486, #11905, #22291 ),
 .UNSPECIFIED., .F., .F. ) 
 B_SPLINE_CURVE_WITH_KNOTS ( ( 3, 2, 2, 2, 2, 3 ),
 ( 0.6607142857142856984, 0.6642857142857142572, 0.6678571428571428159, 0.6714285714285712636, 0.6749999999999999334, 0.6785714285714284921 ),
 .UNSPECIFIED. ) 
 CURVE ( )  GEOMETRIC_REPRESENTATION_ITEM ( )  RATIONAL_B_SPLINE_CURVE ( ( 1.000000000000000000, 0.9510565162951534202, 1.000000000000000000, 0.9510565162951534202, 1.000000000000000000, 0.9510565162951534202, 1.000000000000000000, 0.9510565162951534202, 1.000000000000000000, 0.9510565162951549745, 0.9999999999999984457 ) ) 
 REPRESENTATION_ITEM ( '' )  );
#6305 = CARTESIAN_POINT ( 'NONE',  ( -60.99994150909498103, 194.9999963443187028, 0.1639972282098350886 ) ) ;
#6306 = CARTESIAN_POINT ( 'NONE',  ( -8.062137200540822946, 201.0835637161416400, 8.198862081921435063 ) ) ;
#6307 = CARTESIAN_POINT ( 'NONE',  ( 49.07499999726881157, 141.7447067706911810, -9.630534252274387086 ) ) ;
#6308 = ORIENTED_EDGE ( 'NONE', *, *, #18720, .T. ) ;
#6309 = CARTESIAN_POINT ( 'NONE',  ( 59.02499999726880731, 149.9369285172503510, -15.58253175000000823 ) ) ;
#6310 = CARTESIAN_POINT ( 'NONE',  ( -6.500168698208129925, 202.3363017425936050, 51.20113791807857240 ) ) ;
#6311 = CARTESIAN_POINT ( 'NONE',  ( 60.78867513459481842, 155.0000000000000000, -15.00000000000002487 ) ) ;
#6312 =( NAMED_UNIT ( * ) PLANE_ANGLE_UNIT ( ) SI_UNIT ( $, .RADIAN. ) );
#6313 = DIRECTION ( 'NONE',  ( 1.224646799147353207E-16, 1.000000000000000000, 0.000000000000000000 ) ) ;
#6314 = CARTESIAN_POINT ( 'NONE',  ( -10.01549611932659722, 210.2015048109875011, 86.64886208192139350 ) ) ;
#6315 = CARTESIAN_POINT ( 'NONE',  ( 61.47499999726879594, 160.0630714827496206, -15.58253175000000823 ) ) ;
#6316 = CARTESIAN_POINT ( 'NONE',  ( -3.044812012440131443, 216.5253028482142952, 22.10113791807856742 ) ) ;
#6317 = DIRECTION ( 'NONE',  ( -0.000000000000000000, -0.000000000000000000, 1.000000000000000000 ) ) ;
#6318 = CARTESIAN_POINT ( 'NONE',  ( 7.456977232089471386, 196.8216656703012006, 82.44886208192144750 ) ) ;
#6319 = CIRCLE ( 'NONE', #17271, 2.149999999999985256 ) ;
#6320 = AXIS2_PLACEMENT_3D ( 'NONE', #4506, #33300, #30411 ) ;
#6321 = CARTESIAN_POINT ( 'NONE',  ( 75.60000000000000853, 150.2886644046228639, 14.49999999999999645 ) ) ;
#6322 = CARTESIAN_POINT ( 'NONE',  ( 40.08867513459482979, 142.2402378747194405, 9.270509831248432420 ) ) ;
#6323 = FACE_OUTER_BOUND ( 'NONE', #3081, .T. ) ;
#6324 = CARTESIAN_POINT ( 'NONE',  ( -0.05014649552810635652, 196.4853777576173002, 92.75113791807858377 ) ) ;
#6325 = FACE_OUTER_BOUND ( 'NONE', #2508, .T. ) ;
#6326 = CARTESIAN_POINT ( 'NONE',  ( 44.47499999726879594, 149.9369285172503510, 15.58253174999999580 ) ) ;
#6327 = CARTESIAN_POINT ( 'NONE',  ( 3.135527875058820690, 216.4958274776887492, 37.40113791807857524 ) ) ;
#6328 = EDGE_CURVE ( 'NONE', #5021, #20942, #4817, .T. ) ;
#6329 = AXIS2_PLACEMENT_3D ( 'NONE', #18023, #295, #13239 ) ;
#6330 = CARTESIAN_POINT ( 'NONE',  ( 76.32499999726881867, 145.8408176439707802, 12.60653300113718345 ) ) ;
#6331 = ORIENTED_EDGE ( 'NONE', *, *, #15102, .T. ) ;
#6332 = CARTESIAN_POINT ( 'NONE',  ( 51.81132485994281467, 159.8737954434937478, -14.99999999999993072 ) ) ;
#6333 = CARTESIAN_POINT ( 'NONE',  ( 47.19999999453762740, 146.4771138417591203, 11.73074641843673227 ) ) ;
#6334 = B_SPLINE_CURVE_WITH_KNOTS ( 'NONE', 3,
 ( #29037, #32089, #11150, #8752, #26803 ),
 .UNSPECIFIED., .F., .F.,
 ( 4, 1, 4 ),
 ( 0.000000000000000000, 0.003752776749732568765, 0.007505553499465137529 ),
 .UNSPECIFIED. ) ;
#6335 = CARTESIAN_POINT ( 'NONE',  ( 7.456977232089302632, 217.1783343296989131, 22.55113791807857027 ) ) ;
#6336 = CARTESIAN_POINT ( 'NONE',  ( -68.50000000000000000, 215.0000000000000000, 2.500000000000000000 ) ) ;
#6337 = DIRECTION ( 'NONE',  ( 1.000000000000000000, -0.000000000000000000, -0.000000000000000000 ) ) ;
#6338 = VERTEX_POINT ( 'NONE', #26038 ) ;
#6339 = CARTESIAN_POINT ( 'NONE',  ( -3.662846001189865142, 195.5725841191952838, 37.89886208192143613 ) ) ;
#6340 = CARTESIAN_POINT ( 'NONE',  ( 85.78867513459481131, 155.0000000000000000, 15.00000000000001243 ) ) ;
#6341 = CARTESIAN_POINT ( 'NONE',  ( -10.00000000000000711, 207.0476921513413515, 54.50113791807857666 ) ) ;
#6342 = VERTEX_POINT ( 'NONE', #18449 ) ;
#6343 = CARTESIAN_POINT ( 'NONE',  ( -2.517493886309087880, 214.5937144450984135, 18.09886208192143187 ) ) ;
#6344 = VECTOR ( 'NONE', #19458, 1000.000000000000000 ) ;
#6345 = AXIS2_PLACEMENT_3D ( 'NONE', #17892, #15161, #25554 ) ;
#6346 = UNCERTAINTY_MEASURE_WITH_UNIT (LENGTH_MEASURE( 1.000000000000000082E-05 ), #32798, 'distance_accuracy_value', 'NONE');
#6347 = CARTESIAN_POINT ( 'NONE',  ( 50.38867513459482694, 140.7341522555726669, -4.635254915624220651 ) ) ;
#6348 = ORIENTED_EDGE ( 'NONE', *, *, #5938, .F. ) ;
#6349 = CARTESIAN_POINT ( 'NONE',  ( 8.015496119326595448, 204.4483345814782638, 103.1488620819214361 ) ) ;
#6350 = CARTESIAN_POINT ( 'NONE',  ( -119.7500000000000000, -6.429395695523609083E-16, 35.00000599999999906 ) ) ;
#6351 = CARTESIAN_POINT ( 'NONE',  ( 8.015496119326531499, 209.5516654185219636, 43.85113791807856387 ) ) ;
#6352 = CARTESIAN_POINT ( 'NONE',  ( 32.50000000000000000, 155.0000000000000000, -6.938893903907228378E-15 ) ) ;
#6354 = ORIENTED_EDGE ( 'NONE', *, *, #1670, .F. ) ;
#6353 = AXIS2_PLACEMENT_3D ( 'NONE', #18148, #7081, #25470 ) ;
#6355 = CARTESIAN_POINT ( 'NONE',  ( 40.52499999726881441, 140.1801316387863778, 4.815267126137185549 ) ) ;
#6356 = CARTESIAN_POINT ( 'NONE',  ( 3.044812012439969795, 216.5253028482143520, 57.39886208192143613 ) ) ;
#6357 = CARTESIAN_POINT ( 'NONE',  ( 43.07499999726881157, 141.7447067706911810, -9.630534252274385310 ) ) ;
#6358 = CARTESIAN_POINT ( 'NONE',  ( 1.517883041479706208E-15, 4.041451884327390331, -0.3126073911696551910 ) ) ;
#6359 = CARTESIAN_POINT ( 'NONE',  ( -8.015496119326531499, 204.4483345814780364, 96.35113791807857808 ) ) ;
#6360 = CARTESIAN_POINT ( 'NONE',  ( 53.40000000000000568, 159.7113355953771077, 14.49999999999999289 ) ) ;
#6361 = DIRECTION ( 'NONE',  ( -0.000000000000000000, -0.000000000000000000, 1.000000000000000000 ) ) ;
#6362 = CARTESIAN_POINT ( 'NONE',  ( 2.517493886309087436, 199.4062855549015865, 70.59886208192142476 ) ) ;
#6363 = AXIS2_PLACEMENT_3D ( 'NONE', #11164, #8600, #24099 ) ;
#6364 = DIRECTION ( 'NONE',  ( 0.000000000000000000, 0.000000000000000000, -1.000000000000000000 ) ) ;
#6365 = DIRECTION ( 'NONE',  ( 0.000000000000000000, 0.000000000000000000, 1.000000000000000000 ) ) ;
#6366 = EDGE_CURVE ( 'NONE', #22231, #23387, #20610, .T. ) ;
#6367 =( GEOMETRIC_REPRESENTATION_CONTEXT ( 3 ) GLOBAL_UNCERTAINTY_ASSIGNED_CONTEXT ( ( #21558 ) ) GLOBAL_UNIT_ASSIGNED_CONTEXT ( ( #32821, #27538, #27373 ) ) REPRESENTATION_CONTEXT ( 'NONE', 'WORKASPACE' ) );
#6368 = B_SPLINE_CURVE_WITH_KNOTS ( 'NONE', 3,
 ( #33060, #12116, #1894, #7008, #17221, #30345, #22164, #17394, #24732, #1386, #19616, #27608, #14668, #1716, #22507, #27780, #4444, #25231, #9729, #14832, #30512, #5125, #23681, #10419, #18409, #15844, #4958, #8024, #20791, #341 ),
 .UNSPECIFIED., .F., .F.,
 ( 4, 2, 2, 2, 2, 2, 2, 2, 2, 2, 2, 2, 2, 2, 4 ),
 ( 0.007818044621537994371, 0.008306560441632113850, 0.008795076261726231595, 0.009772107901914449737, 0.01026062372200855187, 0.01074913954210265227, 0.01123765536219675440, 0.01172617118229085653, 0.01221468700238495693, 0.01270320282247905906, 0.01319171864257315946, 0.01368023446266726159, 0.01416875028276136372, 0.01465726610285546412, 0.01563429774304366665 ),
 .UNSPECIFIED. ) ;
#6369 = CARTESIAN_POINT ( 'NONE',  ( 54.72499999726881015, 140.1801316387863778, -4.815267126137194431 ) ) ;
#6370 =( GEOMETRIC_REPRESENTATION_CONTEXT ( 3 ) GLOBAL_UNCERTAINTY_ASSIGNED_CONTEXT ( ( #26674 ) ) GLOBAL_UNIT_ASSIGNED_CONTEXT ( ( #27550, #14270, #1333 ) ) REPRESENTATION_CONTEXT ( 'NONE', 'WORKASPACE' ) );
#6372 = ORIENTED_EDGE ( 'NONE', *, *, #16423, .T. ) ;
#6371 = CARTESIAN_POINT ( 'NONE',  ( 10.00000000000000711, 206.9523078486586201, 17.00113791807856600 ) ) ;
#6373 = CARTESIAN_POINT ( 'NONE',  ( -12.58016597185465280, 24.49110259512896448, -0.01440555954223410491 ) ) ;
#6374 = CARTESIAN_POINT ( 'NONE',  ( 81.27499999726877888, 149.9369285172503510, -15.58253175000000823 ) ) ;
#6375 = CARTESIAN_POINT ( 'NONE',  ( -11.98450388067348804, 210.9467285061362247, 81.65113791807856103 ) ) ;
#6376 = EDGE_CURVE ( 'NONE', #33389, #20431, #32554, .T. ) ;
#6377 = CARTESIAN_POINT ( 'NONE',  ( -8.118202686958039038, 201.1607312380087080, 96.20113791807857240 ) ) ;
#6378 = DIRECTION ( 'NONE',  ( 0.000000000000000000, 0.000000000000000000, 1.000000000000000000 ) ) ;
#6379 = VECTOR ( 'NONE', #10462, 1000.000000000000000 ) ;
#6380 = EDGE_CURVE ( 'NONE', #23586, #19626, #25692, .T. ) ;
#6381 = VERTEX_POINT ( 'NONE', #31146 ) ;
#6382 = CARTESIAN_POINT ( 'NONE',  ( -3.135527875058982783, 216.4958274776886924, 3.098862081921434974 ) ) ;
#6383 = CARTESIAN_POINT ( 'NONE',  ( 11.98450388067341876, 210.9467285061363953, 60.84886208192143187 ) ) ;
#6384 = CARTESIAN_POINT ( 'NONE',  ( 8.062137200540822946, 212.9164362838583315, 78.69886208192143329 ) ) ;
#6385 = CARTESIAN_POINT ( 'NONE',  ( -7.375838497908014268, 196.7627149292498530, 2.048862081921434264 ) ) ;
#6386 = DIRECTION ( 'NONE',  ( 0.000000000000000000, -0.4999999999999990563, 0.8660254037844391517 ) ) ;
#6387 = CARTESIAN_POINT ( 'NONE',  ( 3.044812012440130555, 197.4746971517856764, 20.60113791807856742 ) ) ;
#6388 = CARTESIAN_POINT ( 'NONE',  ( -8.118202686958138514, 212.8392687619910930, 92.79886208192144181 ) ) ;
#6389 = ORIENTED_EDGE ( 'NONE', *, *, #25989, .F. ) ;
#6390 = EDGE_CURVE ( 'NONE', #9889, #6511, #33667, .T. ) ;
#6391 = CARTESIAN_POINT ( 'NONE',  ( -65.20000000000000284, -7.347880794884118356E-15, -19.30000000000003979 ) ) ;
#6392 = ORIENTED_EDGE ( 'NONE', *, *, #9785, .F. ) ;
#6393 = LINE ( 'NONE', #11510, #11291 ) ;
#6394 = CARTESIAN_POINT ( 'NONE',  ( -2.426778023690076225, 199.3768101843759553, 67.89886208192143613 ) ) ;
#6395 = AXIS2_PLACEMENT_3D ( 'NONE', #20064, #14274, #21943 ) ;
#6396 = EDGE_LOOP ( 'NONE', ( #12689, #1942, #23086, #31010 ) ) ;
#6397 = AXIS2_PLACEMENT_3D ( 'NONE', #14057, #19512, #24272 ) ;
#6398 = CARTESIAN_POINT ( 'NONE',  ( 81.52499999726880731, 169.8198683612136222, -4.815267126137197984 ) ) ;
#6399 = ORIENTED_EDGE ( 'NONE', *, *, #22723, .T. ) ;
#6400 = DIRECTION ( 'NONE',  ( -1.000000000000000000, 0.000000000000000000, 0.000000000000000000 ) ) ;
#6401 = VECTOR ( 'NONE', #11857, 1000.000000000000000 ) ;
#6402 = EDGE_CURVE ( 'NONE', #20607, #14989, #13873, .T. ) ;
#6403 = CONICAL_SURFACE ( 'NONE', #4856, 12.00000000000001066, 0.1047197551196174109 ) ;
#6404 = CARTESIAN_POINT ( 'NONE',  ( 74.92499999726881299, 145.8408176439707802, -12.60653300113719588 ) ) ;
#6405 = CARTESIAN_POINT ( 'NONE',  ( 4.903702542908601636, 200.1653181626581102, 71.45113791807854398 ) ) ;
#6406 = FACE_OUTER_BOUND ( 'NONE', #19328, .T. ) ;
#6407 = AXIS2_PLACEMENT_3D ( 'NONE', #12795, #15683, #18246 ) ;
#6408 =( NAMED_UNIT ( * ) PLANE_ANGLE_UNIT ( ) SI_UNIT ( $, .RADIAN. ) );
#6409 = CARTESIAN_POINT ( 'NONE',  ( 38.29999999999999716, 146.4771138417591203, -11.73074641843674470 ) ) ;
#6410 = CARTESIAN_POINT ( 'NONE',  ( -6.500168698208244500, 211.6636982574061676, 47.79886208192144181 ) ) ;
#6411 = CARTESIAN_POINT ( 'NONE',  ( 3.044812012440130555, 197.4746971517856764, 89.60113791807857808 ) ) ;
#6412 = CARTESIAN_POINT ( 'NONE',  ( -6.220909254589537696, 198.5229672870051161, 78.05113791807858092 ) ) ;
#6413 = EDGE_CURVE ( 'NONE', #9970, #8044, #12037, .T. ) ;
#6414 = FACE_OUTER_BOUND ( 'NONE', #3547, .T. ) ;
#6415 = CARTESIAN_POINT ( 'NONE',  ( 129.1982509225904039, -3.226370279868275404, 35.00001200000000523 ) ) ;
#6416 = DIRECTION ( 'NONE',  ( 1.000000000000000000, 0.000000000000000000, 0.000000000000000000 ) ) ;
#6417 = CARTESIAN_POINT ( 'NONE',  ( 50.42499999726880588, 141.7447067706911810, 9.630534252274376428 ) ) ;
#6418 = CARTESIAN_POINT ( 'NONE',  ( 12.00000000000000711, 206.9523078486586485, 47.00113791807856956 ) ) ;
#6419 = CARTESIAN_POINT ( 'NONE',  ( -129.1982509225904892, -3.226370279868305602, 35.00001200000000523 ) ) ;
#6420 = AXIS2_PLACEMENT_3D ( 'NONE', #11146, #23590, #13679 ) ;
#6421 = PRODUCT_DEFINITION_SHAPE ( 'NONE', 'NONE',  #29780 ) ;
#6422 = CARTESIAN_POINT ( 'NONE',  ( 6.139770520408368348, 198.4640165459539674, 95.45113791807855819 ) ) ;
#6423 = CARTESIAN_POINT ( 'NONE',  ( -6.139770520408368348, 215.5359834540460042, 72.95113791807855819 ) ) ;
#6424 = AXIS2_PLACEMENT_3D ( 'NONE', #26924, #14143, #32036 ) ;
#6425 = CARTESIAN_POINT ( 'NONE',  ( 9.680171189290716072, 214.0920067884432854, 30.69886208192143684 ) ) ;
#6426 = CARTESIAN_POINT ( 'NONE',  ( 0.05014649552828275014, 196.4853777576173002, 34.74886208192143044 ) ) ;
#6427 = CARTESIAN_POINT ( 'NONE',  ( 82.99999999453763166, 155.0000000000000000, 14.49999999999999467 ) ) ;
#6428 = CARTESIAN_POINT ( 'NONE',  ( -12.00000000000000711, 207.0476921513413515, 75.50113791807856956 ) ) ;
#6429 = CARTESIAN_POINT ( 'NONE',  ( 8.015496119326531499, 209.5516654185219636, 97.85113791807857808 ) ) ;
#6430 = EDGE_CURVE ( 'NONE', #20010, #25373, #16775, .T. ) ;
#6431 = CARTESIAN_POINT ( 'NONE',  ( -0.05014649552828403384, 217.5146222423826714, 63.24886208192143755 ) ) ;
#6432 = CARTESIAN_POINT ( 'NONE',  ( 2.621086668468698644, 7.606368536631364030, -7.634085501268425666 ) ) ;
#6433 = AXIS2_PLACEMENT_3D ( 'NONE', #6627, #17012, #14792 ) ;
#6434 = EDGE_LOOP ( 'NONE', ( #12045, #33040, #21796 ) ) ;
#6435 = CARTESIAN_POINT ( 'NONE',  ( -3.753561863808878130, 218.3979405102790281, 63.09886208192143187 ) ) ;
#6436 = VERTEX_POINT ( 'NONE', #10376 ) ;
#6437 = CARTESIAN_POINT ( 'NONE',  ( 74.37499999726881583, 155.0000000000000000, 15.58253174999999402 ) ) ;
#6438 = CARTESIAN_POINT ( 'NONE',  ( 2.517493886309087436, 199.4062855549015865, 40.59886208192143897 ) ) ;
#6439 = VERTEX_POINT ( 'NONE', #5245 ) ;
#6440 = EDGE_CURVE ( 'NONE', #31548, #32869, #16241, .T. ) ;
#6441 = CARTESIAN_POINT ( 'NONE',  ( 86.47499999726881015, 149.9369285172503510, 15.58253174999999580 ) ) ;
#6442 = DIRECTION ( 'NONE',  ( -0.9396926207859143121, 0.000000000000000000, -0.3420201433256525592 ) ) ;
#6443 = CARTESIAN_POINT ( 'NONE',  ( 10.00000000000000888, 207.0476921513417494, 0.9988620819214907298 ) ) ;
#6444 = CARTESIAN_POINT ( 'NONE',  ( 8.000000000000008882, 206.9523078486586485, 53.00113791807857666 ) ) ;
#6445 = AXIS2_PLACEMENT_3D ( 'NONE', #16296, #19027, #29752 ) ;
#6446 = EDGE_CURVE ( 'NONE', #15275, #4416, #11049, .T. ) ;
#6447 = LINE ( 'NONE', #30117, #15645 ) ;
#6448 = CARTESIAN_POINT ( 'NONE',  ( 8.062137200540822946, 212.9164362838583315, 30.69886208192144039 ) ) ;
#6449 = CARTESIAN_POINT ( 'NONE',  ( 67.67499999726881299, 168.2552932293087906, -9.630534252274387086 ) ) ;
#6450 = ORIENTED_EDGE ( 'NONE', *, *, #8545, .T. ) ;
#6451 = DIRECTION ( 'NONE',  ( -0.000000000000000000, -0.000000000000000000, 1.000000000000000000 ) ) ;
#6452 =( NAMED_UNIT ( * ) PLANE_ANGLE_UNIT ( ) SI_UNIT ( $, .RADIAN. ) );
#6453 = CARTESIAN_POINT ( 'NONE',  ( 52.08867513459482268, 142.2402378747194405, 9.270509831248432420 ) ) ;
#6454 = CARTESIAN_POINT ( 'NONE',  ( -7.025762299539908296E-16, -8.895730773063899477, -7.917997657324741034 ) ) ;
#6455 = CARTESIAN_POINT ( 'NONE',  ( -6.444103211790928043, 202.2591342207265939, 14.19886208192143684 ) ) ;
#6456 = CARTESIAN_POINT ( 'NONE',  ( -0.05014649552810635652, 196.4853777576173002, 59.75113791807857666 ) ) ;
#6457 = CARTESIAN_POINT ( 'NONE',  ( -8.062137200540920645, 212.9164362838581894, 36.80113791807856671 ) ) ;
#6458 = AXIS2_PLACEMENT_3D ( 'NONE', #7613, #12878, #10343 ) ;
#6459 = CARTESIAN_POINT ( 'NONE',  ( 8.000000000000008882, 207.0476921513415220, 99.99886208192143044 ) ) ;
#6460 = CARTESIAN_POINT ( 'NONE',  ( 44.82499999726880446, 141.7447067706911810, -9.630534252274385310 ) ) ;
#6461 = DIRECTION ( 'NONE',  ( -1.000000000000000000, -0.000000000000000000, -0.000000000000000000 ) ) ;
#6462 = CARTESIAN_POINT ( 'NONE',  ( 115.4999999999999858, 155.0000000000000000, -6.938893903907228378E-15 ) ) ;
#6463 = CARTESIAN_POINT ( 'NONE',  ( -9.680171189290831535, 214.0920067884431148, 18.80113791807856671 ) ) ;
#6464 = PLANE ( 'NONE',  #6433 ) ;
#6465 = CARTESIAN_POINT ( 'NONE',  ( 3.135527875058820690, 216.4958274776887492, 70.40113791807857524 ) ) ;
#6466 = CARTESIAN_POINT ( 'NONE',  ( -9.984503880673475606, 210.2968891136704315, 39.65113791807857524 ) ) ;
#6467 = CARTESIAN_POINT ( 'NONE',  ( 32.50000000000000000, 155.0000000000000000, -15.00000000000002487 ) ) ;
#6468 = FACE_BOUND ( 'NONE', #6887, .T. ) ;
#6469 = CARTESIAN_POINT ( 'NONE',  ( -11.89830997168683702, 232.6342992855866783, 103.4854814124441447 ) ) ;
#6470 = CARTESIAN_POINT ( 'NONE',  ( -10.01549611932659545, 210.2015048109875011, 5.648862081921436129 ) ) ;
#6471 = CARTESIAN_POINT ( 'NONE',  ( 64.69999999453762030, 167.3344367211045096, 8.961492836873468093 ) ) ;
#6472 = ORIENTED_EDGE ( 'NONE', *, *, #13635, .T. ) ;
#6473 = CARTESIAN_POINT ( 'NONE',  ( -7.456977232089304408, 196.8216656703010301, 51.05113791807856671 ) ) ;
#6474 = CIRCLE ( 'NONE', #25509, 1.000000000000000000 ) ;
#6475 = CARTESIAN_POINT ( 'NONE',  ( 4.984841277089725686, 213.7757310962907411, 70.55113791807856671 ) ) ;
#6476 = EDGE_CURVE ( 'NONE', #7575, #12674, #23239, .T. ) ;
#6477 = B_SPLINE_CURVE_WITH_KNOTS ( 'NONE', 3,
 ( #11007, #8612, #14400, #27177, #17123, #14055 ),
 .UNSPECIFIED., .F., .F.,
 ( 4, 2, 4 ),
 ( 0.003841072314098346787, 0.005765657563962181195, 0.007690242813826015170 ),
 .UNSPECIFIED. ) ;
#6478 = CARTESIAN_POINT ( 'NONE',  ( 6.220909254589681581, 198.5229672870052582, 34.44886208192143329 ) ) ;
#6479 = EDGE_CURVE ( 'NONE', #29326, #19336, #13910, .T. ) ;
#6480 = ORIENTED_EDGE ( 'NONE', *, *, #6366, .T. ) ;
#6481 = CARTESIAN_POINT ( 'NONE',  ( 3.044812012440130555, 197.4746971517856764, 86.60113791807857808 ) ) ;
#6482 = ADVANCED_FACE ( 'NONE', ( #8967 ), #3851, .F. ) ;
#6483 = VERTEX_POINT ( 'NONE', #8466 ) ;
#6484 = EDGE_CURVE ( 'NONE', #24452, #32263, #28903, .T. ) ;
#6485 = CIRCLE ( 'NONE', #29883, 2.500000000000000000 ) ;
#6486 = CARTESIAN_POINT ( 'NONE',  ( 42.78867513459481842, 155.0000000000000000, -15.00000000000002487 ) ) ;
#6487 = DIRECTION ( 'NONE',  ( 0.000000000000000000, 0.000000000000000000, 1.000000000000000000 ) ) ;
#6488 = ORIENTED_EDGE ( 'NONE', *, *, #15413, .F. ) ;
#6489 = CARTESIAN_POINT ( 'NONE',  ( 0.05014649552807626948, 215.4116977939061144, 25.25113791807856956 ) ) ;
#6490 = CARTESIAN_POINT ( 'NONE',  ( -60.15146012614710003, 194.9557722165940845, -1.884122726181822971 ) ) ;
#6491 = CARTESIAN_POINT ( 'NONE',  ( -6.139770520408224463, 198.4640165459539389, 5.048862081921435596 ) ) ;
#6492 = CARTESIAN_POINT ( 'NONE',  ( 50.37499999726881583, 155.0000000000000000, 15.58253174999999402 ) ) ;
#6493 = VERTEX_POINT ( 'NONE', #19357 ) ;
#6494 = CARTESIAN_POINT ( 'NONE',  ( 7.984503880673485376, 204.3529502787953902, 50.15113791807857524 ) ) ;
#6495 = CARTESIAN_POINT ( 'NONE',  ( -9.521242624480144912, 207.9188892840786878, 102.6634595774070533 ) ) ;
#6496 = CARTESIAN_POINT ( 'NONE',  ( -13.75000000000001954, 23.81569860407205752, 0.000000000000000000 ) ) ;
#6497 = CIRCLE ( 'NONE', #7062, 27.50000000000000355 ) ;
#6498 = CARTESIAN_POINT ( 'NONE',  ( 0.05014649552828275708, 196.4853777576173002, 94.74886208192141623 ) ) ;
#6499 = CARTESIAN_POINT ( 'NONE',  ( 59.67499999726880588, 168.2552932293087906, -9.630534252274385310 ) ) ;
#6500 = CARTESIAN_POINT ( 'NONE',  ( 9.984503880673470277, 203.7031108863295401, 32.15113791807857524 ) ) ;
#6501 = DIRECTION ( 'NONE',  ( 1.000000000000000000, 0.000000000000000000, 0.000000000000000000 ) ) ;
#6502 = CARTESIAN_POINT ( 'NONE',  ( -9.736236675708031640, 214.0148392665760753, 80.79886208192144181 ) ) ;
#6503 = CARTESIAN_POINT ( 'NONE',  ( 83.19999999999998863, 167.3344367211045096, 8.961492836873468093 ) ) ;
#6504 = CARTESIAN_POINT ( 'NONE',  ( 65.78867513459482552, 155.0000000000000000, 15.00000000000001243 ) ) ;
#6505 = CARTESIAN_POINT ( 'NONE',  ( 117.5000000000000142, 155.0000000000000000, -6.938893903907228378E-15 ) ) ;
#6506 = CARTESIAN_POINT ( 'NONE',  ( -3.135527875058821579, 197.5041725223112223, 98.90113791807857524 ) ) ;
#6507 = DIRECTION ( 'NONE',  ( 1.000000000000000000, -0.000000000000000000, -0.000000000000000000 ) ) ;
#6508 = CARTESIAN_POINT ( 'NONE',  ( 45.87499999726880162, 171.3844434931184253, -7.942151717890132712E-15 ) ) ;
#6509 = CARTESIAN_POINT ( 'NONE',  ( -8.062137200540920645, 212.9164362838581894, 36.80113791807856671 ) ) ;
#6510 = CARTESIAN_POINT ( 'NONE',  ( 85.02499999726882152, 149.9369285172503510, -15.58253175000000823 ) ) ;
#6511 = VERTEX_POINT ( 'NONE', #21743 ) ;
#6512 = CARTESIAN_POINT ( 'NONE',  ( -5.276765049035075705, 6.073111908730296271, -7.634085501268424778 ) ) ;
#6513 = CARTESIAN_POINT ( 'NONE',  ( -6.539196172009840602, -3.775406670193658165, -6.286444963328103874 ) ) ;
#6514 = CARTESIAN_POINT ( 'NONE',  ( 49.99999999453763166, 155.0000000000000000, -14.50000000000000711 ) ) ;
#6515 = CARTESIAN_POINT ( 'NONE',  ( 0.05014649552807549926, 219.6175466908591716, 22.25113791807856956 ) ) ;
#6516 = DIRECTION ( 'NONE',  ( 0.000000000000000000, 0.000000000000000000, 1.000000000000000000 ) ) ;
#6517 = DIRECTION ( 'NONE',  ( -1.000000000000000000, -0.000000000000000000, -0.000000000000000000 ) ) ;
#6518 = ORIENTED_EDGE ( 'NONE', *, *, #9752, .F. ) ;
#6519 = CARTESIAN_POINT ( 'NONE',  ( 3.662846001189864698, 218.4274158808046593, 42.39886208192144323 ) ) ;
#6520 = CARTESIAN_POINT ( 'NONE',  ( 3.044812012440130555, 197.4746971517856764, 2.601137918078566091 ) ) ;
#6521 = CIRCLE ( 'NONE', #14123, 4.200000000000001954 ) ;
#6522 = CARTESIAN_POINT ( 'NONE',  ( 6.220909254589536808, 215.4770327129947702, 49.55113791807855250 ) ) ;
#6523 =( BOUNDED_CURVE ( )  B_SPLINE_CURVE ( 2, ( #26333, #30960, #15602, #5545, #2999, #13378, #23776, #12886, #13217, #18335, #29058 ),
 .UNSPECIFIED., .F., .T. ) 
 B_SPLINE_CURVE_WITH_KNOTS ( ( 3, 2, 2, 2, 2, 3 ),
 ( 0.9464285714285712858, 0.9499999999999998446, 0.9535714285714284033, 0.9571428571428569620, 0.9607142857142855208, 0.9642857142857140795 ),
 .UNSPECIFIED. ) 
 CURVE ( )  GEOMETRIC_REPRESENTATION_ITEM ( )  RATIONAL_B_SPLINE_CURVE ( ( 1.000000000000001554, 0.9510565162951518658, 1.000000000000000000, 0.9510565162951534202, 1.000000000000000000, 0.9510565162951534202, 1.000000000000000000, 0.9510565162951534202, 1.000000000000000000, 0.9510565162951549745, 0.9999999999999984457 ) ) 
 REPRESENTATION_ITEM ( '' )  );
#6524 = CARTESIAN_POINT ( 'NONE',  ( 8.015496119326595448, 204.4483345814782638, 10.14886208192143435 ) ) ;
#6525 = CARTESIAN_POINT ( 'NONE',  ( 79.48867513459484258, 167.7597621252805880, 9.270509831248428867 ) ) ;
#6526 = VERTEX_POINT ( 'NONE', #802 ) ;
#6527 = CARTESIAN_POINT ( 'NONE',  ( 6.500168698208244500, 202.3363017425938324, 100.2988620819214276 ) ) ;
#6528 = CARTESIAN_POINT ( 'NONE',  ( 107.9108275708642850, 155.0000000000000000, 13.00000000000001066 ) ) ;
#6529 = CARTESIAN_POINT ( 'NONE',  ( -4.903702542908602524, 213.8346818373418898, 39.95113791807856529 ) ) ;
#6530 = CARTESIAN_POINT ( 'NONE',  ( 115.4999999999999858, 52.61186241335891367, 27.43481878086798176 ) ) ;
#6531 = ORIENTED_EDGE ( 'NONE', *, *, #191, .F. ) ;
#6532 = CARTESIAN_POINT ( 'NONE',  ( 36.12499999726881583, 155.0000000000000000, 15.58253174999999402 ) ) ;
#6533 = CARTESIAN_POINT ( 'NONE',  ( 39.18867513459482410, 169.2658477444273331, -4.635254915624224203 ) ) ;
#6534 = CARTESIAN_POINT ( 'NONE',  ( -8.062137200540822946, 201.0835637161416400, 65.19886208192143329 ) ) ;
#6535 = CARTESIAN_POINT ( 'NONE',  ( 37.77499999726881441, 169.8198683612136222, -4.815267126137197984 ) ) ;
#6536 = CARTESIAN_POINT ( 'NONE',  ( -52.50000000000002132, 155.0000000000000000, 6.938893903907228378E-15 ) ) ;
#6537 = CARTESIAN_POINT ( 'NONE',  ( -3.135527875058821579, 197.5041725223112223, 2.901137918078565914 ) ) ;
#6538 = CARTESIAN_POINT ( 'NONE',  ( 63.79999999999999716, 142.6655632788954620, 8.961492836873471646 ) ) ;
#6539 = CARTESIAN_POINT ( 'NONE',  ( 1.083333333333333703, 6.880090707843044662, -5.848636054922036642 ) ) ;
#6540 = CARTESIAN_POINT ( 'NONE',  ( -0.05014649552828365914, 215.4116977939061144, 84.24886208192143044 ) ) ;
#6541 = DIRECTION ( 'NONE',  ( 1.000000000000000000, 0.000000000000000000, 0.000000000000000000 ) ) ;
#6542 = DIRECTION ( 'NONE',  ( -0.000000000000000000, -0.000000000000000000, -1.000000000000000000 ) ) ;
#6543 = CARTESIAN_POINT ( 'NONE',  ( 57.52499999726881441, 169.8198683612136222, -4.815267126137197984 ) ) ;
#6545 = ORIENTED_EDGE ( 'NONE', *, *, #27084, .T. ) ;
#6544 = CARTESIAN_POINT ( 'NONE',  ( -6.139770520408368348, 215.5359834540460042, 15.95113791807856884 ) ) ;
#6546 = CARTESIAN_POINT ( 'NONE',  ( -31.74999999999995737, 0.000000000000000000, 8.000000000000000000 ) ) ;
#6547 = CARTESIAN_POINT ( 'NONE',  ( 84.07499999726877604, 168.2552932293087906, 9.630534252274372875 ) ) ;
#6548 = CARTESIAN_POINT ( 'NONE',  ( -3.662846001190052991, 218.4274158808045740, 85.10113791807857808 ) ) ;
#6549 = DIRECTION ( 'NONE',  ( 1.000000000000000000, -0.000000000000000000, -0.000000000000000000 ) ) ;
#6550 = CARTESIAN_POINT ( 'NONE',  ( 53.48867513459483547, 167.7597621252805880, 9.270509831248428867 ) ) ;
#6551 = ORIENTED_EDGE ( 'NONE', *, *, #32978, .T. ) ;
#6552 = CARTESIAN_POINT ( 'NONE',  ( 9.680171189290716072, 214.0920067884432854, 66.69886208192143329 ) ) ;
#6553 = CARTESIAN_POINT ( 'NONE',  ( 3.044812012439969795, 216.5253028482143520, 78.39886208192143613 ) ) ;
#6554 = CARTESIAN_POINT ( 'NONE',  ( -9.680171189290716072, 199.9079932115567146, 17.19886208192143684 ) ) ;
#6555 = CARTESIAN_POINT ( 'NONE',  ( -3.399999999999999911, 4.163799117101000559E-16, -7.554475477074173106 ) ) ;
#6556 = CARTESIAN_POINT ( 'NONE',  ( -0.05014649552810635652, 196.4853777576173002, 23.75113791807855890 ) ) ;
#6557 = CARTESIAN_POINT ( 'NONE',  ( -0.05014649552828403384, 217.5146222423826714, 93.24886208192140202 ) ) ;
#6558 = ORIENTED_EDGE ( 'NONE', *, *, #26437, .F. ) ;
#6559 = CARTESIAN_POINT ( 'NONE',  ( 38.71132485994280614, 155.0000000000000000, 15.00000000000001243 ) ) ;
#6560 = ORIENTED_EDGE ( 'NONE', *, *, #28904, .F. ) ;
#6561 = CARTESIAN_POINT ( 'NONE',  ( -3.250000000000000444, -5.629165124598859649, -5.592027715088708995 ) ) ;
#6562 = CARTESIAN_POINT ( 'NONE',  ( 6.444103211790928043, 211.7408657792734061, 69.69886208192143329 ) ) ;
#6563 = ORIENTED_EDGE ( 'NONE', *, *, #25009, .T. ) ;
#6564 = PRODUCT_DEFINITION_SHAPE ( 'NONE', 'NONE',  #33696 ) ;
#6565 = EDGE_CURVE ( 'NONE', #11757, #8265, #15081, .T. ) ;
#6566 = CARTESIAN_POINT ( 'NONE',  ( 86.42499999726881299, 141.7447067706911810, 9.630534252274376428 ) ) ;
#6567 = ORIENTED_EDGE ( 'NONE', *, *, #17503, .T. ) ;
#6568 = DIRECTION ( 'NONE',  ( 1.000000000000000000, 0.000000000000000000, 0.000000000000000000 ) ) ;
#6569 = CARTESIAN_POINT ( 'NONE',  ( 73.32499999726880446, 164.1591823560292198, -12.60653300113719766 ) ) ;
#6570 = DIRECTION ( 'NONE',  ( -0.000000000000000000, -0.000000000000000000, 1.000000000000000000 ) ) ;
#6571 = CARTESIAN_POINT ( 'NONE',  ( -4.903702542908602524, 213.8346818373418898, 72.95113791807857240 ) ) ;
#6572 = CARTESIAN_POINT ( 'NONE',  ( -3.499999999999999556, -3.004629197474309385E-15, -2.899999999999999911 ) ) ;
#6573 = AXIS2_PLACEMENT_3D ( 'NONE', #13081, #4908, #2189 ) ;
#6574 = SURFACE_STYLE_FILL_AREA ( #19184 ) ;
#6575 = CARTESIAN_POINT ( 'NONE',  ( 38.40000000000000568, 150.2886644046228639, -14.50000000000000888 ) ) ;
#6576 = CARTESIAN_POINT ( 'NONE',  ( 6.500168698208244500, 202.3363017425938324, 55.29886208192144892 ) ) ;
#6577 = CARTESIAN_POINT ( 'NONE',  ( 6.220909254589536808, 215.4770327129947702, 73.55113791807858092 ) ) ;
#6578 = CARTESIAN_POINT ( 'NONE',  ( -8.542937654374687995, 0.000000000000000000, -6.800000000000000711 ) ) ;
#6579 = CARTESIAN_POINT ( 'NONE',  ( 73.21132485994282035, 139.2280666364260071, -4.041636747397287284E-15 ) ) ;
#6580 = CARTESIAN_POINT ( 'NONE',  ( 77.50000000000000000, 155.0000000000000000, 15.50000000000000355 ) ) ;
#6581 = CARTESIAN_POINT ( 'NONE',  ( 53.82499999726880446, 168.2552932293087906, 9.630534252274372875 ) ) ;
#6582 = CARTESIAN_POINT ( 'NONE',  ( 0.05014649552807549926, 219.6175466908591716, 55.25113791807857666 ) ) ;
#6583 = CARTESIAN_POINT ( 'NONE',  ( -129.5873785388598662, -2.643999646947223336, 35.00001199999999812 ) ) ;
#6584 = CARTESIAN_POINT ( 'NONE',  ( 12.01549611932652972, 210.8513442034534933, 4.851137918078565647 ) ) ;
#6586 = CARTESIAN_POINT ( 'NONE',  ( -9.984503880673475606, 210.2968891136704315, 78.65113791807856103 ) ) ;
#6585 = APPLICATION_CONTEXT ( 'automotive_design' ) ;
#6587 = CARTESIAN_POINT ( 'NONE',  ( -0.05014649552828442242, 219.6175466908591716, 36.24886208192142334 ) ) ;
#6588 = CARTESIAN_POINT ( 'NONE',  ( 10.01549611932659367, 203.7984951890124421, 49.14886208192143613 ) ) ;
#6589 = CARTESIAN_POINT ( 'NONE',  ( 85.29999999453761461, 142.6655632788954620, 8.961492836873471646 ) ) ;
#6590 = CARTESIAN_POINT ( 'NONE',  ( 7.456977232089302632, 217.1783343296989131, 88.55113791807858092 ) ) ;
#6591 = CARTESIAN_POINT ( 'NONE',  ( 8.015496119326531499, 209.5516654185219636, 100.8511379180785781 ) ) ;
#6592 = ADVANCED_FACE ( 'NONE', ( #1133 ), #16798, .F. ) ;
#6593 = CARTESIAN_POINT ( 'NONE',  ( 10.00000000000000711, 207.0476921513415220, 57.99886208192143044 ) ) ;
#6594 = SURFACE_STYLE_USAGE ( .BOTH. , #22266 ) ;
#6595 = ORIENTED_EDGE ( 'NONE', *, *, #18744, .F. ) ;
#6596 = CARTESIAN_POINT ( 'NONE',  ( -0.05014649552828442242, 219.6175466908591716, 57.24886208192144466 ) ) ;
#6597 = AXIS2_PLACEMENT_3D ( 'NONE', #1503, #19565, #9853 ) ;
#6598 = EDGE_LOOP ( 'NONE', ( #10063, #33597, #18191, #768 ) ) ;
#6599 = CARTESIAN_POINT ( 'NONE',  ( 69.57499999726881867, 164.1591823560292198, -12.60653300113719766 ) ) ;
#6600 = CARTESIAN_POINT ( 'NONE',  ( -8.015496119326597224, 209.5516654185217362, 38.64886208192143613 ) ) ;
#6601 = ORIENTED_EDGE ( 'NONE', *, *, #5218, .T. ) ;
#6602 = EDGE_CURVE ( 'NONE', #23832, #31055, #10813, .T. ) ;
#6603 = CARTESIAN_POINT ( 'NONE',  ( 83.87499999726880162, 171.3844434931184253, -7.942151717890134290E-15 ) ) ;
#6604 = DIRECTION ( 'NONE',  ( 0.5526942671207055735, 0.1536855300543024383, 0.8190908404712107238 ) ) ;
#6605 = CARTESIAN_POINT ( 'NONE',  ( 3.281878800801977025, 207.2857746820136526, -8.268545444955467616 ) ) ;
#6606 = CARTESIAN_POINT ( 'NONE',  ( 6.444103211791042618, 202.2591342207267644, 59.30113791807857382 ) ) ;
#6607 = DIRECTION ( 'NONE',  ( -1.000000000000000000, 0.000000000000000000, 0.000000000000000000 ) ) ;
#6608 = CARTESIAN_POINT ( 'NONE',  ( 3.044812012439969795, 216.5253028482143520, 42.39886208192143613 ) ) ;
#6609 = CARTESIAN_POINT ( 'NONE',  ( 67.57499999726881867, 164.1591823560292198, -12.60653300113719766 ) ) ;
#6610 = EDGE_LOOP ( 'NONE', ( #4334, #910, #23987, #29946 ) ) ;
#6611 = CARTESIAN_POINT ( 'NONE',  ( 5.000000000000000000, 4.685197434473814759, -5.637851296924623057E-15 ) ) ;
#6612 = ADVANCED_FACE ( 'NONE', ( #13579 ), #6240, .F. ) ;
#6613 = DIRECTION ( 'NONE',  ( 0.000000000000000000, 0.000000000000000000, -1.000000000000000000 ) ) ;
#6614 = DIRECTION ( 'NONE',  ( -1.000000000000000000, 0.000000000000000000, 0.000000000000000000 ) ) ;
#6615 = CARTESIAN_POINT ( 'NONE',  ( -4.903702542908436435, 200.1653181626580249, 11.04886208192143648 ) ) ;
#6616 = CARTESIAN_POINT ( 'NONE',  ( 6.220909254589536808, 215.4770327129947702, 64.55113791807858092 ) ) ;
#6617 = CARTESIAN_POINT ( 'NONE',  ( -8.062137200540920645, 212.9164362838581894, 42.80113791807857382 ) ) ;
#6618 = CARTESIAN_POINT ( 'NONE',  ( 70.91132485994280898, 146.1832212156128890, 12.13525491562421976 ) ) ;
#6619 = CONTEXT_DEPENDENT_SHAPE_REPRESENTATION ( #85, #9004 ) ;
#6620 = CARTESIAN_POINT ( 'NONE',  ( -0.05014649552810635652, 196.4853777576173002, 20.75113791807855890 ) ) ;
#6621 = AXIS2_PLACEMENT_3D ( 'NONE', #3433, #29167, #6154 ) ;
#6622 = CARTESIAN_POINT ( 'NONE',  ( -4.903702542908436435, 200.1653181626580249, 101.0488620819214276 ) ) ;
#6623 = CARTESIAN_POINT ( 'NONE',  ( 46.12499999726880873, 155.0000000000000000, 15.58253174999999402 ) ) ;
#6624 = DIRECTION ( 'NONE',  ( 1.000000000000000000, -0.000000000000000000, -0.000000000000000000 ) ) ;
#6625 = CARTESIAN_POINT ( 'NONE',  ( 87.50000000000004263, 150.3648420706765592, -14.53435407936543200 ) ) ;
#6626 = CARTESIAN_POINT ( 'NONE',  ( -9.680171189290831535, 214.0920067884431148, 27.80113791807857027 ) ) ;
#6627 = CARTESIAN_POINT ( 'NONE',  ( -68.50000000000000000, 215.0000000000000000, 0.000000000000000000 ) ) ;
#6628 = EDGE_CURVE ( 'NONE', #16441, #26329, #18698, .T. ) ;
#6629 = CARTESIAN_POINT ( 'NONE',  ( 8.062137200540920645, 201.0835637161417822, 71.30113791807856671 ) ) ;
#6630 = CARTESIAN_POINT ( 'NONE',  ( 8.062137200540920645, 201.0835637161417822, 35.30113791807857382 ) ) ;
#6631 = CARTESIAN_POINT ( 'NONE',  ( 7.500000000000000000, 4.330127018922199866, -1.000000000000000888 ) ) ;
#6632 = CARTESIAN_POINT ( 'NONE',  ( 33.24999999726880873, 155.0000000000000000, -15.58253175000000823 ) ) ;
#6633 = CARTESIAN_POINT ( 'NONE',  ( 12.00000000000000711, 207.0476921513415220, 0.9988620819214339974 ) ) ;
#6634 = CARTESIAN_POINT ( 'NONE',  ( -10.00000000000000711, 206.9523078486584495, 23.49886208192143755 ) ) ;
#6635 = CARTESIAN_POINT ( 'NONE',  ( 64.09999999453764019, 159.7113355953771077, -14.50000000000000888 ) ) ;
#6636 = VECTOR ( 'NONE', #20990, 1000.000000000000000 ) ;
#6637 = VERTEX_POINT ( 'NONE', #23970 ) ;
#6638 = CARTESIAN_POINT ( 'NONE',  ( -7.375838497908182134, 217.2372850707499765, 48.95113791807855108 ) ) ;
#6639 = CARTESIAN_POINT ( 'NONE',  ( 7.984503880673485376, 204.3529502787953902, 74.15113791807857524 ) ) ;
#6640 = EDGE_CURVE ( 'NONE', #29364, #22604, #30553, .T. ) ;
#6641 = CARTESIAN_POINT ( 'NONE',  ( -10.01549611932659722, 210.2015048109875011, 32.64886208192143613 ) ) ;
#6642 = DIRECTION ( 'NONE',  ( 1.000000000000000000, 0.000000000000000000, 0.000000000000000000 ) ) ;
#6643 = ORIENTED_EDGE ( 'NONE', *, *, #9825, .F. ) ;
#6644 = CARTESIAN_POINT ( 'NONE',  ( -3.044812012440131443, 216.5253028482142952, 91.10113791807857808 ) ) ;
#6645 = ORIENTED_EDGE ( 'NONE', *, *, #3445, .T. ) ;
#6646 = CARTESIAN_POINT ( 'NONE',  ( 3.399999999999999911, 0.000000000000000000, -8.000000000000000000 ) ) ;
#6647 = FACE_OUTER_BOUND ( 'NONE', #9460, .T. ) ;
#6648 = ORIENTED_EDGE ( 'NONE', *, *, #4323, .F. ) ;
#6649 = CARTESIAN_POINT ( 'NONE',  ( 7.984503880673485376, 204.3529502787953902, 26.15113791807857169 ) ) ;
#6650 = CARTESIAN_POINT ( 'NONE',  ( 85.61132485994281183, 150.1262045565064227, -15.00000000000002665 ) ) ;
#6651 = CARTESIAN_POINT ( 'NONE',  ( -6.139770520408224463, 198.4640165459539389, 8.048862081921434708 ) ) ;
#6652 = CARTESIAN_POINT ( 'NONE',  ( 53.37499999726881583, 155.0000000000000000, -15.58253175000000823 ) ) ;
#6653 = ORIENTED_EDGE ( 'NONE', *, *, #20985, .F. ) ;
#6654 = CARTESIAN_POINT ( 'NONE',  ( 4.903702542908601636, 200.1653181626581102, 53.45113791807857950 ) ) ;
#6655 = DIRECTION ( 'NONE',  ( 1.000000000000000000, -0.000000000000000000, -0.000000000000000000 ) ) ;
#6656 = AXIS2_PLACEMENT_3D ( 'NONE', #548, #3094, #21651 ) ;
#6657 = CARTESIAN_POINT ( 'NONE',  ( 115.4999999999999858, 102.0000000000001990, 89.64869280115064498 ) ) ;
#6658 = CARTESIAN_POINT ( 'NONE',  ( 10.00000000000000711, 207.0476921513415220, 90.99886208192144466 ) ) ;
#6659 = CIRCLE ( 'NONE', #25707, 12.10452846326765020 ) ;
#6660 = CARTESIAN_POINT ( 'NONE',  ( 60.17499999726881299, 164.1591823560292198, 12.60653300113718167 ) ) ;
#6661 = CARTESIAN_POINT ( 'NONE',  ( -3.044812012440131443, 216.5253028482142952, 31.10113791807856742 ) ) ;
#6662 = DIRECTION ( 'NONE',  ( -1.000000000000000000, 0.000000000000000000, 0.000000000000000000 ) ) ;
#6663 = EDGE_CURVE ( 'NONE', #3719, #5223, #9300, .T. ) ;
#6664 = EDGE_CURVE ( 'NONE', #25327, #7152, #16963, .T. ) ;
#6665 = CARTESIAN_POINT ( 'NONE',  ( 6.220909254589536808, 215.4770327129947702, 19.55113791807856671 ) ) ;
#6666 = DIRECTION ( 'NONE',  ( 6.123233995736766036E-17, 0.000000000000000000, -1.000000000000000000 ) ) ;
#6667 = CARTESIAN_POINT ( 'NONE',  ( 77.59999999999999432, 150.2886644046228639, 14.49999999999999645 ) ) ;
#6668 = CARTESIAN_POINT ( 'NONE',  ( -1.750000000000016209, -3.031088913245524985, -2.899999999999999911 ) ) ;
#6669 = FACE_OUTER_BOUND ( 'NONE', #9323, .T. ) ;
#6670 = CARTESIAN_POINT ( 'NONE',  ( -6.139770520408369237, 215.5359834540460042, 96.95113791807857240 ) ) ;
#6671 = DIRECTION ( 'NONE',  ( 0.000000000000000000, 0.000000000000000000, 1.000000000000000000 ) ) ;
#6672 = CARTESIAN_POINT ( 'NONE',  ( 45.67499999726881299, 168.2552932293087906, -9.630534252274385310 ) ) ;
#6673 = EDGE_CURVE ( 'NONE', #22495, #355, #9133, .T. ) ;
#6674 = CARTESIAN_POINT ( 'NONE',  ( -0.05014649552810635652, 196.4853777576173002, 38.75113791807856956 ) ) ;
#6675 = CARTESIAN_POINT ( 'NONE',  ( 85.62499999726880162, 171.3844434931184253, -7.942151717890132712E-15 ) ) ;
#6676 = AXIS2_PLACEMENT_3D ( 'NONE', #16411, #32718, #11771 ) ;
#6677 = CARTESIAN_POINT ( 'NONE',  ( 125.0000000000000000, -24.99999999999995737, -35.00000000000000000 ) ) ;
#6678 = DIRECTION ( 'NONE',  ( 0.000000000000000000, 0.000000000000000000, -1.000000000000000000 ) ) ;
#6679 = CARTESIAN_POINT ( 'NONE',  ( 47.79999999453762882, 146.4771138417591203, -11.73074641843674470 ) ) ;
#6680 = VERTEX_POINT ( 'NONE', #12366 ) ;
#6681 = CARTESIAN_POINT ( 'NONE',  ( 9.680171189290831535, 199.9079932115568852, 20.30113791807857027 ) ) ;
#6682 = ADVANCED_FACE ( 'NONE', ( #14415 ), #8627, .F. ) ;
#6683 = CARTESIAN_POINT ( 'NONE',  ( -10.95989699996054512, 207.3450541041420081, 103.1859396839448806 ) ) ;
#6684 = FACE_OUTER_BOUND ( 'NONE', #29573, .T. ) ;
#6685 = ORIENTED_EDGE ( 'NONE', *, *, #31152, .F. ) ;
#6686 = CIRCLE ( 'NONE', #7789, 3.500000000000000000 ) ;
#6687 = CARTESIAN_POINT ( 'NONE',  ( -0.05014649552828442242, 219.6175466908591716, 39.24886208192143755 ) ) ;
#6688 = CARTESIAN_POINT ( 'NONE',  ( -9.984503880673473830, 210.2968891136704315, 3.651137918078565026 ) ) ;
#6689 = CARTESIAN_POINT ( 'NONE',  ( -0.05014649552810635652, 196.4853777576173002, 62.75113791807856956 ) ) ;
#6690 = AXIS2_PLACEMENT_3D ( 'NONE', #20728, #2684, #20900 ) ;
#6691 = CARTESIAN_POINT ( 'NONE',  ( -2.517493886309087880, 214.5937144450984135, 24.09886208192143897 ) ) ;
#6692 = UNCERTAINTY_MEASURE_WITH_UNIT (LENGTH_MEASURE( 1.000000000000000082E-05 ), #18688, 'distance_accuracy_value', 'NONE');
#6693 = CARTESIAN_POINT ( 'NONE',  ( 5.978033218201114884, 4.054134411712192687, -0.5602453477493293255 ) ) ;
#6694 = VERTEX_POINT ( 'NONE', #4530 ) ;
#6695 = CARTESIAN_POINT ( 'NONE',  ( -6.500168698208244500, 211.6636982574061676, 101.7988620819214560 ) ) ;
#6696 = DIRECTION ( 'NONE',  ( 0.000000000000000000, 0.000000000000000000, -1.000000000000000000 ) ) ;
#6697 = CARTESIAN_POINT ( 'NONE',  ( -8.000000000000008882, 207.0476921513413515, 39.50113791807857666 ) ) ;
#6698 = CARTESIAN_POINT ( 'NONE',  ( 5.000000000000000000, 4.685197434473814759, -5.637851296924623057E-15 ) ) ;
#6699 = EDGE_LOOP ( 'NONE', ( #20691, #17591, #7058, #2558 ) ) ;
#6700 = CARTESIAN_POINT ( 'NONE',  ( 38.52499999726881441, 140.1801316387863778, 4.815267126137185549 ) ) ;
#6701 = DIRECTION ( 'NONE',  ( 0.000000000000000000, 0.000000000000000000, 1.000000000000000000 ) ) ;
#6702 = CARTESIAN_POINT ( 'NONE',  ( 6.220909254589536808, 215.4770327129947702, 1.551137918078565825 ) ) ;
#6703 = AXIS2_PLACEMENT_3D ( 'NONE', #26088, #13133, #23526 ) ;
#6704 = CARTESIAN_POINT ( 'NONE',  ( 6.139770520408223575, 215.5359834540460611, 66.54886208192144181 ) ) ;
#6705 = CARTESIAN_POINT ( 'NONE',  ( 38.07499999726880446, 168.2552932293087906, 9.630534252274372875 ) ) ;
#6706 = LINE ( 'NONE', #9588, #16735 ) ;
#6707 = CARTESIAN_POINT ( 'NONE',  ( 3.044812012440130555, 197.4746971517856764, 5.601137918078566535 ) ) ;
#6708 = AXIS2_PLACEMENT_3D ( 'NONE', #12654, #30215, #20496 ) ;
#6709 = CARTESIAN_POINT ( 'NONE',  ( 63.10000000000000142, 168.7903194862797420, 4.480746418436729606 ) ) ;
#6710 = DIRECTION ( 'NONE',  ( 0.000000000000000000, 1.000000000000000000, 0.000000000000000000 ) ) ;
#6711 = CARTESIAN_POINT ( 'NONE',  ( 7.984503880673422316, 209.6470497212048372, 78.84886208192143897 ) ) ;
#6712 = CARTESIAN_POINT ( 'NONE',  ( -2.558993250147282073, 7.638875775587784744, -7.593821156097241065 ) ) ;
#6713 = AXIS2_PLACEMENT_3D ( 'NONE', #5681, #2641, #10645 ) ;
#6714 = DIRECTION ( 'NONE',  ( 1.000000000000000000, 0.000000000000000000, 0.000000000000000000 ) ) ;
#6715 = AXIS2_PLACEMENT_3D ( 'NONE', #19469, #24586, #29070 ) ;
#6716 = CARTESIAN_POINT ( 'NONE',  ( 66.82499999726881867, 141.7447067706911810, -9.630534252274385310 ) ) ;
#6718 = ORIENTED_EDGE ( 'NONE', *, *, #30798, .T. ) ;
#6717 = CARTESIAN_POINT ( 'NONE',  ( 10.01549611932653860, 210.2015048109876716, 22.85113791807856742 ) ) ;
#6719 = CARTESIAN_POINT ( 'NONE',  ( -9.092171885314261459, 26.50489691992488162, -0.2827231011780766967 ) ) ;
#6720 = CARTESIAN_POINT ( 'NONE',  ( 81.67499999726881299, 168.2552932293087906, -9.630534252274385310 ) ) ;
#6721 = CARTESIAN_POINT ( 'NONE',  ( 12.01549611932652972, 210.8513442034534933, 88.85113791807857808 ) ) ;
#6722 = CARTESIAN_POINT ( 'NONE',  ( 72.28867513459482552, 139.2280666364260071, -4.041636747397287284E-15 ) ) ;
#6723 = ORIENTED_EDGE ( 'NONE', *, *, #12014, .F. ) ;
#6724 = CARTESIAN_POINT ( 'NONE',  ( 3.662846001189864698, 218.4274158808046593, 72.39886208192143613 ) ) ;
#6725 = CIRCLE ( 'NONE', #23584, 3.500000000000000000 ) ;
#6726 = CARTESIAN_POINT ( 'NONE',  ( 3.135527875058981895, 197.5041725223112792, 76.59886208192142476 ) ) ;
#6727 = CARTESIAN_POINT ( 'NONE',  ( -0.05014649552828442242, 219.6175466908591716, 12.24886208192143577 ) ) ;
#6728 = DIRECTION ( 'NONE',  ( 0.000000000000000000, 0.000000000000000000, 1.000000000000000000 ) ) ;
#6729 = CARTESIAN_POINT ( 'NONE',  ( 6.139770520408368348, 198.4640165459539674, 29.45113791807856529 ) ) ;
#6730 = CARTESIAN_POINT ( 'NONE',  ( 66.38867513459483405, 140.7341522555726669, -4.635254915624220651 ) ) ;
#6731 = CARTESIAN_POINT ( 'NONE',  ( 8.118202686958138514, 201.1607312380088501, 85.29886208192144181 ) ) ;
#6732 = CARTESIAN_POINT ( 'NONE',  ( 39.61132485994280472, 150.1262045565063943, -15.00000000000000355 ) ) ;
#6733 = ORIENTED_EDGE ( 'NONE', *, *, #16415, .T. ) ;
#6734 = DIRECTION ( 'NONE',  ( 2.312964634635740985E-16, -1.000000000000000000, 0.000000000000000000 ) ) ;
#6735 = CARTESIAN_POINT ( 'NONE',  ( -2.517493886309087880, 214.5937144450984135, 69.09886208192143897 ) ) ;
#6736 = ORIENTED_EDGE ( 'NONE', *, *, #22443, .F. ) ;
#6737 = AXIS2_PLACEMENT_3D ( 'NONE', #20804, #7872, #20130 ) ;
#6738 = CARTESIAN_POINT ( 'NONE',  ( 85.72499999726882436, 169.8198683612136222, 4.815267126137181997 ) ) ;
#6739 = ORIENTED_EDGE ( 'NONE', *, *, #16983, .F. ) ;
#6740 = CARTESIAN_POINT ( 'NONE',  ( 69.51132485994280330, 146.1832212156128890, -12.13525491562423042 ) ) ;
#6741 = CARTESIAN_POINT ( 'NONE',  ( 76.92499999726881299, 145.8408176439707802, -12.60653300113719588 ) ) ;
#6742 = DIRECTION ( 'NONE',  ( 0.000000000000000000, 1.000000000000000000, -6.454785026890489601E-15 ) ) ;
#6743 = CARTESIAN_POINT ( 'NONE',  ( 4.984841277089725686, 213.7757310962907411, 79.55113791807858092 ) ) ;
#6744 = DIRECTION ( 'NONE',  ( 1.000000000000000000, 0.000000000000000000, 0.000000000000000000 ) ) ;
#6745 =( GEOMETRIC_REPRESENTATION_CONTEXT ( 3 ) GLOBAL_UNCERTAINTY_ASSIGNED_CONTEXT ( ( #2847 ) ) GLOBAL_UNIT_ASSIGNED_CONTEXT ( ( #3926, #32542, #30168 ) ) REPRESENTATION_CONTEXT ( 'NONE', 'WORKASPACE' ) );
#6746 = CARTESIAN_POINT ( 'NONE',  ( 44.70000000000000284, 163.5228861582408797, -11.73074641843674470 ) ) ;
#6747 = CARTESIAN_POINT ( 'NONE',  ( 2.426778023690075337, 214.6231898156240447, 54.39886208192144323 ) ) ;
#6748 = CARTESIAN_POINT ( 'NONE',  ( -6.500000000000000000, -3.155218591052673549, -0.5622968210053901350 ) ) ;
#6749 = CARTESIAN_POINT ( 'NONE',  ( 73.31132485994281467, 140.7341522555726669, -4.635254915624220651 ) ) ;
#6750 = VECTOR ( 'NONE', #517, 1000.000000000000000 ) ;
#6751 = CARTESIAN_POINT ( 'NONE',  ( 27.50000000000000355, 0.000000000000000000, -18.00000000000000000 ) ) ;
#6752 = CARTESIAN_POINT ( 'NONE',  ( 49.42499999726880588, 168.2552932293087906, -9.630534252274387086 ) ) ;
#6753 = CARTESIAN_POINT ( 'NONE',  ( 65.97499999726881015, 169.8198683612136222, 4.815267126137181997 ) ) ;
#6754 =( BOUNDED_CURVE ( )  B_SPLINE_CURVE ( 2, ( #25739, #10746, #10422, #10087, #28635, #10259, #20794, #31525, #18412, #20464, #31358 ),
 .UNSPECIFIED., .F., .T. ) 
 B_SPLINE_CURVE_WITH_KNOTS ( ( 3, 2, 2, 2, 2, 3 ),
 ( 0.4107142857142855874, 0.4142857142857141461, 0.4178571428571427049, 0.4214285714285713191, 0.4249999999999998779, 0.4285714285714284366 ),
 .UNSPECIFIED. ) 
 CURVE ( )  GEOMETRIC_REPRESENTATION_ITEM ( )  RATIONAL_B_SPLINE_CURVE ( ( 1.000000000000001554, 0.9510565162951518658, 1.000000000000000000, 0.9510565162951534202, 1.000000000000000000, 0.9510565162951534202, 1.000000000000000000, 0.9510565162951534202, 1.000000000000000000, 0.9510565162951541973, 0.9999999999999992228 ) ) 
 REPRESENTATION_ITEM ( '' )  );
#6755 = CARTESIAN_POINT ( 'NONE',  ( -3.753561863808691168, 195.6020594897209435, 59.90113791807856103 ) ) ;
#6756 = LINE ( 'NONE', #6923, #33653 ) ;
#6757 = AXIS2_PLACEMENT_3D ( 'NONE', #9161, #19556, #27887 ) ;
#6758 = CARTESIAN_POINT ( 'NONE',  ( 11.98450388067348271, 203.0532714938637753, 5.151137918078566358 ) ) ;
#6759 = EDGE_CURVE ( 'NONE', #317, #17109, #11356, .T. ) ;
#6760 = CARTESIAN_POINT ( 'NONE',  ( 9.984503880673473830, 203.7031108863295401, 80.15113791807858945 ) ) ;
#6761 = CARTESIAN_POINT ( 'NONE',  ( 3.662846001189864698, 218.4274158808046593, 39.39886208192143613 ) ) ;
#6762 = CARTESIAN_POINT ( 'NONE',  ( 3.135527875058981895, 197.5041725223112792, 52.59886208192143897 ) ) ;
#6763 = CARTESIAN_POINT ( 'NONE',  ( 88.29999999453762882, 167.3344367211045096, -8.961492836873482304 ) ) ;
#6764 = CARTESIAN_POINT ( 'NONE',  ( 9.680171189290831535, 199.9079932115568852, 83.30113791807858092 ) ) ;
#6765 = CARTESIAN_POINT ( 'NONE',  ( 4.903702542908601636, 200.1653181626581102, 95.45113791807858661 ) ) ;
#6766 = CARTESIAN_POINT ( 'NONE',  ( 10.00000000000000711, 207.0476921513415220, 60.99886208192143755 ) ) ;
#6767 = FILL_AREA_STYLE ('',( #24659 ) ) ;
#6768 = ORIENTED_EDGE ( 'NONE', *, *, #8485, .T. ) ;
#6769 = CARTESIAN_POINT ( 'NONE',  ( -3.662846001189865142, 195.5725841191952838, 70.89886208192143613 ) ) ;
#6770 = MECHANICAL_DESIGN_GEOMETRIC_PRESENTATION_REPRESENTATION (  '', ( #8929 ), #12761 ) ;
#6771 = ORIENTED_EDGE ( 'NONE', *, *, #27793, .T. ) ;
#6772 = CARTESIAN_POINT ( 'NONE',  ( 69.07499999726881867, 141.7447067706911810, -9.630534252274385310 ) ) ;
#6773 = CARTESIAN_POINT ( 'NONE',  ( -2.426778023690076225, 199.3768101843759553, 43.89886208192144323 ) ) ;
#6774 = VERTEX_POINT ( 'NONE', #15086 ) ;
#6775 = CARTESIAN_POINT ( 'NONE',  ( 82.87499999726880162, 138.6155565068815747, -3.929120461958505118E-15 ) ) ;
#6776 = FACE_OUTER_BOUND ( 'NONE', #8694, .T. ) ;
#6777 = DIRECTION ( 'NONE',  ( -1.000000000000000000, -0.000000000000000000, -0.000000000000000000 ) ) ;
#6778 = CARTESIAN_POINT ( 'NONE',  ( -0.05014649552807731031, 198.5883022060938572, 62.75113791807856245 ) ) ;
#6779 = DIRECTION ( 'NONE',  ( 0.8660254037844382635, 0.5000000000000004441, 0.000000000000000000 ) ) ;
#6780 = CARTESIAN_POINT ( 'NONE',  ( -10.01549611932659722, 210.2015048109875011, 41.64886208192144323 ) ) ;
#6781 = ORIENTED_EDGE ( 'NONE', *, *, #17712, .F. ) ;
#6782 = DIRECTION ( 'NONE',  ( 0.000000000000000000, -1.000000000000000000, 0.000000000000000000 ) ) ;
#6783 = CARTESIAN_POINT ( 'NONE',  ( -0.2813450144774474748, -7.667988119308860817, -6.122077150241856280 ) ) ;
#6784 = CYLINDRICAL_SURFACE ( 'NONE', #20710, 12.10452846326766441 ) ;
#6785 = CARTESIAN_POINT ( 'NONE',  ( -0.05014649552828365914, 215.4116977939061144, 24.24886208192144110 ) ) ;
#6786 = CARTESIAN_POINT ( 'NONE',  ( 10.00000000000000711, 206.9523078486586201, 65.00113791807856956 ) ) ;
#6787 = CARTESIAN_POINT ( 'NONE',  ( 0.05014649552810505201, 217.5146222423826714, 49.25113791807857666 ) ) ;
#6788 = CARTESIAN_POINT ( 'NONE',  ( 38.31132485994280756, 169.2658477444273331, 4.635254915624208216 ) ) ;
#6789 = CARTESIAN_POINT ( 'NONE',  ( -10.00000000000000711, 207.0476921513413515, 15.50113791807856600 ) ) ;
#6790 = CARTESIAN_POINT ( 'NONE',  ( -8.000000000000008882, 207.0476921513413515, 3.501137918078566003 ) ) ;
#6791 = CARTESIAN_POINT ( 'NONE',  ( 47.02499999726881441, 149.9369285172503510, -15.58253175000000823 ) ) ;
#6792 = FACE_BOUND ( 'NONE', #21223, .T. ) ;
#6793 = CARTESIAN_POINT ( 'NONE',  ( 0.000000000000000000, 0.000000000000000000, -2.874600000000001376 ) ) ;
#6794 = CARTESIAN_POINT ( 'NONE',  ( -9.680171189290831535, 214.0920067884431148, 30.80113791807857027 ) ) ;
#6795 = DIRECTION ( 'NONE',  ( 0.000000000000000000, -0.4999999999999994449, 0.8660254037844389297 ) ) ;
#6796 = CARTESIAN_POINT ( 'NONE',  ( -8.118202686958039038, 201.1607312380087080, 72.20113791807857240 ) ) ;
#6797 = EDGE_CURVE ( 'NONE', #8990, #8808, #7277, .T. ) ;
#6798 = CARTESIAN_POINT ( 'NONE',  ( 10.01549611932653860, 210.2015048109876716, 46.85113791807856387 ) ) ;
#6799 = CARTESIAN_POINT ( 'NONE',  ( 0.000000000000000000, -2.342598717236903383, 4.057500000000001883 ) ) ;
#6800 = CARTESIAN_POINT ( 'NONE',  ( -2.343682934607786539, -2.688325911136476343, -2.870065989602846201 ) ) ;
#6801 = CARTESIAN_POINT ( 'NONE',  ( 12.00000000000000711, 207.0476921513415220, 12.99886208192143400 ) ) ;
#6802 = CARTESIAN_POINT ( 'NONE',  ( -0.05014649552828402690, 217.5146222423826714, 18.24886208192143755 ) ) ;
#6803 = CARTESIAN_POINT ( 'NONE',  ( 68.29999999453761461, 167.3344367211045096, -8.961492836873482304 ) ) ;
#6804 = EDGE_LOOP ( 'NONE', ( #7511, #31697 ) ) ;
#6805 = CARTESIAN_POINT ( 'NONE',  ( -12.00000000000000711, 207.0476921513413515, 60.50113791807856956 ) ) ;
#6806 = EDGE_CURVE ( 'NONE', #1695, #22398, #11697, .T. ) ;
#6807 = CARTESIAN_POINT ( 'NONE',  ( 6.444103211791042618, 202.2591342207267644, 68.30113791807856671 ) ) ;
#6808 = CARTESIAN_POINT ( 'NONE',  ( -8.118202686958138514, 212.8392687619910930, 35.79886208192143471 ) ) ;
#6809 = DIRECTION ( 'NONE',  ( 1.000000000000000000, -0.000000000000000000, -0.000000000000000000 ) ) ;
#6810 = EDGE_LOOP ( 'NONE', ( #2776, #9117, #319, #4728, #16479, #25371 ) ) ;
#6811 = EDGE_CURVE ( 'NONE', #18459, #17539, #28054, .T. ) ;
#6812 = CARTESIAN_POINT ( 'NONE',  ( -6.139770520408369237, 215.5359834540460042, 87.95113791807858661 ) ) ;
#6813 = VERTEX_POINT ( 'NONE', #1801 ) ;
#6814 = CARTESIAN_POINT ( 'NONE',  ( -54.50000000000002132, 155.0000000000000000, -17.00000000000000000 ) ) ;
#6815 = DIRECTION ( 'NONE',  ( 0.000000000000000000, 0.000000000000000000, -1.000000000000000000 ) ) ;
#6816 = ORIENTED_EDGE ( 'NONE', *, *, #5748, .F. ) ;
#6817 = CARTESIAN_POINT ( 'NONE',  ( 4.984841277089725686, 213.7757310962907411, 28.55113791807857027 ) ) ;
#6818 = EDGE_CURVE ( 'NONE', #10366, #21724, #28217, .T. ) ;
#6819 = DIRECTION ( 'NONE',  ( -1.000000000000000000, -0.000000000000000000, -0.000000000000000000 ) ) ;
#6820 = B_SPLINE_CURVE_WITH_KNOTS ( 'NONE', 3,
 ( #20503, #23225, #25786, #30905, #28841, #23401 ),
 .UNSPECIFIED., .F., .F.,
 ( 4, 2, 4 ),
 ( 0.005649496001316488963, 0.006672230966438344631, 0.007694965931560200298 ),
 .UNSPECIFIED. ) ;
#6821 = CARTESIAN_POINT ( 'NONE',  ( -3.044812012439970683, 197.4746971517856196, 10.89886208192143613 ) ) ;
#6822 = CARTESIAN_POINT ( 'NONE',  ( 59.07499999726880446, 141.7447067706911810, -9.630534252274387086 ) ) ;
#6823 = ORIENTED_EDGE ( 'NONE', *, *, #14588, .T. ) ;
#6824 = CARTESIAN_POINT ( 'NONE',  ( 6.444103211791042618, 202.2591342207267644, 50.30113791807858092 ) ) ;
#6825 = PLANE ( 'NONE',  #14537 ) ;
#6826 = CARTESIAN_POINT ( 'NONE',  ( 60.63708498984762940, 155.0000000000000000, 40.00000000000001421 ) ) ;
#6827 = CARTESIAN_POINT ( 'NONE',  ( 8.118202686958138514, 201.1607312380088501, 103.2988620819214418 ) ) ;
#6828 = EDGE_CURVE ( 'NONE', #25971, #15698, #21690, .T. ) ;
#6829 = CARTESIAN_POINT ( 'NONE',  ( 61.07499999726881867, 141.7447067706911810, -9.630534252274385310 ) ) ;
#6830 = CARTESIAN_POINT ( 'NONE',  ( -9.984503880673473830, 210.2968891136704315, 30.65113791807856813 ) ) ;
#6831 = CYLINDRICAL_SURFACE ( 'NONE', #23613, 7.500000000000015099 ) ;
#6832 = CARTESIAN_POINT ( 'NONE',  ( -6.139770520408369237, 215.5359834540460042, 18.95113791807856884 ) ) ;
#6833 = DIRECTION ( 'NONE',  ( 6.123233995736766036E-17, 0.000000000000000000, -1.000000000000000000 ) ) ;
#6834 = CARTESIAN_POINT ( 'NONE',  ( 79.50000000000000000, 155.0000000000000000, 14.49999999999999467 ) ) ;
#6835 = CARTESIAN_POINT ( 'NONE',  ( 0.000000000000000000, 0.000000000000000000, -9.999999999999998224 ) ) ;
#6836 = DIRECTION ( 'NONE',  ( 1.000000000000000000, 0.000000000000000000, 0.000000000000000000 ) ) ;
#6837 = CARTESIAN_POINT ( 'NONE',  ( 11.98450388067348271, 203.0532714938637753, 5.151137918078566358 ) ) ;
#6838 = DIRECTION ( 'NONE',  ( -0.5000000000000006661, 0.8660254037844382635, 0.000000000000000000 ) ) ;
#6839 = CARTESIAN_POINT ( 'NONE',  ( 44.67499999726881299, 141.7447067706911810, 9.630534252274376428 ) ) ;
#6840 = CARTESIAN_POINT ( 'NONE',  ( -6.139770520408369237, 215.5359834540460042, 45.95113791807857950 ) ) ;
#6841 = CARTESIAN_POINT ( 'NONE',  ( 85.72499999726882436, 169.8198683612136222, 4.815267126137181997 ) ) ;
#6842 = CARTESIAN_POINT ( 'NONE',  ( 125.5000000000000000, 261.0000000000000000, 2.149999999999985256 ) ) ;
#6843 = LINE ( 'NONE', #22341, #481 ) ;
#6844 = CARTESIAN_POINT ( 'NONE',  ( 49.79999999453762882, 146.4771138417591203, -11.73074641843674470 ) ) ;
#6845 = EDGE_LOOP ( 'NONE', ( #3244, #4598 ) ) ;
#6846 = CARTESIAN_POINT ( 'NONE',  ( 11.98450388067348271, 203.0532714938637753, 29.15113791807857169 ) ) ;
#6847 = CARTESIAN_POINT ( 'NONE',  ( 32.50000000000000000, 155.0000000000000000, -6.938893903907228378E-15 ) ) ;
#6848 = FACE_OUTER_BOUND ( 'NONE', #11014, .T. ) ;
#6849 = ORIENTED_EDGE ( 'NONE', *, *, #32692, .F. ) ;
#6850 = CARTESIAN_POINT ( 'NONE',  ( -12.01549611932659722, 210.8513442034533227, 44.64886208192143613 ) ) ;
#6851 = CARTESIAN_POINT ( 'NONE',  ( -0.05014649552810635652, 196.4853777576173002, -0.2488620819214343305 ) ) ;
#6852 = CARTESIAN_POINT ( 'NONE',  ( -10.01549611932653860, 203.7984951890123284, 63.35113791807857098 ) ) ;
#6853 = CARTESIAN_POINT ( 'NONE',  ( -7.984503880673422316, 204.3529502787951628, 23.34886208192143542 ) ) ;
#6854 = ADVANCED_FACE ( 'NONE', ( #7092 ), #30381, .F. ) ;
#6855 = DIRECTION ( 'NONE',  ( -0.000000000000000000, 1.000000000000000000, 1.224646799147353207E-16 ) ) ;
#6856 = VERTEX_POINT ( 'NONE', #33155 ) ;
#6857 = CARTESIAN_POINT ( 'NONE',  ( -2.517493886308901807, 199.4062855549015012, 2.901137918078565914 ) ) ;
#6858 = EDGE_CURVE ( 'NONE', #12674, #17539, #21956, .T. ) ;
#6859 = DIRECTION ( 'NONE',  ( 1.000000000000000000, 0.000000000000000000, 0.000000000000000000 ) ) ;
#6860 = AXIS2_PLACEMENT_3D ( 'NONE', #22595, #25321, #7618 ) ;
#6861 = CARTESIAN_POINT ( 'NONE',  ( -3.662846001189865142, 195.5725841191952838, 88.89886208192143613 ) ) ;
#6862 = CARTESIAN_POINT ( 'NONE',  ( 5.759474945355412601, 0.000000000000000000, 0.000000000000000000 ) ) ;
#6863 = ORIENTED_EDGE ( 'NONE', *, *, #13724, .F. ) ;
#6864 = CARTESIAN_POINT ( 'NONE',  ( 43.92499999726881299, 164.1591823560292198, 12.60653300113718167 ) ) ;
#6865 = CARTESIAN_POINT ( 'NONE',  ( 10.40000000000000036, 0.000000000000000000, 0.000000000000000000 ) ) ;
#6866 = FACE_OUTER_BOUND ( 'NONE', #28324, .T. ) ;
#6867 = CARTESIAN_POINT ( 'NONE',  ( 9.984503880673420539, 210.2968891136705167, 57.84886208192143897 ) ) ;
#6868 = EDGE_CURVE ( 'NONE', #16155, #2927, #11335, .T. ) ;
#6869 = CARTESIAN_POINT ( 'NONE',  ( 41.47499999726880304, 160.0630714827496206, -15.58253175000000823 ) ) ;
#6870 = PLANE ( 'NONE',  #12389 ) ;
#6871 = CARTESIAN_POINT ( 'NONE',  ( 3.044812012440130555, 197.4746971517856764, -0.3988620819214342972 ) ) ;
#6872 = CARTESIAN_POINT ( 'NONE',  ( 6.500000000000000000, 0.6470732608156823940, -0.01945970098673075951 ) ) ;
#6873 = CARTESIAN_POINT ( 'NONE',  ( 59.79999999999999716, 142.6655632788954620, 8.961492836873471646 ) ) ;
#6874 = DIRECTION ( 'NONE',  ( -1.000000000000000000, 0.000000000000000000, 0.000000000000000000 ) ) ;
#6875 = CARTESIAN_POINT ( 'NONE',  ( -4.903702542908436435, 200.1653181626580249, 80.04886208192144181 ) ) ;
#6876 = CARTESIAN_POINT ( 'NONE',  ( 32.50000000000000000, 155.0000000000000000, -6.938893903907228378E-15 ) ) ;
#6877 = DIRECTION ( 'NONE',  ( 0.000000000000000000, 0.9988620819214357738, 0.04769215134144196705 ) ) ;
#6878 = CARTESIAN_POINT ( 'NONE',  ( -0.05014649552828442242, 219.6175466908591716, 84.24886208192143044 ) ) ;
#6879 = CARTESIAN_POINT ( 'NONE',  ( 62.82499999726881867, 141.7447067706911810, -9.630534252274385310 ) ) ;
#6881 = ORIENTED_EDGE ( 'NONE', *, *, #27020, .T. ) ;
#6880 = CARTESIAN_POINT ( 'NONE',  ( 0.05014649552810506589, 217.5146222423826714, 19.25113791807856600 ) ) ;
#6882 = CYLINDRICAL_SURFACE ( 'NONE', #9197, 40.00000000000000711 ) ;
#6883 = CARTESIAN_POINT ( 'NONE',  ( 81.07499999726880446, 141.7447067706911810, -9.630534252274385310 ) ) ;
#6884 = CARTESIAN_POINT ( 'NONE',  ( 7.375838497908181246, 196.7627149292499666, 83.45113791807857240 ) ) ;
#6885 = DIRECTION ( 'NONE',  ( 0.000000000000000000, 1.000000000000000000, -3.227392513445244800E-15 ) ) ;
#6886 = AXIS2_PLACEMENT_3D ( 'NONE', #3447, #26780, #18625 ) ;
#6887 = EDGE_LOOP ( 'NONE', ( #8449, #31579 ) ) ;
#6888 = CARTESIAN_POINT ( 'NONE',  ( -9.736236675708031640, 214.0148392665760753, 71.79886208192142760 ) ) ;
#6889 = CLOSED_SHELL ( 'NONE', ( #16015, #28692, #23967, #764, #22279, #20964, #21242, #32054, #22481, #16585, #26023, #2047, #23326, #4685, #3279, #5201, #29139, #4277, #6236, #3028, #24156, #9967, #445, #8141, #18499, #21885, #30768, #16053, #10412, #6854, #11378, #16941, #25587, #14513, #14358, #23296, #25356, #18137, #5994, #27182, #21473, #24496, #23342, #28496, #9123, #1753, #10464, #28128, #24367, #13139, #32828, #2853, #31257, #9493, #29920, #17866, #14478, #13898, #6901, #17085, #27664, #32558, #13294, #14774, #13459, #26384, #15813, #23871 ) ) ;
#6890 = CARTESIAN_POINT ( 'NONE',  ( -6.139770520408224463, 198.4640165459539105, 77.04886208192144181 ) ) ;
#6891 = CARTESIAN_POINT ( 'NONE',  ( 7.456977232089471386, 196.8216656703012006, 13.44886208192143684 ) ) ;
#6892 = CARTESIAN_POINT ( 'NONE',  ( 117.5000000000000000, 155.0000000000000000, -6.938893903907228378E-15 ) ) ;
#6893 = CARTESIAN_POINT ( 'NONE',  ( -6.220909254589537696, 198.5229672870051161, 33.05113791807857382 ) ) ;
#6894 = DIRECTION ( 'NONE',  ( 0.5526942671207023539, 0.1536855300543050473, 0.8190908404712123891 ) ) ;
#6895 = CARTESIAN_POINT ( 'NONE',  ( 8.062137200540822946, 212.9164362838583315, 96.69886208192143329 ) ) ;
#6896 = ADVANCED_FACE ( 'NONE', ( #10158 ), #7772, .T. ) ;
#6897 = LINE ( 'NONE', #22742, #31182 ) ;
#6898 = VERTEX_POINT ( 'NONE', #17991 ) ;
#6899 = PLANE ( 'NONE',  #21108 ) ;
#6900 = CARTESIAN_POINT ( 'NONE',  ( -4.903702542908436435, 200.1653181626580249, 71.04886208192142760 ) ) ;
#6901 = ADVANCED_FACE ( 'NONE', ( #30770 ), #12456, .T. ) ;
#6902 = VERTEX_POINT ( 'NONE', #28383 ) ;
#6903 = ADVANCED_FACE ( 'NONE', ( #25827 ), #2491, .T. ) ;
#6904 = CARTESIAN_POINT ( 'NONE',  ( 81.22499999726881015, 160.0630714827496206, -15.58253175000000823 ) ) ;
#6905 = ORIENTED_EDGE ( 'NONE', *, *, #19495, .T. ) ;
#6906 = CARTESIAN_POINT ( 'NONE',  ( 93.60208470531338776, 155.0000000000000000, 12.00000000000001066 ) ) ;
#6907 = AXIS2_PLACEMENT_3D ( 'NONE', #11602, #9040, #29836 ) ;
#6908 = CARTESIAN_POINT ( 'NONE',  ( 76.82499999726881867, 141.7447067706911810, -9.630534252274385310 ) ) ;
#6909 = CARTESIAN_POINT ( 'NONE',  ( 63.71132485994279904, 155.0000000000000000, -15.00000000000002487 ) ) ;
#6910 = CARTESIAN_POINT ( 'NONE',  ( 4.903702542908601636, 200.1653181626581102, 74.45113791807855819 ) ) ;
#6911 = CARTESIAN_POINT ( 'NONE',  ( 127.5000000000000000, 155.0000000000000000, 98.00000000000000000 ) ) ;
#6912 = COLOUR_RGB ( '', 0.66274510, 0.83137255, 0.94901961) ;
#6913 = AXIS2_PLACEMENT_3D ( 'NONE', #21646, #24375, #21311 ) ;
#6914 = CARTESIAN_POINT ( 'NONE',  ( 42.60000000000000142, 159.7113355953771077, -14.50000000000000888 ) ) ;
#6915 = CARTESIAN_POINT ( 'NONE',  ( 8.015496119326595448, 204.4483345814782638, 52.14886208192145034 ) ) ;
#6916 = CIRCLE ( 'NONE', #2010, 5.250000000000004441 ) ;
#6917 = FACE_OUTER_BOUND ( 'NONE', #26797, .T. ) ;
#6918 = CARTESIAN_POINT ( 'NONE',  ( -7.703920929261752981, 4.447860822324863683, -7.917989418073281271 ) ) ;
#6919 = CARTESIAN_POINT ( 'NONE',  ( 72.99495483890930814, 155.0000000000000000, -6.938893903907228378E-15 ) ) ;
#6920 = CARTESIAN_POINT ( 'NONE',  ( 47.92499999726881299, 164.1591823560292198, 12.60653300113718167 ) ) ;
#6921 = CARTESIAN_POINT ( 'NONE',  ( 64.57499999726881867, 145.8408176439707802, 12.60653300113718345 ) ) ;
#6922 = CARTESIAN_POINT ( 'NONE',  ( 9.736236675707914401, 214.0148392665762458, 58.70113791807857240 ) ) ;
#6923 = CARTESIAN_POINT ( 'NONE',  ( -64.50000000000000000, 0.000000000000000000, 20.00000000000000000 ) ) ;
#6924 = CARTESIAN_POINT ( 'NONE',  ( -7.375838497908182134, 217.2372850707499765, 0.9511379180785655141 ) ) ;
#6925 = CARTESIAN_POINT ( 'NONE',  ( -6.139770520408368348, 215.5359834540460042, 81.95113791807855819 ) ) ;
#6926 = CARTESIAN_POINT ( 'NONE',  ( -0.05014649552828442242, 219.6175466908591716, 45.24886208192143755 ) ) ;
#6927 = CARTESIAN_POINT ( 'NONE',  ( -9.984503880673420539, 203.7031108863293980, 50.34886208192143187 ) ) ;
#6928 = FACE_OUTER_BOUND ( 'NONE', #33471, .T. ) ;
#6929 = CARTESIAN_POINT ( 'NONE',  ( 12.00000000000000711, 206.9523078486586485, 83.00113791807856956 ) ) ;
#6930 = LINE ( 'NONE', #16687, #30055 ) ;
#6931 = AXIS2_PLACEMENT_3D ( 'NONE', #21773, #27057, #11065 ) ;
#6932 = CARTESIAN_POINT ( 'NONE',  ( -6.220909254589537696, 198.5229672870051161, 6.051137918078566713 ) ) ;
#6933 = CARTESIAN_POINT ( 'NONE',  ( 10.01549611932659545, 203.7984951890123853, 73.14886208192143613 ) ) ;
#6934 = CONICAL_SURFACE ( 'NONE', #29795, 11.99999999999998224, 0.1047197551196726167 ) ;
#6935 = DIRECTION ( 'NONE',  ( 0.000000000000000000, 0.000000000000000000, 1.000000000000000000 ) ) ;
#6936 = VERTEX_POINT ( 'NONE', #15258 ) ;
#6937 = CARTESIAN_POINT ( 'NONE',  ( -9.680171189290716072, 199.9079932115567146, 74.19886208192143329 ) ) ;
#6938 = PRESENTATION_LAYER_ASSIGNMENT (  '', '', ( #5310 ) ) ;
#6939 = AXIS2_PLACEMENT_3D ( 'NONE', #14707, #27158, #24772 ) ;
#6940 = ORIENTED_EDGE ( 'NONE', *, *, #10432, .T. ) ;
#6941 = CARTESIAN_POINT ( 'NONE',  ( 72.67499999726881299, 141.7447067706911810, 9.630534252274376428 ) ) ;
#6942 = CARTESIAN_POINT ( 'NONE',  ( 2.426778023690075337, 214.6231898156240447, 42.39886208192144323 ) ) ;
#6943 = ORIENTED_EDGE ( 'NONE', *, *, #16321, .F. ) ;
#6944 = AXIS2_PLACEMENT_3D ( 'NONE', #29705, #21865, #32597 ) ;
#6945 = CARTESIAN_POINT ( 'NONE',  ( 81.47499999726879594, 160.0630714827496206, -15.58253175000000823 ) ) ;
#6946 = DIRECTION ( 'NONE',  ( -1.000000000000000000, -0.000000000000000000, -0.000000000000000000 ) ) ;
#6947 = DIRECTION ( 'NONE',  ( -0.000000000000000000, -0.000000000000000000, 1.000000000000000000 ) ) ;
#6948 = CARTESIAN_POINT ( 'NONE',  ( 59.22499999726879594, 160.0630714827496206, -15.58253175000000823 ) ) ;
#6949 = PLANE ( 'NONE',  #25418 ) ;
#6950 = CARTESIAN_POINT ( 'NONE',  ( -3.044812012439970683, 197.4746971517856196, 40.89886208192143613 ) ) ;
#6951 = ORIENTED_EDGE ( 'NONE', *, *, #16005, .F. ) ;
#6952 = CARTESIAN_POINT ( 'NONE',  ( 0.000000000000000000, 0.000000000000000000, 0.000000000000000000 ) ) ;
#6953 = SHAPE_REPRESENTATION_RELATIONSHIP ( 'NONE' , 'NONE' ,  #17605, #9595 ) ;
#6954 = CARTESIAN_POINT ( 'NONE',  ( 5.000000000000000000, 4.685197434473814759, -5.637851296924623057E-15 ) ) ;
#6955 = CARTESIAN_POINT ( 'NONE',  ( 0.000000000000000000, 1.773042676681340968, -2.276824562219559311E-15 ) ) ;
#6956 = CARTESIAN_POINT ( 'NONE',  ( 7.984503880673422316, 209.6470497212048372, 27.84886208192143897 ) ) ;
#6957 = CONICAL_SURFACE ( 'NONE', #26006, 31.00000000000000000, 1.466076571675244411 ) ;
#6958 = CARTESIAN_POINT ( 'NONE',  ( -6.220909254589537696, 198.5229672870051161, 57.05113791807857382 ) ) ;
#6959 = B_SPLINE_CURVE_WITH_KNOTS ( 'NONE', 3,
 ( #1072, #29180, #10961, #733, #5832, #21509 ),
 .UNSPECIFIED., .F., .F.,
 ( 4, 2, 4 ),
 ( 0.003605240635278498650, 0.004627368318297494024, 0.005649496001316488963 ),
 .UNSPECIFIED. ) ;
#6960 = CARTESIAN_POINT ( 'NONE',  ( 10.00000000000000711, 206.9523078486586201, 47.00113791807856956 ) ) ;
#6961 = CARTESIAN_POINT ( 'NONE',  ( 70.81132485994281467, 150.1262045565064227, 15.00000000000001599 ) ) ;
#6962 = VECTOR ( 'NONE', #15321, 1000.000000000000000 ) ;
#6963 = CIRCLE ( 'NONE', #26011, 12.00000000000000355 ) ;
#6964 = CARTESIAN_POINT ( 'NONE',  ( 6.139770520408368348, 198.4640165459539674, 17.45113791807855819 ) ) ;
#6965 = CARTESIAN_POINT ( 'NONE',  ( -4.984841277089726574, 200.2242689037092305, 3.051137918078566269 ) ) ;
#6966 = CARTESIAN_POINT ( 'NONE',  ( 45.42499999726879878, 168.2552932293087906, -9.630534252274385310 ) ) ;
#6967 = DIRECTION ( 'NONE',  ( 0.000000000000000000, 0.000000000000000000, -1.000000000000000000 ) ) ;
#6968 = DIRECTION ( 'NONE',  ( 1.000000000000000000, 0.000000000000000000, 0.000000000000000000 ) ) ;
#6969 = CARTESIAN_POINT ( 'NONE',  ( 12.01549611932652972, 210.8513442034534933, 31.85113791807857453 ) ) ;
#6970 = DIRECTION ( 'NONE',  ( 1.000000000000000000, 0.000000000000000000, 0.000000000000000000 ) ) ;
#6971 = CARTESIAN_POINT ( 'NONE',  ( 6.220909254589536808, 215.4770327129947702, 79.55113791807855250 ) ) ;
#6972 = CARTESIAN_POINT ( 'NONE',  ( 0.05014649552810506589, 217.5146222423826714, 49.25113791807856956 ) ) ;
#6973 = VECTOR ( 'NONE', #25355, 1000.000000000000000 ) ;
#6974 = CARTESIAN_POINT ( 'NONE',  ( -64.50000000000000000, 155.0000000000000000, 6.938893903907228378E-15 ) ) ;
#6975 = CARTESIAN_POINT ( 'NONE',  ( 35.48867513459483547, 167.7597621252805880, 9.270509831248428867 ) ) ;
#6976 = CARTESIAN_POINT ( 'NONE',  ( -0.05014649552828442242, 219.6175466908591716, 12.24886208192143577 ) ) ;
#6977 = CARTESIAN_POINT ( 'NONE',  ( -3.135527875058982783, 216.4958274776886924, 18.09886208192143542 ) ) ;
#6978 = CARTESIAN_POINT ( 'NONE',  ( 72.39999999453763735, 168.7903194862797420, -4.480746418436745593 ) ) ;
#6979 = ORIENTED_EDGE ( 'NONE', *, *, #27629, .F. ) ;
#6980 = CARTESIAN_POINT ( 'NONE',  ( -12.00000000000000711, 207.0476921513413515, 57.50113791807856956 ) ) ;
#6981 = CARTESIAN_POINT ( 'NONE',  ( 2.426778023690261410, 199.3768101843759837, 83.60113791807857808 ) ) ;
#6982 = CARTESIAN_POINT ( 'NONE',  ( -10.00000000000000711, 206.9523078486584495, 32.49886208192143044 ) ) ;
#6983 = CARTESIAN_POINT ( 'NONE',  ( 76.51132485994280330, 163.8167787843871110, 12.13525491562421621 ) ) ;
#6984 = ORIENTED_EDGE ( 'NONE', *, *, #27838, .F. ) ;
#6985 = VERTEX_POINT ( 'NONE', #18493 ) ;
#6986 = EDGE_LOOP ( 'NONE', ( #2282, #30319, #13558, #8732 ) ) ;
#6987 = PRODUCT_DEFINITION_SHAPE ( 'NONE', 'NONE',  #12945 ) ;
#6988 = VECTOR ( 'NONE', #18723, 1000.000000000000000 ) ;
#6989 = LINE ( 'NONE', #24870, #3693 ) ;
#6990 = DIRECTION ( 'NONE',  ( -1.000000000000000000, -0.000000000000000000, -0.000000000000000000 ) ) ;
#6991 = VERTEX_POINT ( 'NONE', #20882 ) ;
#6992 = CARTESIAN_POINT ( 'NONE',  ( -2.517493886308901807, 199.4062855549015012, 29.90113791807857169 ) ) ;
#6993 = CARTESIAN_POINT ( 'NONE',  ( 85.21132485994283456, 139.2280666364260071, -4.041636747397287284E-15 ) ) ;
#6994 = EDGE_CURVE ( 'NONE', #13849, #25466, #5041, .T. ) ;
#6995 = CARTESIAN_POINT ( 'NONE',  ( -3.135527875058982783, 216.4958274776886924, 18.09886208192143542 ) ) ;
#6996 = CARTESIAN_POINT ( 'NONE',  ( 54.17499999726881299, 164.1591823560292198, 12.60653300113718167 ) ) ;
#6998 = ORIENTED_EDGE ( 'NONE', *, *, #25390, .T. ) ;
#6997 = VECTOR ( 'NONE', #27239, 1000.000000000000000 ) ;
#6999 = CARTESIAN_POINT ( 'NONE',  ( 2.517493886308900919, 214.5937144450984420, 52.40113791807858235 ) ) ;
#7000 = DIRECTION ( 'NONE',  ( 0.000000000000000000, 0.000000000000000000, -1.000000000000000000 ) ) ;
#7001 = CARTESIAN_POINT ( 'NONE',  ( 57.61132485994281183, 150.1262045565064227, -15.00000000000002665 ) ) ;
#7002 = CARTESIAN_POINT ( 'NONE',  ( 8.118202686958138514, 201.1607312380088501, 100.2988620819214418 ) ) ;
#7003 = CARTESIAN_POINT ( 'NONE',  ( 64.77499999726882152, 140.1801316387863778, 4.815267126137185549 ) ) ;
#7004 = CARTESIAN_POINT ( 'NONE',  ( 6.220909254589536808, 215.4770327129947702, 31.55113791807857382 ) ) ;
#7005 = CARTESIAN_POINT ( 'NONE',  ( 3.044812012440130555, 197.4746971517856764, 20.60113791807856742 ) ) ;
#7006 = CARTESIAN_POINT ( 'NONE',  ( 121.5000000000000000, 154.9999999999996305, -106.0000000000000142 ) ) ;
#7007 = CARTESIAN_POINT ( 'NONE',  ( 82.60000000000002274, 159.7113355953771077, -14.50000000000000888 ) ) ;
#7008 = CARTESIAN_POINT ( 'NONE',  ( -57.85233474027615586, 194.9267265987278961, -2.420233332361308332 ) ) ;
#7009 = CARTESIAN_POINT ( 'NONE',  ( 1.750000000000016209, -3.031088913245524985, 0.000000000000000000 ) ) ;
#7010 = CARTESIAN_POINT ( 'NONE',  ( 0.05014649552810505201, 217.5146222423826714, 100.2511379180785838 ) ) ;
#7011 = CARTESIAN_POINT ( 'NONE',  ( 48.78867513459482552, 155.0000000000000000, -15.00000000000002487 ) ) ;
#7012 = CARTESIAN_POINT ( 'NONE',  ( 50.87499999726881583, 138.6155565068815463, -3.929120461958505118E-15 ) ) ;
#7013 = CARTESIAN_POINT ( 'NONE',  ( 8.118202686958039038, 212.8392687619912635, 49.70113791807857240 ) ) ;
#7014 = CARTESIAN_POINT ( 'NONE',  ( 81.82499999726879025, 168.2552932293087906, 9.630534252274372875 ) ) ;
#7015 = CIRCLE ( 'NONE', #1562, 7.500000000000001776 ) ;
#7016 = CARTESIAN_POINT ( 'NONE',  ( 51.71132485994281325, 155.0000000000000000, -15.00000000000002487 ) ) ;
#7017 = ADVANCED_FACE ( 'NONE', ( #8586 ), #19140, .F. ) ;
#7018 = DIRECTION ( 'NONE',  ( 1.000000000000000000, 0.000000000000000000, 0.000000000000000000 ) ) ;
#7019 = CARTESIAN_POINT ( 'NONE',  ( 46.19999999453763451, 163.5228861582408797, -11.73074641843674470 ) ) ;
#7020 = VERTEX_POINT ( 'NONE', #23436 ) ;
#7021 = CARTESIAN_POINT ( 'NONE',  ( 12.01549611932652972, 210.8513442034534933, 31.85113791807857453 ) ) ;
#7022 = CARTESIAN_POINT ( 'NONE',  ( 61.31132485994281467, 140.7341522555726669, -4.635254915624220651 ) ) ;
#7023 = CARTESIAN_POINT ( 'NONE',  ( -9.680171189290716072, 199.9079932115567146, 104.1988620819214475 ) ) ;
#7024 = TOROIDAL_SURFACE ( 'NONE', #2681, 69.99999999999998579, 27.99999999999999645 ) ;
#7025 = CARTESIAN_POINT ( 'NONE',  ( -16.00000000000000000, 1.959434878635765131E-15, -16.57418492358057094 ) ) ;
#7026 = ORIENTED_EDGE ( 'NONE', *, *, #19384, .F. ) ;
#7027 = CARTESIAN_POINT ( 'NONE',  ( 10.00000000000000711, 206.9523078486586201, 5.001137918078565114 ) ) ;
#7028 = CARTESIAN_POINT ( 'NONE',  ( 6.139770520408368348, 198.4640165459539674, 65.45113791807857240 ) ) ;
#7029 = EDGE_CURVE ( 'NONE', #20137, #14046, #6474, .T. ) ;
#7030 = CARTESIAN_POINT ( 'NONE',  ( -6.500168698208244500, 211.6636982574061676, 26.79886208192143826 ) ) ;
#7031 = DIRECTION ( 'NONE',  ( -1.000000000000000000, -0.000000000000000000, -0.000000000000000000 ) ) ;
#7032 = ORIENTED_EDGE ( 'NONE', *, *, #31439, .T. ) ;
#7033 = CARTESIAN_POINT ( 'NONE',  ( 7.984503880673485376, 204.3529502787953902, -0.8488620819214343083 ) ) ;
#7034 = VECTOR ( 'NONE', #21206, 1000.000000000000000 ) ;
#7035 = EDGE_CURVE ( 'NONE', #18384, #27919, #31830, .T. ) ;
#7036 = CARTESIAN_POINT ( 'NONE',  ( -1.206569728928481577, -7.963640680051488729, -0.4524126574264552558 ) ) ;
#7037 = CARTESIAN_POINT ( 'NONE',  ( -0.05014649552828442242, 219.6175466908591716, 87.24886208192144466 ) ) ;
#7038 = CARTESIAN_POINT ( 'NONE',  ( 40.57499999726881157, 145.8408176439707802, 12.60653300113718345 ) ) ;
#7039 = EDGE_LOOP ( 'NONE', ( #11143, #4668 ) ) ;
#7040 = CARTESIAN_POINT ( 'NONE',  ( 43.22499999726881015, 160.0630714827496206, -15.58253175000000823 ) ) ;
#7041 = DIRECTION ( 'NONE',  ( 0.000000000000000000, 0.000000000000000000, 1.000000000000000000 ) ) ;
#7042 = CARTESIAN_POINT ( 'NONE',  ( 2.000000000000000000, -1.773042676681340524, 1.734723475976807094E-15 ) ) ;
#7043 = CARTESIAN_POINT ( 'NONE',  ( -6.220909254589682469, 215.4770327129946850, 71.94886208192144750 ) ) ;
#7044 = CARTESIAN_POINT ( 'NONE',  ( 47.27499999726880731, 149.9369285172503510, -15.58253175000000823 ) ) ;
#7045 = CARTESIAN_POINT ( 'NONE',  ( 32.50000000000000000, 155.0000000000000000, 13.00000000000001066 ) ) ;
#7046 = CARTESIAN_POINT ( 'NONE',  ( 8.118202686958039038, 212.8392687619912635, 7.701137918078566180 ) ) ;
#7047 = CARTESIAN_POINT ( 'NONE',  ( 10.00000000000000178, 9.797174393178825657E-16, -8.000000000000000000 ) ) ;
#7048 =( REPRESENTATION_RELATIONSHIP ('NONE','NONE', #25663, #17198 ) REPRESENTATION_RELATIONSHIP_WITH_TRANSFORMATION ( #2019 )SHAPE_REPRESENTATION_RELATIONSHIP( ) );
#7049 = EDGE_CURVE ( 'NONE', #27176, #32876, #28877, .T. ) ;
#7050 = CARTESIAN_POINT ( 'NONE',  ( 60.20000000000000995, 142.6655632788954620, -8.961492836873480528 ) ) ;
#7051 = CARTESIAN_POINT ( 'NONE',  ( 3.135527875058820690, 216.4958274776887492, 91.40113791807857524 ) ) ;
#7052 = FACE_BOUND ( 'NONE', #9753, .T. ) ;
#7053 = CYLINDRICAL_SURFACE ( 'NONE', #14551, 1.650000000000000133 ) ;
#7054 = CARTESIAN_POINT ( 'NONE',  ( -62.70000000000000284, -88.00000000000000000, -20.00000000000000000 ) ) ;
#7055 = CARTESIAN_POINT ( 'NONE',  ( 3.753561863808876797, 195.6020594897209719, 88.59886208192143897 ) ) ;
#7056 = CARTESIAN_POINT ( 'NONE',  ( 65.92499999726881299, 164.1591823560292198, 12.60653300113718167 ) ) ;
#7058 = ORIENTED_EDGE ( 'NONE', *, *, #23044, .T. ) ;
#7057 = CARTESIAN_POINT ( 'NONE',  ( 8.062137200540920645, 201.0835637161417822, 23.30113791807856671 ) ) ;
#7059 = FACE_OUTER_BOUND ( 'NONE', #2376, .T. ) ;
#7060 = CARTESIAN_POINT ( 'NONE',  ( 83.87499999726878741, 171.3844434931184253, -7.942151717890132712E-15 ) ) ;
#7061 = CARTESIAN_POINT ( 'NONE',  ( 3.662846001190051659, 195.5725841191953691, 86.60113791807857808 ) ) ;
#7062 = AXIS2_PLACEMENT_3D ( 'NONE', #26285, #2959, #23896 ) ;
#7063 = EDGE_CURVE ( 'NONE', #6637, #11134, #10836, .T. ) ;
#7064 = DIRECTION ( 'NONE',  ( 1.000000000000000000, 0.000000000000000000, 0.000000000000000000 ) ) ;
#7065 = EDGE_LOOP ( 'NONE', ( #12126, #5698, #15288, #15233 ) ) ;
#7066 = CARTESIAN_POINT ( 'NONE',  ( 7.456977232089471386, 196.8216656703012006, 73.44886208192143329 ) ) ;
#7067 = CARTESIAN_POINT ( 'NONE',  ( 10.01549611932659367, 203.7984951890124421, 73.14886208192143613 ) ) ;
#7068 = CARTESIAN_POINT ( 'NONE',  ( 12.01549611932659367, 203.1486557965466773, 10.14886208192143435 ) ) ;
#7069 = LINE ( 'NONE', #248, #3956 ) ;
#7070 = CARTESIAN_POINT ( 'NONE',  ( 8.118202686958039038, 212.8392687619912635, 34.70113791807857240 ) ) ;
#7071 = EDGE_CURVE ( 'NONE', #854, #16934, #26084, .T. ) ;
#7072 = DIRECTION ( 'NONE',  ( -1.000000000000000000, -0.000000000000000000, -0.000000000000000000 ) ) ;
#7073 = CARTESIAN_POINT ( 'NONE',  ( -6.139770520408224463, 198.4640165459539389, 101.0488620819214134 ) ) ;
#7074 = LINE ( 'NONE', #7410, #11594 ) ;
#7075 = ORIENTED_EDGE ( 'NONE', *, *, #17645, .T. ) ;
#7076 = FACE_OUTER_BOUND ( 'NONE', #3786, .T. ) ;
#7077 = CARTESIAN_POINT ( 'NONE',  ( 2.426778023690075337, 214.6231898156240447, 81.39886208192143613 ) ) ;
#7078 = ORIENTED_EDGE ( 'NONE', *, *, #25296, .F. ) ;
#7079 = CARTESIAN_POINT ( 'NONE',  ( 3.500000000000004885, -1.355464348821719733, -2.761841578728545965 ) ) ;
#7080 = ORIENTED_EDGE ( 'NONE', *, *, #822, .F. ) ;
#7081 = DIRECTION ( 'NONE',  ( -0.000000000000000000, -0.000000000000000000, 1.000000000000000000 ) ) ;
#7082 = CARTESIAN_POINT ( 'NONE',  ( 77.82499999726880446, 168.2552932293087906, 9.630534252274372875 ) ) ;
#7083 = CARTESIAN_POINT ( 'NONE',  ( 125.5000000000000000, 154.9999999999996305, -106.0000000000000142 ) ) ;
#7084 = CARTESIAN_POINT ( 'NONE',  ( -2.517493886308901807, 199.4062855549015012, 77.90113791807856103 ) ) ;
#7085 = CARTESIAN_POINT ( 'NONE',  ( -3.500000000000001332, 1.693985822988442580, -2.681714356710791947 ) ) ;
#7086 =( NAMED_UNIT ( * ) PLANE_ANGLE_UNIT ( ) SI_UNIT ( $, .RADIAN. ) );
#7087 = CARTESIAN_POINT ( 'NONE',  ( 40.00000000000000711, 139.7537977485451393, -4.138211985947621020E-15 ) ) ;
#7088 = CARTESIAN_POINT ( 'NONE',  ( 6.500168698208244500, 202.3363017425938324, 58.29886208192143471 ) ) ;
#7089 = EDGE_CURVE ( 'NONE', #23658, #2760, #17368, .T. ) ;
#7090 = ADVANCED_FACE ( 'NONE', ( #15761 ), #33126, .F. ) ;
#7091 = CARTESIAN_POINT ( 'NONE',  ( 6.663127973346137267, 3.846958729056316528, -6.460793508093409798 ) ) ;
#7092 = FACE_OUTER_BOUND ( 'NONE', #30878, .T. ) ;
#7093 = DIRECTION ( 'NONE',  ( -1.000000000000000000, -0.000000000000000000, 0.000000000000000000 ) ) ;
#7094 = CARTESIAN_POINT ( 'NONE',  ( 51.32499999726881157, 164.1591823560292198, -12.60653300113719766 ) ) ;
#7095 = CARTESIAN_POINT ( 'NONE',  ( 61.27499999726882152, 149.9369285172503510, -15.58253175000000823 ) ) ;
#7096 = CARTESIAN_POINT ( 'NONE',  ( -12.01549611932652972, 203.1486557965464499, 54.35113791807857098 ) ) ;
#7097 = DIRECTION ( 'NONE',  ( -1.000000000000000000, 0.000000000000000000, 0.000000000000000000 ) ) ;
#7098 = CARTESIAN_POINT ( 'NONE',  ( -10.01549611932653860, 203.7984951890123284, 102.3511379180785781 ) ) ;
#7099 = ADVANCED_FACE ( 'NONE', ( #13206 ), #28372, .F. ) ;
#7100 = CARTESIAN_POINT ( 'NONE',  ( 8.062137200540920645, 201.0835637161417822, 80.30113791807858092 ) ) ;
#7101 = CARTESIAN_POINT ( 'NONE',  ( 12.00000000000000711, 207.0476921513415220, 45.99886208192143755 ) ) ;
#7102 = CARTESIAN_POINT ( 'NONE',  ( -10.01549611932659545, 210.2015048109875011, 44.64886208192142902 ) ) ;
#7103 = CARTESIAN_POINT ( 'NONE',  ( -62.70000000000000284, -88.00000000000000000, -20.00000000000000000 ) ) ;
#7104 = CARTESIAN_POINT ( 'NONE',  ( 7.375838497908181246, 196.7627149292499666, 83.45113791807857240 ) ) ;
#7105 = CARTESIAN_POINT ( 'NONE',  ( 83.71132485994282035, 155.0000000000000000, -15.00000000000002487 ) ) ;
#7106 = CARTESIAN_POINT ( 'NONE',  ( 9.984503880673470277, 203.7031108863295401, -0.8488620819214341973 ) ) ;
#7107 = EDGE_CURVE ( 'NONE', #16763, #31655, #26322, .T. ) ;
#7108 = CARTESIAN_POINT ( 'NONE',  ( -3.135527875058982783, 216.4958274776886924, 69.09886208192143897 ) ) ;
#7109 = CARTESIAN_POINT ( 'NONE',  ( 81.37499999726881583, 155.0000000000000000, -15.58253175000000823 ) ) ;
#7110 = VERTEX_POINT ( 'NONE', #16087 ) ;
#7111 = CARTESIAN_POINT ( 'NONE',  ( 11.98450388067341876, 210.9467285061363953, 75.84886208192143897 ) ) ;
#7112 = VERTEX_POINT ( 'NONE', #2987 ) ;
#7113 = CARTESIAN_POINT ( 'NONE',  ( 80.67499999726881299, 141.7447067706911810, 9.630534252274376428 ) ) ;
#7114 = CARTESIAN_POINT ( 'NONE',  ( -7.984503880673422316, 204.3529502787951628, 56.34886208192144608 ) ) ;
#7115 = ORIENTED_EDGE ( 'NONE', *, *, #13066, .F. ) ;
#7116 = CARTESIAN_POINT ( 'NONE',  ( 71.42499999726879878, 168.2552932293087906, -9.630534252274387086 ) ) ;
#7117 = CARTESIAN_POINT ( 'NONE',  ( 0.000000000000000000, 0.000000000000000000, -17.97459999999999525 ) ) ;
#7118 = DIRECTION ( 'NONE',  ( 1.000000000000000000, 0.000000000000000000, 0.000000000000000000 ) ) ;
#7119 = CARTESIAN_POINT ( 'NONE',  ( 59.72499999726881015, 169.8198683612136222, 4.815267126137181997 ) ) ;
#7120 = CYLINDRICAL_SURFACE ( 'NONE', #4204, 2.149999999999985256 ) ;
#7121 = CARTESIAN_POINT ( 'NONE',  ( 10.00000000000000711, 207.0476921513415220, 45.99886208192143755 ) ) ;
#7122 = ORIENTED_EDGE ( 'NONE', *, *, #26380, .F. ) ;
#7123 = DIRECTION ( 'NONE',  ( 0.000000000000000000, 0.000000000000000000, -1.000000000000000000 ) ) ;
#7124 = FILL_AREA_STYLE_COLOUR ( '', #14916 ) ;
#7125 = FACE_OUTER_BOUND ( 'NONE', #19043, .T. ) ;
#7126 = DIRECTION ( 'NONE',  ( -1.000000000000000000, -0.000000000000000000, 0.000000000000000000 ) ) ;
#7127 = CARTESIAN_POINT ( 'NONE',  ( 6.444103211790928043, 211.7408657792734061, 27.69886208192143684 ) ) ;
#7128 = CARTESIAN_POINT ( 'NONE',  ( 3.135527875058820690, 216.4958274776887492, 70.40113791807857524 ) ) ;
#7129 = DIRECTION ( 'NONE',  ( -1.000000000000000000, -0.000000000000000000, -0.000000000000000000 ) ) ;
#7130 = CARTESIAN_POINT ( 'NONE',  ( 10.01549611932653860, 210.2015048109876716, 49.85113791807857808 ) ) ;
#7131 = CONTEXT_DEPENDENT_SHAPE_REPRESENTATION ( #13353, #16061 ) ;
#7132 = CARTESIAN_POINT ( 'NONE',  ( 8.062137200540920645, 201.0835637161417822, 17.30113791807856671 ) ) ;
#7133 = CARTESIAN_POINT ( 'NONE',  ( -7.984503880673488041, 209.6470497212046098, 6.651137918078566358 ) ) ;
#7134 = CARTESIAN_POINT ( 'NONE',  ( 53.22499999726879594, 160.0630714827496206, -15.58253175000000823 ) ) ;
#7135 = FACE_BOUND ( 'NONE', #2212, .T. ) ;
#7136 = CARTESIAN_POINT ( 'NONE',  ( 125.0000000000000000, 3.061616997868383121E-14, -35.00000000000000000 ) ) ;
#7137 = CARTESIAN_POINT ( 'NONE',  ( 7.375838497908181246, 196.7627149292499666, 29.45113791807856529 ) ) ;
#7138 = CARTESIAN_POINT ( 'NONE',  ( -130.2500000000000000, 6.429395695523609083E-16, -35.00000000000000000 ) ) ;
#7139 = CARTESIAN_POINT ( 'NONE',  ( 9.984503880673470277, 203.7031108863295401, 80.15113791807858945 ) ) ;
#7140 = CARTESIAN_POINT ( 'NONE',  ( -6.139770520408368348, 215.5359834540460042, 45.95113791807857950 ) ) ;
#7141 = LINE ( 'NONE', #1519, #29532 ) ;
#7142 = DIRECTION ( 'NONE',  ( -1.000000000000000000, -0.000000000000000000, -0.000000000000000000 ) ) ;
#7143 = CARTESIAN_POINT ( 'NONE',  ( -12.00000000000000711, 206.9523078486584780, 11.49886208192143577 ) ) ;
#7144 = CARTESIAN_POINT ( 'NONE',  ( -6.139770520408224463, 198.4640165459539105, 20.04886208192143116 ) ) ;
#7145 = AXIS2_PLACEMENT_3D ( 'NONE', #18693, #16919, #15797 ) ;
#7146 = CARTESIAN_POINT ( 'NONE',  ( 73.49999999453763166, 139.7537977485451393, -4.138211985947621020E-15 ) ) ;
#7147 = EDGE_LOOP ( 'NONE', ( #19157, #8854, #31862, #26570, #3456 ) ) ;
#7148 = CARTESIAN_POINT ( 'NONE',  ( -3.662846001190052991, 218.4274158808045740, 61.10113791807857808 ) ) ;
#7149 = CARTESIAN_POINT ( 'NONE',  ( -6.444103211791042618, 211.7408657792732356, 75.80113791807858092 ) ) ;
#7150 = CARTESIAN_POINT ( 'NONE',  ( -8.118202686958138514, 212.8392687619910930, 44.79886208192143471 ) ) ;
#7151 = CARTESIAN_POINT ( 'NONE',  ( 65.25000000000000000, 7.347880794884118356E-15, 20.00000000000000000 ) ) ;
#7152 = VERTEX_POINT ( 'NONE', #21534 ) ;
#7153 = EDGE_LOOP ( 'NONE', ( #3038, #15070, #18142, #25253, #12131 ) ) ;
#7154 = ORIENTED_EDGE ( 'NONE', *, *, #18474, .F. ) ;
#7155 = DIRECTION ( 'NONE',  ( 0.000000000000000000, 0.000000000000000000, -1.000000000000000000 ) ) ;
#7156 = CARTESIAN_POINT ( 'NONE',  ( 0.5204879950541921874, 7.205049615410631603, -0.5609245978742269934 ) ) ;
#7157 = ORIENTED_EDGE ( 'NONE', *, *, #9924, .F. ) ;
#7158 = CARTESIAN_POINT ( 'NONE',  ( -2.517493886308901807, 199.4062855549015012, 32.90113791807857524 ) ) ;
#7159 =( BOUNDED_CURVE ( )  B_SPLINE_CURVE ( 2, ( #7011, #12284, #22676, #9733, #7693, #15349, #13292, #2580, #30864, #12966, #28472 ),
 .UNSPECIFIED., .F., .T. ) 
 B_SPLINE_CURVE_WITH_KNOTS ( ( 3, 2, 2, 2, 2, 3 ),
 ( 0.6964285714285712858, 0.6999999999999998446, 0.7035714285714284033, 0.7071428571428569620, 0.7107142857142855208, 0.7142857142857140795 ),
 .UNSPECIFIED. ) 
 CURVE ( )  GEOMETRIC_REPRESENTATION_ITEM ( )  RATIONAL_B_SPLINE_CURVE ( ( 1.000000000000001554, 0.9510565162951518658, 1.000000000000000000, 0.9510565162951534202, 1.000000000000000000, 0.9510565162951534202, 1.000000000000000000, 0.9510565162951534202, 1.000000000000000000, 0.9510565162951549745, 0.9999999999999984457 ) ) 
 REPRESENTATION_ITEM ( '' )  );
#7160 = CARTESIAN_POINT ( 'NONE',  ( 77.50000000000000000, 155.0000000000000000, 13.50000000000000355 ) ) ;
#7161 = CARTESIAN_POINT ( 'NONE',  ( 8.118202686958138514, 201.1607312380088501, 13.29886208192143648 ) ) ;
#7162 = CARTESIAN_POINT ( 'NONE',  ( 59.37499999726881583, 155.0000000000000000, -15.58253175000000823 ) ) ;
#7163 = ORIENTED_EDGE ( 'NONE', *, *, #27591, .T. ) ;
#7164 = CARTESIAN_POINT ( 'NONE',  ( 4.984841277089725686, 213.7757310962907411, 55.55113791807858092 ) ) ;
#7165 = CARTESIAN_POINT ( 'NONE',  ( 67.21132485994282035, 139.2280666364260071, -4.041636747397287284E-15 ) ) ;
#7166 = AXIS2_PLACEMENT_3D ( 'NONE', #33449, #10120, #2451 ) ;
#7167 =( NAMED_UNIT ( * ) SI_UNIT ( $, .STERADIAN. ) SOLID_ANGLE_UNIT ( ) );
#7168 = CARTESIAN_POINT ( 'NONE',  ( 34.49999999999999289, -72.99999999999998579, 30.00000000000000000 ) ) ;
#7169 = CARTESIAN_POINT ( 'NONE',  ( 0.05014649552828275708, 196.4853777576173002, 103.7488620819214589 ) ) ;
#7170 = CARTESIAN_POINT ( 'NONE',  ( 63.87499999726881583, 171.3844434931184253, -7.942151717890132712E-15 ) ) ;
#7171 = CARTESIAN_POINT ( 'NONE',  ( 8.062137200540920645, 201.0835637161417822, 35.30113791807857382 ) ) ;
#7172 = CARTESIAN_POINT ( 'NONE',  ( -4.927659837809095222, 206.3103720916592465, -5.504302862921502282 ) ) ;
#7173 = CARTESIAN_POINT ( 'NONE',  ( 3.135527875058820690, 216.4958274776887492, 13.40113791807856636 ) ) ;
#7174 = DIRECTION ( 'NONE',  ( 0.000000000000000000, 1.000000000000000000, -1.047444401652940007E-14 ) ) ;
#7175 = AXIS2_PLACEMENT_3D ( 'NONE', #9420, #14526, #17423 ) ;
#7176 = CARTESIAN_POINT ( 'NONE',  ( 78.70000000000000284, 163.5228861582408797, -11.73074641843674470 ) ) ;
#7177 = DIRECTION ( 'NONE',  ( -1.000000000000000000, 0.000000000000000000, 0.000000000000000000 ) ) ;
#7178 = DIRECTION ( 'NONE',  ( 1.000000000000000000, 0.000000000000000000, 0.000000000000000000 ) ) ;
#7179 = CARTESIAN_POINT ( 'NONE',  ( -3.662846001190052991, 218.4274158808045740, 4.101137918078565647 ) ) ;
#7180 = CARTESIAN_POINT ( 'NONE',  ( -5.357619327558936585E-16, 7.505553499465137612, -8.000000000000000000 ) ) ;
#7181 = CARTESIAN_POINT ( 'NONE',  ( 52.27499999726880020, 160.0630714827496206, 15.58253174999999402 ) ) ;
#7182 = CARTESIAN_POINT ( 'NONE',  ( 3.044812012440130555, 197.4746971517856764, 44.60113791807857098 ) ) ;
#7183 = CARTESIAN_POINT ( 'NONE',  ( 81.62499999726878741, 171.3844434931184253, -7.942151717890132712E-15 ) ) ;
#7184 = CYLINDRICAL_SURFACE ( 'NONE', #19016, 17.00000000000000355 ) ;
#7185 = CARTESIAN_POINT ( 'NONE',  ( -2.499999999999999556, -7.216878364870334295, -7.063244554130003294 ) ) ;
#7186 = CARTESIAN_POINT ( 'NONE',  ( 54.29999999453762172, 167.3344367211045096, -8.961492836873482304 ) ) ;
#7187 = ORIENTED_EDGE ( 'NONE', *, *, #31448, .T. ) ;
#7188 = CARTESIAN_POINT ( 'NONE',  ( 9.736236675707914401, 214.0148392665762458, 25.70113791807857240 ) ) ;
#7189 = CARTESIAN_POINT ( 'NONE',  ( 37.58867513459482268, 163.8167787843871110, 12.13525491562421621 ) ) ;
#7190 = ADVANCED_FACE ( 'NONE', ( #21870 ), #6200, .F. ) ;
#7191 = CARTESIAN_POINT ( 'NONE',  ( -3.044812012439970683, 197.4746971517856196, 13.89886208192143613 ) ) ;
#7192 = DIRECTION ( 'NONE',  ( -0.000000000000000000, -0.000000000000000000, 1.000000000000000000 ) ) ;
#7193 = ORIENTED_EDGE ( 'NONE', *, *, #18831, .T. ) ;
#7194 = CARTESIAN_POINT ( 'NONE',  ( 10.00000000000000711, 206.9523078486586201, -0.9988620819214343305 ) ) ;
#7195 = CARTESIAN_POINT ( 'NONE',  ( -3.044812012440131443, 216.5253028482142952, 61.10113791807857098 ) ) ;
#7196 = ORIENTED_EDGE ( 'NONE', *, *, #17216, .T. ) ;
#7197 = CARTESIAN_POINT ( 'NONE',  ( -7.984503880673422316, 204.3529502787951628, 20.34886208192143542 ) ) ;
#7198 = CARTESIAN_POINT ( 'NONE',  ( 109.0104235265664272, 155.0000000000000000, 11.99999999999998224 ) ) ;
#7199 = ORIENTED_EDGE ( 'NONE', *, *, #26031, .F. ) ;
#7200 = CIRCLE ( 'NONE', #20254, 2.149999999999999023 ) ;
#7201 = CARTESIAN_POINT ( 'NONE',  ( -4.903702542908602524, 213.8346818373418898, 3.951137918078566624 ) ) ;
#7202 = CARTESIAN_POINT ( 'NONE',  ( -7.500000000000001776, 0.000000000000000000, 0.000000000000000000 ) ) ;
#7203 = CARTESIAN_POINT ( 'NONE',  ( 0.05014649552828288198, 194.3824533091408000, 91.74886208192144466 ) ) ;
#7204 = CARTESIAN_POINT ( 'NONE',  ( 38.57499999726881157, 145.8408176439707802, 12.60653300113718345 ) ) ;
#7205 = ORIENTED_EDGE ( 'NONE', *, *, #9276, .F. ) ;
#7206 = CARTESIAN_POINT ( 'NONE',  ( 43.42499999726881299, 168.2552932293087906, -9.630534252274385310 ) ) ;
#7207 = CARTESIAN_POINT ( 'NONE',  ( 39.68867513459483121, 159.8737954434936057, 15.00000000000001421 ) ) ;
#7208 = CARTESIAN_POINT ( 'NONE',  ( 9.984503880673470277, 203.7031108863295401, 2.151137918078565914 ) ) ;
#7209 = CARTESIAN_POINT ( 'NONE',  ( -6.139770520408224463, 198.4640165459539389, 74.04886208192142760 ) ) ;
#7210 = CARTESIAN_POINT ( 'NONE',  ( 48.67499999726881299, 141.7447067706911810, 9.630534252274376428 ) ) ;
#7211 = DIRECTION ( 'NONE',  ( -1.000000000000000000, -0.000000000000000000, -0.000000000000000000 ) ) ;
#7212 = CARTESIAN_POINT ( 'NONE',  ( -8.062137200540920645, 212.9164362838581894, 0.8011379180785658249 ) ) ;
#7213 = CARTESIAN_POINT ( 'NONE',  ( 6.500000000000000000, 2.227636940139130051, -0.2900584647821234374 ) ) ;
#7214 = PRODUCT_DEFINITION_FORMATION_WITH_SPECIFIED_SOURCE ( 'ANY', '', #3690, .NOT_KNOWN. ) ;
#7215 = CARTESIAN_POINT ( 'NONE',  ( 58.39999999999999858, 150.2886644046228639, -14.50000000000000888 ) ) ;
#7216 = CARTESIAN_POINT ( 'NONE',  ( -6.139770520408369237, 215.5359834540460042, 93.95113791807854398 ) ) ;
#7217 = CARTESIAN_POINT ( 'NONE',  ( 125.5000000000000000, 48.99999999999998579, 2.149999999999971489 ) ) ;
#7218 = CARTESIAN_POINT ( 'NONE',  ( 0.05014649552810505201, 217.5146222423826714, 79.25113791807856956 ) ) ;
#7219 = DIRECTION ( 'NONE',  ( -0.8191520442889907994, 0.000000000000000000, -0.5735764363510474917 ) ) ;
#7220 = CARTESIAN_POINT ( 'NONE',  ( 34.77499999726880731, 140.1801316387863778, 4.815267126137185549 ) ) ;
#7221 = CARTESIAN_POINT ( 'NONE',  ( 9.680171189290716072, 214.0920067884432854, 87.69886208192144750 ) ) ;
#7222 = CARTESIAN_POINT ( 'NONE',  ( 64.02499999726880731, 160.0630714827496206, 15.58253174999999402 ) ) ;
#7224 = ORIENTED_EDGE ( 'NONE', *, *, #16463, .F. ) ;
#7223 = CARTESIAN_POINT ( 'NONE',  ( -6.139770520408368348, 215.5359834540460042, 33.95113791807856529 ) ) ;
#7225 = DIRECTION ( 'NONE',  ( 1.000000000000000000, 0.000000000000000000, 0.000000000000000000 ) ) ;
#7226 = AXIS2_PLACEMENT_3D ( 'NONE', #2490, #17990, #5204 ) ;
#7227 = CARTESIAN_POINT ( 'NONE',  ( 86.27499999726880731, 160.0630714827496206, 15.58253174999999402 ) ) ;
#7228 = CARTESIAN_POINT ( 'NONE',  ( 9.680171189290831535, 199.9079932115568852, 92.30113791807858092 ) ) ;
#7229 = AXIS2_PLACEMENT_3D ( 'NONE', #25456, #12514, #27834 ) ;
#7230 = CARTESIAN_POINT ( 'NONE',  ( 125.5000000000000000, 80.04668119422662187, 74.95331880577468553 ) ) ;
#7231 = ADVANCED_FACE ( 'NONE', ( #16418 ), #14040, .T. ) ;
#7232 = EDGE_LOOP ( 'NONE', ( #27845, #29053, #26774, #6979 ) ) ;
#7233 = CARTESIAN_POINT ( 'NONE',  ( -0.05014649552828402690, 217.5146222423826714, 90.24886208192143044 ) ) ;
#7234 = CARTESIAN_POINT ( 'NONE',  ( 0.05014649552828288198, 194.3824533091408000, 13.74886208192143577 ) ) ;
#7235 = LINE ( 'NONE', #32951, #31160 ) ;
#7236 = CARTESIAN_POINT ( 'NONE',  ( -0.05014649552810635652, 196.4853777576173002, 32.75113791807856956 ) ) ;
#7237 = CARTESIAN_POINT ( 'NONE',  ( -0.5974722283283655511, 8.315303285985683246, -0.7026937717022859742 ) ) ;
#7238 = CARTESIAN_POINT ( 'NONE',  ( -8.062137200540822946, 201.0835637161416400, 98.19886208192143329 ) ) ;
#7239 = EDGE_CURVE ( 'NONE', #30802, #12687, #26815, .T. ) ;
#7240 = AXIS2_PLACEMENT_3D ( 'NONE', #28131, #15184, #25577 ) ;
#7241 = FACE_OUTER_BOUND ( 'NONE', #24373, .T. ) ;
#7242 = ORIENTED_EDGE ( 'NONE', *, *, #12909, .T. ) ;
#7243 = CARTESIAN_POINT ( 'NONE',  ( -9.981832587775443244, 205.9534224131111273, 104.4516590477787901 ) ) ;
#7244 = CARTESIAN_POINT ( 'NONE',  ( 4.984841277089891776, 200.2242689037093726, 79.44886208192144750 ) ) ;
#7245 = ORIENTED_EDGE ( 'NONE', *, *, #19318, .T. ) ;
#7246 = APPLICATION_CONTEXT ( 'automotive_design' ) ;
#7247 = DIRECTION ( 'NONE',  ( 0.000000000000000000, 0.000000000000000000, -1.000000000000000000 ) ) ;
#7248 = ORIENTED_EDGE ( 'NONE', *, *, #14578, .T. ) ;
#7249 = DIRECTION ( 'NONE',  ( -0.000000000000000000, -0.000000000000000000, 1.000000000000000000 ) ) ;
#7250 = AXIS2_PLACEMENT_3D ( 'NONE', #31556, #226, #23882 ) ;
#7251 = AXIS2_PLACEMENT_3D ( 'NONE', #30025, #19462, #14511 ) ;
#7252 = CARTESIAN_POINT ( 'NONE',  ( 73.77499999726882152, 169.8198683612136222, -4.815267126137197984 ) ) ;
#7253 = CARTESIAN_POINT ( 'NONE',  ( 83.12499999726881583, 155.0000000000000000, -15.58253175000000823 ) ) ;
#7254 = ADVANCED_FACE ( 'NONE', ( #29711 ), #492, .T. ) ;
#7255 = CARTESIAN_POINT ( 'NONE',  ( -150.0000000000000000, 0.000000000000000000, 20.00000000000000000 ) ) ;
#7256 = CARTESIAN_POINT ( 'NONE',  ( -0.05014649552807731031, 198.5883022060938572, 74.75113791807856956 ) ) ;
#7257 = CARTESIAN_POINT ( 'NONE',  ( 0.000000000000000000, 0.000000000000000000, 0.000000000000000000 ) ) ;
#7258 = CIRCLE ( 'NONE', #20849, 2.000000000000000888 ) ;
#7259 = CARTESIAN_POINT ( 'NONE',  ( 45.00000000000000000, 170.2462022514548323, -7.872454543227099337E-15 ) ) ;
#7260 = CARTESIAN_POINT ( 'NONE',  ( 4.984841277089891776, 200.2242689037093726, 58.44886208192144039 ) ) ;
#7261 = EDGE_CURVE ( 'NONE', #13192, #9072, #2693, .T. ) ;
#7262 = VECTOR ( 'NONE', #15307, 1000.000000000000000 ) ;
#7263 = CARTESIAN_POINT ( 'NONE',  ( -6.500000000000000000, -0.6456425506958733962, 7.521652571618187011E-16 ) ) ;
#7264 = CARTESIAN_POINT ( 'NONE',  ( -0.6250000000000001110, 8.299410119600874935, -7.298562697733108173 ) ) ;
#7265 = CARTESIAN_POINT ( 'NONE',  ( -127.6439996469472788, 4.587378538859859134, 35.00001200000001234 ) ) ;
#7266 = CARTESIAN_POINT ( 'NONE',  ( 59.72499999726881015, 169.8198683612136222, 4.815267126137181997 ) ) ;
#7267 = CARTESIAN_POINT ( 'NONE',  ( 61.67499999726881299, 168.2552932293087906, -9.630534252274385310 ) ) ;
#7268 = STYLED_ITEM ( 'NONE', ( #1302 ), #20158 ) ;
#7269 = CARTESIAN_POINT ( 'NONE',  ( -7.456977232089304408, 196.8216656703010301, 60.05113791807858092 ) ) ;
#7270 = DIRECTION ( 'NONE',  ( 0.000000000000000000, 0.000000000000000000, -1.000000000000000000 ) ) ;
#7271 = CARTESIAN_POINT ( 'NONE',  ( -3.662846001190052991, 218.4274158808045740, 4.101137918078565647 ) ) ;
#7272 = CARTESIAN_POINT ( 'NONE',  ( 8.118202686958039038, 212.8392687619912635, 76.70113791807857240 ) ) ;
#7273 = CARTESIAN_POINT ( 'NONE',  ( 11.98450388067341876, 210.9467285061363953, 45.84886208192143187 ) ) ;
#7274 = CARTESIAN_POINT ( 'NONE',  ( 10.01549611932659367, 203.7984951890124421, 58.14886208192142902 ) ) ;
#7275 = CARTESIAN_POINT ( 'NONE',  ( 0.000000000000000000, 0.000000000000000000, -18.00000000000000000 ) ) ;
#7276 = CIRCLE ( 'NONE', #8915, 24.99999999999999289 ) ;
#7277 =( BOUNDED_CURVE ( )  B_SPLINE_CURVE ( 2, ( #1633, #1468, #27358, #17647, #14581, #9470, #20199, #14744, #25137, #22413, #32803 ),
 .UNSPECIFIED., .F., .T. ) 
 B_SPLINE_CURVE_WITH_KNOTS ( ( 3, 2, 2, 2, 2, 3 ),
 ( 0.1607142857142858372, 0.1642857142857143127, 0.1678571428571427882, 0.1714285714285712636, 0.1749999999999997391, 0.1785714285714282146 ),
 .UNSPECIFIED. ) 
 CURVE ( )  GEOMETRIC_REPRESENTATION_ITEM ( )  RATIONAL_B_SPLINE_CURVE ( ( 0.9999999999999981126, 0.9510565162951553075, 1.000000000000000000, 0.9510565162951534202, 1.000000000000000000, 0.9510565162951534202, 1.000000000000000000, 0.9510565162951534202, 1.000000000000000000, 0.9510565162951571949, 0.9999999999999962252 ) ) 
 REPRESENTATION_ITEM ( '' )  );
#7278 = CARTESIAN_POINT ( 'NONE',  ( -9.736236675707914401, 199.9851607334237542, 84.20113791807858661 ) ) ;
#7279 = CARTESIAN_POINT ( 'NONE',  ( -125.0000000000000000, 25.00000000000000000, -20.00000000000000000 ) ) ;
#7280 = CARTESIAN_POINT ( 'NONE',  ( 10.00000000000000711, 206.9523078486586201, 8.001137918078566003 ) ) ;
#7281 = AXIS2_PLACEMENT_3D ( 'NONE', #20311, #10441, #13474 ) ;
#7282 = CARTESIAN_POINT ( 'NONE',  ( -9.984503880673420539, 203.7031108863293980, 65.34886208192143897 ) ) ;
#7283 = VECTOR ( 'NONE', #23533, 1000.000000000000000 ) ;
#7284 = DIRECTION ( 'NONE',  ( 1.000000000000000000, -0.000000000000000000, -0.000000000000000000 ) ) ;
#7285 = ORIENTED_EDGE ( 'NONE', *, *, #15353, .F. ) ;
#7286 = CARTESIAN_POINT ( 'NONE',  ( 12.01549611932659367, 203.1486557965466773, 76.14886208192143613 ) ) ;
#7287 = ORIENTED_EDGE ( 'NONE', *, *, #13269, .F. ) ;
#7288 = CARTESIAN_POINT ( 'NONE',  ( 75.27499999726879309, 149.9369285172503510, -15.58253175000000823 ) ) ;
#7289 = CARTESIAN_POINT ( 'NONE',  ( 8.015496119326595448, 204.4483345814782638, 55.14886208192145034 ) ) ;
#7290 = ORIENTED_EDGE ( 'NONE', *, *, #1384, .F. ) ;
#7291 = EDGE_CURVE ( 'NONE', #15658, #25924, #8654, .T. ) ;
#7292 = EDGE_CURVE ( 'NONE', #6439, #5220, #8932, .T. ) ;
#7293 = CARTESIAN_POINT ( 'NONE',  ( 68.22499999726881015, 149.9369285172503510, 15.58253174999999580 ) ) ;
#7294 = CARTESIAN_POINT ( 'NONE',  ( -67.50000000000000000, -92.00000000000000000, 17.00000000000001421 ) ) ;
#7295 = CIRCLE ( 'NONE', #25799, 18.00000000000000000 ) ;
#7296 = FACE_OUTER_BOUND ( 'NONE', #22052, .T. ) ;
#7297 = CARTESIAN_POINT ( 'NONE',  ( 65.02499999726882152, 149.9369285172503510, -15.58253175000000823 ) ) ;
#7298 = EDGE_CURVE ( 'NONE', #11884, #32735, #30355, .T. ) ;
#7299 = CARTESIAN_POINT ( 'NONE',  ( -7.922811899608408481, -4.628803996615321381, -8.057669882367649805 ) ) ;
#7300 = CARTESIAN_POINT ( 'NONE',  ( -8.118202686958138514, 212.8392687619910930, 44.79886208192143471 ) ) ;
#7301 = EDGE_LOOP ( 'NONE', ( #1500, #9879 ) ) ;
#7302 = CARTESIAN_POINT ( 'NONE',  ( 115.4999999999999858, 52.61186241335891367, 27.43481878086798176 ) ) ;
#7303 = VECTOR ( 'NONE', #24688, 1000.000000000000114 ) ;
#7304 = CARTESIAN_POINT ( 'NONE',  ( 127.5000000000000000, 155.0000000000000000, -6.938893903907228378E-15 ) ) ;
#7305 = PLANE ( 'NONE',  #32149 ) ;
#7306 = CARTESIAN_POINT ( 'NONE',  ( -6.500168698208244500, 211.6636982574061676, 29.79886208192143826 ) ) ;
#7307 = CONICAL_SURFACE ( 'NONE', #9459, 4.171999999999999709, 0.7853981633974687071 ) ;
#7308 = EDGE_CURVE ( 'NONE', #4045, #3502, #1100, .T. ) ;
#7309 = CARTESIAN_POINT ( 'NONE',  ( 10.01549611932653860, 210.2015048109876716, 70.85113791807854966 ) ) ;
#7310 = CARTESIAN_POINT ( 'NONE',  ( 8.331345277524542681, 0.000000000000000000, -7.381345277524544279 ) ) ;
#7311 = CARTESIAN_POINT ( 'NONE',  ( -10.00000000000000711, 207.0476921513413515, 45.50113791807857666 ) ) ;
#7312 = CARTESIAN_POINT ( 'NONE',  ( 9.984503880673470277, 203.7031108863295401, 20.15113791807856813 ) ) ;
#7313 = CARTESIAN_POINT ( 'NONE',  ( 8.015496119326531499, 209.5516654185219636, 4.851137918078565647 ) ) ;
#7314 = DIRECTION ( 'NONE',  ( 1.000000000000000000, 0.000000000000000000, 0.000000000000000000 ) ) ;
#7315 = CARTESIAN_POINT ( 'NONE',  ( 40.62499999726880873, 138.6155565068815747, -3.929120461958505118E-15 ) ) ;
#7316 = CARTESIAN_POINT ( 'NONE',  ( -3.753561863808691168, 195.6020594897209435, 26.90113791807856813 ) ) ;
#7317 = FACE_BOUND ( 'NONE', #15067, .T. ) ;
#7318 = CARTESIAN_POINT ( 'NONE',  ( -3.044812012440131443, 216.5253028482142952, 73.10113791807857808 ) ) ;
#7319 = CARTESIAN_POINT ( 'NONE',  ( -6.220909254589537696, 198.5229672870051445, 54.05113791807855961 ) ) ;
#7320 = CARTESIAN_POINT ( 'NONE',  ( 92.50248874961125978, 155.0000000000000000, 0.000000000000000000 ) ) ;
#7321 =( GEOMETRIC_REPRESENTATION_CONTEXT ( 3 ) GLOBAL_UNCERTAINTY_ASSIGNED_CONTEXT ( ( #15858 ) ) GLOBAL_UNIT_ASSIGNED_CONTEXT ( ( #32334, #9332, #29956 ) ) REPRESENTATION_CONTEXT ( 'NONE', 'WORKASPACE' ) );
#7322 = CARTESIAN_POINT ( 'NONE',  ( 35.18867513459482410, 169.2658477444273331, -4.635254915624224203 ) ) ;
#7323 = CARTESIAN_POINT ( 'NONE',  ( -7.375838497908014268, 196.7627149292498530, 17.04886208192143471 ) ) ;
#7324 = CARTESIAN_POINT ( 'NONE',  ( -10.01549611932659545, 210.2015048109875011, 17.64886208192143613 ) ) ;
#7325 = CARTESIAN_POINT ( 'NONE',  ( 70.89999999453762314, 159.7113355953771077, 14.49999999999999289 ) ) ;
#7326 = VERTEX_POINT ( 'NONE', #29045 ) ;
#7327 = CARTESIAN_POINT ( 'NONE',  ( 0.05014649552807549926, 219.6175466908591716, 55.25113791807857666 ) ) ;
#7328 = CARTESIAN_POINT ( 'NONE',  ( 6.444103211791042618, 202.2591342207267644, 77.30113791807858092 ) ) ;
#7329 = CARTESIAN_POINT ( 'NONE',  ( 0.05014649552828275708, 196.4853777576173002, 37.74886208192143755 ) ) ;
#7330 = DIRECTION ( 'NONE',  ( -0.000000000000000000, -0.000000000000000000, -1.000000000000000000 ) ) ;
#7331 = ORIENTED_EDGE ( 'NONE', *, *, #29781, .T. ) ;
#7332 = CIRCLE ( 'NONE', #33441, 40.00000000000000711 ) ;
#7333 = VERTEX_POINT ( 'NONE', #18655 ) ;
#7334 = VERTEX_POINT ( 'NONE', #5699 ) ;
#7335 = ADVANCED_FACE ( 'NONE', ( #14386 ), #4494, .T. ) ;
#7336 = CYLINDRICAL_SURFACE ( 'NONE', #28221, 15.00000000000001776 ) ;
#7337 = DIRECTION ( 'NONE',  ( -0.000000000000000000, -0.000000000000000000, -1.000000000000000000 ) ) ;
#7338 = ORIENTED_EDGE ( 'NONE', *, *, #3709, .T. ) ;
#7339 = CARTESIAN_POINT ( 'NONE',  ( -4.903702542908602524, 213.8346818373418898, 30.95113791807857595 ) ) ;
#7340 = DIRECTION ( 'NONE',  ( -1.000000000000000000, -0.000000000000000000, -0.000000000000000000 ) ) ;
#7341 = CARTESIAN_POINT ( 'NONE',  ( -3.044812012439970683, 197.4746971517856196, 16.89886208192143613 ) ) ;
#7342 = CARTESIAN_POINT ( 'NONE',  ( 55.97499999726881015, 169.8198683612136222, 4.815267126137181997 ) ) ;
#7343 = VERTEX_POINT ( 'NONE', #27323 ) ;
#7344 = CARTESIAN_POINT ( 'NONE',  ( -2.426778023690262742, 214.6231898156240163, 55.10113791807857808 ) ) ;
#7345 = CARTESIAN_POINT ( 'NONE',  ( 0.000000000000000000, 1.759474945355380404, -3.047500000000001652 ) ) ;
#7346 = CARTESIAN_POINT ( 'NONE',  ( -63.49999999999884892, 215.0000000000000000, 2.500000000000000000 ) ) ;
#7347 = CARTESIAN_POINT ( 'NONE',  ( -6.220909254589682469, 215.4770327129946850, 98.94886208192140487 ) ) ;
#7348 = CARTESIAN_POINT ( 'NONE',  ( 65.37499999726881583, 155.0000000000000000, -15.58253175000000823 ) ) ;
#7349 = CARTESIAN_POINT ( 'NONE',  ( 6.220909254589536808, 215.4770327129947702, 37.55113791807856671 ) ) ;
#7350 = CARTESIAN_POINT ( 'NONE',  ( 70.68867513459485963, 150.1262045565065648, -15.00000000000016520 ) ) ;
#7351 = CARTESIAN_POINT ( 'NONE',  ( 9.984503880673470277, 203.7031108863295401, 20.15113791807856813 ) ) ;
#7352 = CARTESIAN_POINT ( 'NONE',  ( 8.062137200540822946, 212.9164362838583315, 99.69886208192144750 ) ) ;
#7353 = DIRECTION ( 'NONE',  ( 0.000000000000000000, 0.000000000000000000, 1.000000000000000000 ) ) ;
#7354 = CARTESIAN_POINT ( 'NONE',  ( 85.79999999999999716, 142.6655632788954620, 8.961492836873471646 ) ) ;
#7355 = CARTESIAN_POINT ( 'NONE',  ( -4.515071337844649868, -29.14748715311448279, -1.088725517910814400 ) ) ;
#7356 = DIRECTION ( 'NONE',  ( -0.000000000000000000, -0.000000000000000000, 1.000000000000000000 ) ) ;
#7357 = CARTESIAN_POINT ( 'NONE',  ( -3.044812012440131443, 216.5253028482142952, 100.1011379180785781 ) ) ;
#7358 = CARTESIAN_POINT ( 'NONE',  ( 60.00000000000000000, 7.347880794884118356E-15, 35.00000000000000000 ) ) ;
#7359 = CARTESIAN_POINT ( 'NONE',  ( 49.47499999726881725, 160.0630714827496206, -15.58253175000000823 ) ) ;
#7360 = CARTESIAN_POINT ( 'NONE',  ( -10.00000000000000711, 207.0476921513413515, 45.50113791807857666 ) ) ;
#7361 = CARTESIAN_POINT ( 'NONE',  ( 35.01132485994281041, 142.2402378747194405, 9.270509831248432420 ) ) ;
#7362 = DIRECTION ( 'NONE',  ( 0.000000000000000000, 0.000000000000000000, -1.000000000000000000 ) ) ;
#7363 = DIRECTION ( 'NONE',  ( -1.000000000000000000, 0.000000000000000000, 0.000000000000000000 ) ) ;
#7364 = CARTESIAN_POINT ( 'NONE',  ( 54.39999999453763024, 168.7903194862797420, -4.480746418436745593 ) ) ;
#7365 = ORIENTED_EDGE ( 'NONE', *, *, #31069, .T. ) ;
#7366 = CARTESIAN_POINT ( 'NONE',  ( 7.375838497908181246, 196.7627149292499666, 29.45113791807856529 ) ) ;
#7367 = FACE_OUTER_BOUND ( 'NONE', #31700, .T. ) ;
#7368 = CARTESIAN_POINT ( 'NONE',  ( -8.118202686958138514, 212.8392687619910930, 14.79886208192143648 ) ) ;
#7369 = DIRECTION ( 'NONE',  ( 0.000000000000000000, 0.000000000000000000, 1.000000000000000000 ) ) ;
#7370 = ORIENTED_EDGE ( 'NONE', *, *, #20639, .T. ) ;
#7371 = CARTESIAN_POINT ( 'NONE',  ( -10.00000000000000711, 207.0476921513413515, 9.501137918078566003 ) ) ;
#7372 = CARTESIAN_POINT ( 'NONE',  ( -8.118202686958039038, 201.1607312380087080, 57.20113791807857950 ) ) ;
#7373 = VERTEX_POINT ( 'NONE', #33117 ) ;
#7374 = CARTESIAN_POINT ( 'NONE',  ( -2.426778023690076225, 199.3768101843759553, 22.89886208192143613 ) ) ;
#7375 = DIRECTION ( 'NONE',  ( 0.000000000000000000, 0.000000000000000000, 1.000000000000000000 ) ) ;
#7376 = ORIENTED_EDGE ( 'NONE', *, *, #24018, .F. ) ;
#7377 = CARTESIAN_POINT ( 'NONE',  ( 0.05014649552807626948, 215.4116977939061144, 1.251137918078566225 ) ) ;
#7378 = CARTESIAN_POINT ( 'NONE',  ( 12.01549611932659367, 203.1486557965466773, 91.14886208192143613 ) ) ;
#7379 = CARTESIAN_POINT ( 'NONE',  ( 38.97499999726881015, 140.1801316387863778, -4.815267126137194431 ) ) ;
#7380 = ORIENTED_EDGE ( 'NONE', *, *, #29747, .T. ) ;
#7381 = CARTESIAN_POINT ( 'NONE',  ( 42.82499999726879736, 141.7447067706911810, -9.630534252274385310 ) ) ;
#7382 = CARTESIAN_POINT ( 'NONE',  ( 119.8866434474913660, 1.374176392886252707, 35.00001199999999812 ) ) ;
#7383 = CARTESIAN_POINT ( 'NONE',  ( -6.220909254589537696, 198.5229672870051161, 3.051137918078564937 ) ) ;
#7384 = CARTESIAN_POINT ( 'NONE',  ( -10.00000000000000711, 206.9523078486584495, 68.49886208192143044 ) ) ;
#7385 = CARTESIAN_POINT ( 'NONE',  ( 49.27499999726880020, 149.9369285172503510, -15.58253175000000823 ) ) ;
#7386 = CARTESIAN_POINT ( 'NONE',  ( 8.118202686958039038, 212.8392687619912635, 13.70113791807856707 ) ) ;
#7387 = CARTESIAN_POINT ( 'NONE',  ( -27.50000000000000000, -15.87713240271474824, -2.456200930618646971 ) ) ;
#7388 = EDGE_CURVE ( 'NONE', #28270, #14862, #30398, .T. ) ;
#7389 = CARTESIAN_POINT ( 'NONE',  ( 69.20000000000001705, 167.3344367211045096, 8.961492836873468093 ) ) ;
#7390 = CARTESIAN_POINT ( 'NONE',  ( -0.05014649552810635652, 196.4853777576173002, 92.75113791807858377 ) ) ;
#7391 = DIRECTION ( 'NONE',  ( 0.000000000000000000, -0.8660254037844391517, -0.4999999999999991118 ) ) ;
#7392 = CARTESIAN_POINT ( 'NONE',  ( 10.00000000000000711, 206.9523078486586201, 74.00113791807858377 ) ) ;
#7393 = CARTESIAN_POINT ( 'NONE',  ( -1.015826369459165157, 8.073766409993364590, -7.642786413619490737 ) ) ;
#7394 = CARTESIAN_POINT ( 'NONE',  ( 87.50000000000001421, 155.0000000000000000, -6.938893903907228378E-15 ) ) ;
#7395 = CARTESIAN_POINT ( 'NONE',  ( 3.753561863808876797, 195.6020594897209719, 91.59886208192145318 ) ) ;
#7396 = CARTESIAN_POINT ( 'NONE',  ( 66.02499999726879309, 160.0630714827496206, 15.58253174999999402 ) ) ;
#7398 = ORIENTED_EDGE ( 'NONE', *, *, #23828, .F. ) ;
#7397 = CARTESIAN_POINT ( 'NONE',  ( 3.044812012440130555, 197.4746971517856764, 26.60113791807856742 ) ) ;
#7399 = CARTESIAN_POINT ( 'NONE',  ( 43.31132485994280756, 140.7341522555726669, -4.635254915624220651 ) ) ;
#7400 = CARTESIAN_POINT ( 'NONE',  ( 35.19999999453762740, 146.4771138417591203, 11.73074641843673227 ) ) ;
#7401 = CARTESIAN_POINT ( 'NONE',  ( -3.662846001190052991, 218.4274158808045740, 97.10113791807857808 ) ) ;
#7402 = DIRECTION ( 'NONE',  ( 1.000000000000000000, 0.000000000000000000, 0.000000000000000000 ) ) ;
#7403 = ORIENTED_EDGE ( 'NONE', *, *, #19488, .F. ) ;
#7404 = CARTESIAN_POINT ( 'NONE',  ( 10.00000000000000711, 207.0476921513415220, 84.99886208192143044 ) ) ;
#7405 = CARTESIAN_POINT ( 'NONE',  ( -3.753561863808878130, 218.3979405102790281, 21.09886208192143897 ) ) ;
#7406 = LINE ( 'NONE', #12847, #17581 ) ;
#7407 = CARTESIAN_POINT ( 'NONE',  ( 6.220909254589536808, 215.4770327129947702, 28.55113791807855961 ) ) ;
#7408 = DIRECTION ( 'NONE',  ( 0.000000000000000000, 0.000000000000000000, 1.000000000000000000 ) ) ;
#7409 = CARTESIAN_POINT ( 'NONE',  ( -10.00000000000000711, 206.9523078486584495, 101.4988620819214304 ) ) ;
#7410 = CARTESIAN_POINT ( 'NONE',  ( 2.000000000000000000, 1.880445160090761061E-16, -1.535500000000000087 ) ) ;
#7411 = ORIENTED_EDGE ( 'NONE', *, *, #1384, .T. ) ;
#7412 = CARTESIAN_POINT ( 'NONE',  ( 125.5000000000000000, 155.0000000000000000, 112.0000000000000426 ) ) ;
#7413 = CARTESIAN_POINT ( 'NONE',  ( -2.517493886309087880, 214.5937144450984135, 84.09886208192143897 ) ) ;
#7414 = ADVANCED_FACE ( 'NONE', ( #7059 ), #30430, .T. ) ;
#7415 = ORIENTED_EDGE ( 'NONE', *, *, #29527, .T. ) ;
#7416 = ORIENTED_EDGE ( 'NONE', *, *, #29362, .T. ) ;
#7417 = CARTESIAN_POINT ( 'NONE',  ( 0.000000000000000000, -0.8865213383406685965, 1.535500000000000531 ) ) ;
#7418 = CARTESIAN_POINT ( 'NONE',  ( 2.517493886308900919, 214.5937144450984420, 64.40113791807856103 ) ) ;
#7419 = CARTESIAN_POINT ( 'NONE',  ( 81.02499999726880731, 149.9369285172503510, -15.58253175000000823 ) ) ;
#7420 = CARTESIAN_POINT ( 'NONE',  ( 107.0104235265664556, 155.0000000000000000, 11.99999999999998224 ) ) ;
#7421 =( BOUNDED_CURVE ( )  B_SPLINE_CURVE ( 2, ( #21269, #27051, #656, #26710, #15993, #26541, #13933, #18724, #26385, #3045, #825 ),
 .UNSPECIFIED., .F., .T. ) 
 B_SPLINE_CURVE_WITH_KNOTS ( ( 3, 2, 2, 2, 2, 3 ),
 ( 0.4999999999999998890, 0.5035714285714285587, 0.5071428571428571175, 0.5107142857142856762, 0.5142857142857142350, 0.5178571428571427937 ),
 .UNSPECIFIED. ) 
 CURVE ( )  GEOMETRIC_REPRESENTATION_ITEM ( )  RATIONAL_B_SPLINE_CURVE ( ( 1.000000000000000666, 0.9510565162951526430, 1.000000000000000000, 0.9510565162951534202, 1.000000000000000000, 0.9510565162951534202, 1.000000000000000000, 0.9510565162951534202, 1.000000000000000000, 0.9510565162951534202, 1.000000000000000000 ) ) 
 REPRESENTATION_ITEM ( '' )  );
#7422 = CARTESIAN_POINT ( 'NONE',  ( -8.015496119326531499, 204.4483345814780364, 75.35113791807856387 ) ) ;
#7423 = DIRECTION ( 'NONE',  ( 1.000000000000000000, -0.000000000000000000, -0.000000000000000000 ) ) ;
#7424 = EDGE_CURVE ( 'NONE', #7326, #11207, #5921, .T. ) ;
#7425 = CARTESIAN_POINT ( 'NONE',  ( 48.40000000000000568, 150.2886644046228639, -14.50000000000000888 ) ) ;
#7426 = CARTESIAN_POINT ( 'NONE',  ( -2.517493886309087880, 214.5937144450984135, 66.09886208192142476 ) ) ;
#7427 = ADVANCED_FACE ( 'NONE', ( #9782 ), #32429, .F. ) ;
#7428 = AXIS2_PLACEMENT_3D ( 'NONE', #17236, #22015, #9063 ) ;
#7429 = EDGE_CURVE ( 'NONE', #17208, #10473, #32767, .T. ) ;
#7430 = CIRCLE ( 'NONE', #3071, 3.047499999999999876 ) ;
#7431 = CARTESIAN_POINT ( 'NONE',  ( -8.118202686958039038, 201.1607312380087080, 0.2011379180785657361 ) ) ;
#7432 = CARTESIAN_POINT ( 'NONE',  ( 124.9999999999999716, -73.00000000000002842, -20.00000000000000000 ) ) ;
#7433 = DIRECTION ( 'NONE',  ( 1.000000000000000000, -0.000000000000000000, -0.000000000000000000 ) ) ;
#7434 = CARTESIAN_POINT ( 'NONE',  ( 57.02499999726882152, 149.9369285172503510, -15.58253175000000823 ) ) ;
#7435 = CARTESIAN_POINT ( 'NONE',  ( 72.57499999726880446, 145.8408176439707802, 12.60653300113718345 ) ) ;
#7436 = CARTESIAN_POINT ( 'NONE',  ( -0.05014649552807705357, 194.3824533091408000, 71.75113791807856956 ) ) ;
#7437 = CARTESIAN_POINT ( 'NONE',  ( 2.428571428571428381, 0.000000000000000000, 2.066666666667000385 ) ) ;
#7438 = CARTESIAN_POINT ( 'NONE',  ( -11.98450388067348804, 210.9467285061362247, 9.651137918078566358 ) ) ;
#7439 = CARTESIAN_POINT ( 'NONE',  ( 8.062137200540920645, 201.0835637161417822, 92.30113791807858092 ) ) ;
#7440 = CARTESIAN_POINT ( 'NONE',  ( 12.01549611932659367, 203.1486557965466773, 43.14886208192143613 ) ) ;
#7441 = CARTESIAN_POINT ( 'NONE',  ( 6.139770520408223575, 215.5359834540460611, 57.54886208192142760 ) ) ;
#7442 = DIRECTION ( 'NONE',  ( -0.000000000000000000, -0.000000000000000000, 1.000000000000000000 ) ) ;
#7443 = CARTESIAN_POINT ( 'NONE',  ( -12.00000000000000711, 207.0476921513413515, 96.50113791807856956 ) ) ;
#7444 = DIRECTION ( 'NONE',  ( 1.000000000000000000, 0.000000000000000000, 0.000000000000000000 ) ) ;
#7445 = CARTESIAN_POINT ( 'NONE',  ( -3.135527875058821579, 197.5041725223112223, -0.09886208192143428053 ) ) ;
#7446 = CARTESIAN_POINT ( 'NONE',  ( 3.135527875058981895, 197.5041725223112792, 67.59886208192143897 ) ) ;
#7447 = CARTESIAN_POINT ( 'NONE',  ( 0.000000000000000000, 0.000000000000000000, -17.97459999999999525 ) ) ;
#7448 = EDGE_LOOP ( 'NONE', ( #18051, #2303, #25121, #207 ) ) ;
#7449 = CARTESIAN_POINT ( 'NONE',  ( 7.456977232089471386, 196.8216656703012006, 67.44886208192143329 ) ) ;
#7450 = CARTESIAN_POINT ( 'NONE',  ( -8.118202686958039038, 201.1607312380087080, 93.20113791807857240 ) ) ;
#7451 = ORIENTED_EDGE ( 'NONE', *, *, #20414, .T. ) ;
#7452 = CARTESIAN_POINT ( 'NONE',  ( 76.07499999726879025, 168.2552932293087906, 9.630534252274372875 ) ) ;
#7453 = CARTESIAN_POINT ( 'NONE',  ( -4.984841277089891776, 213.7757310962905990, 47.94886208192144039 ) ) ;
#7454 = EDGE_CURVE ( 'NONE', #12774, #19514, #19661, .T. ) ;
#7455 = ORIENTED_EDGE ( 'NONE', *, *, #12870, .T. ) ;
#7456 = CONICAL_SURFACE ( 'NONE', #26477, 15.79999999999999538, 0.9599310885968802554 ) ;
#7457 = CARTESIAN_POINT ( 'NONE',  ( 71.82499999726881867, 168.2552932293087906, 9.630534252274372875 ) ) ;
#7458 = CARTESIAN_POINT ( 'NONE',  ( -125.0000000000000000, 0.000000000000000000, -35.00000000000000000 ) ) ;
#7459 = CARTESIAN_POINT ( 'NONE',  ( -56.12712552280034117, 194.9922069576863066, 0.8039670099889266730 ) ) ;
#7460 = CARTESIAN_POINT ( 'NONE',  ( 60.42499999726881299, 141.7447067706911810, 9.630534252274376428 ) ) ;
#7461 = FACE_OUTER_BOUND ( 'NONE', #25505, .T. ) ;
#7462 = EDGE_CURVE ( 'NONE', #6637, #25971, #25279, .T. ) ;
#7463 = CARTESIAN_POINT ( 'NONE',  ( 0.05014649552828275708, 196.4853777576173002, 52.74886208192143044 ) ) ;
#7464 = EDGE_LOOP ( 'NONE', ( #24203, #18021, #17572, #27724 ) ) ;
#7465 = CYLINDRICAL_SURFACE ( 'NONE', #14006, 24.99999999999999289 ) ;
#7466 = SURFACE_STYLE_FILL_AREA ( #30464 ) ;
#7467 = DIRECTION ( 'NONE',  ( 0.000000000000000000, 0.000000000000000000, -1.000000000000000000 ) ) ;
#7468 = DIRECTION ( 'NONE',  ( -0.000000000000000000, -0.000000000000000000, 1.000000000000000000 ) ) ;
#7469 = CARTESIAN_POINT ( 'NONE',  ( 4.903702542908435547, 213.8346818373419751, 24.54886208192144181 ) ) ;
#7470 = CARTESIAN_POINT ( 'NONE',  ( -3.044812012440131443, 216.5253028482142952, 70.10113791807857808 ) ) ;
#7471 = PLANE ( 'NONE',  #25623 ) ;
#7472 = CARTESIAN_POINT ( 'NONE',  ( -8.118202686958039038, 201.1607312380087080, 57.20113791807857950 ) ) ;
#7473 = EDGE_CURVE ( 'NONE', #21688, #22734, #17075, .T. ) ;
#7474 = CARTESIAN_POINT ( 'NONE',  ( -3.044812012440131443, 216.5253028482142952, 25.10113791807856742 ) ) ;
#7475 = CARTESIAN_POINT ( 'NONE',  ( -6.444103211791042618, 211.7408657792732356, 3.801137918078566269 ) ) ;
#7476 = CARTESIAN_POINT ( 'NONE',  ( 123.6258236071138015, -5.113356552508631303, 35.00001199999999812 ) ) ;
#7477 = DIRECTION ( 'NONE',  ( 0.000000000000000000, 0.000000000000000000, 1.000000000000000000 ) ) ;
#7478 = CARTESIAN_POINT ( 'NONE',  ( 39.32499999726881157, 164.1591823560292198, -12.60653300113719766 ) ) ;
#7479 =( BOUNDED_CURVE ( )  B_SPLINE_CURVE ( 2, ( #23353, #31184, #23510, #10578, #5937, #24004, #16497, #3055, #29119, #16329, #26896 ),
 .UNSPECIFIED., .F., .F. ) 
 B_SPLINE_CURVE_WITH_KNOTS ( ( 3, 2, 2, 2, 2, 3 ),
 ( 0.8214285714285715079, 0.8250000000000000666, 0.8285714285714287364, 0.8321428571428572951, 0.8357142857142858539, 0.8392857142857144126 ),
 .UNSPECIFIED. ) 
 CURVE ( )  GEOMETRIC_REPRESENTATION_ITEM ( )  RATIONAL_B_SPLINE_CURVE ( ( 0.9999999999999984457, 0.9510565162951549745, 1.000000000000000000, 0.9510565162951534202, 1.000000000000000000, 0.9510565162951534202, 1.000000000000000000, 0.9510565162951534202, 1.000000000000000000, 0.9510565162951518658, 1.000000000000001554 ) ) 
 REPRESENTATION_ITEM ( '' )  );
#7480 = CARTESIAN_POINT ( 'NONE',  ( -3.753561863808691168, 195.6020594897209435, 38.90113791807856813 ) ) ;
#7481 = DIRECTION ( 'NONE',  ( 1.000000000000000000, 0.000000000000000000, 0.000000000000000000 ) ) ;
#7482 = TOROIDAL_SURFACE ( 'NONE', #26501, 70.00000000000001421, 30.00000000000000000 ) ;
#7483 = CARTESIAN_POINT ( 'NONE',  ( 3.044812012440130555, 197.4746971517856764, 80.60113791807857808 ) ) ;
#7484 = CARTESIAN_POINT ( 'NONE',  ( -10.01549611932653860, 203.7984951890123000, 45.35113791807857808 ) ) ;
#7485 = CIRCLE ( 'NONE', #6397, 4.057500000000000107 ) ;
#7486 = DIRECTION ( 'NONE',  ( 0.5000000000000046629, -0.8660254037844359321, 0.000000000000000000 ) ) ;
#7487 = AXIS2_PLACEMENT_3D ( 'NONE', #32663, #2007, #29782 ) ;
#7488 = CARTESIAN_POINT ( 'NONE',  ( 3.662846001189864698, 218.4274158808046593, 15.39886208192143613 ) ) ;
#7489 = CARTESIAN_POINT ( 'NONE',  ( -10.00000000000000711, 206.9523078486584495, 29.49886208192143400 ) ) ;
#7490 = CARTESIAN_POINT ( 'NONE',  ( 72.19999999453763451, 163.5228861582408797, -11.73074641843674470 ) ) ;
#7491 = VERTEX_POINT ( 'NONE', #12332 ) ;
#7492 = CARTESIAN_POINT ( 'NONE',  ( 12.01549611932652972, 210.8513442034534933, 55.85113791807856387 ) ) ;
#7493 = CARTESIAN_POINT ( 'NONE',  ( -8.015496119326531499, 204.4483345814780364, 81.35113791807857808 ) ) ;
#7494 = EDGE_CURVE ( 'NONE', #30420, #7638, #15710, .T. ) ;
#7495 = CARTESIAN_POINT ( 'NONE',  ( -3.135527875058982783, 216.4958274776886924, 42.09886208192143897 ) ) ;
#7496 = CARTESIAN_POINT ( 'NONE',  ( -52.50000000000002132, 0.000000000000000000, 270.4495957273638282 ) ) ;
#7497 = AXIS2_PLACEMENT_3D ( 'NONE', #17104, #4830, #12661 ) ;
#7498 = ORIENTED_EDGE ( 'NONE', *, *, #11384, .T. ) ;
#7499 = CARTESIAN_POINT ( 'NONE',  ( 0.05014649552828288198, 194.3824533091408000, 43.74886208192143755 ) ) ;
#7500 = ORIENTED_EDGE ( 'NONE', *, *, #2325, .F. ) ;
#7501 = EDGE_CURVE ( 'NONE', #29388, #30979, #1049, .T. ) ;
#7502 = ORIENTED_EDGE ( 'NONE', *, *, #25531, .F. ) ;
#7503 = CARTESIAN_POINT ( 'NONE',  ( -150.0000000000000000, 0.000000000000000000, -35.00000000000000000 ) ) ;
#7504 = CARTESIAN_POINT ( 'NONE',  ( 7.703397592599076305, 206.6253034553826637, 111.3476260793010084 ) ) ;
#7505 = VERTEX_POINT ( 'NONE', #22729 ) ;
#7506 = CARTESIAN_POINT ( 'NONE',  ( -8.000000000000008882, 207.0476921513413515, 36.50113791807857666 ) ) ;
#7507 = AXIS2_PLACEMENT_3D ( 'NONE', #25724, #4772, #33565 ) ;
#7508 = CIRCLE ( 'NONE', #1508, 50.00000000000000000 ) ;
#7509 = CARTESIAN_POINT ( 'NONE',  ( 6.220909254589681581, 198.5229672870052582, 19.44886208192142618 ) ) ;
#7510 = CARTESIAN_POINT ( 'NONE',  ( 59.57499999726881157, 164.1591823560292198, -12.60653300113719766 ) ) ;
#7511 = ORIENTED_EDGE ( 'NONE', *, *, #16196, .F. ) ;
#7512 = CARTESIAN_POINT ( 'NONE',  ( -6.444103211791042618, 211.7408657792732356, 60.80113791807858092 ) ) ;
#7513 = DIRECTION ( 'NONE',  ( -1.000000000000000000, 0.000000000000000000, 0.000000000000000000 ) ) ;
#7514 = FILL_AREA_STYLE_COLOUR ( '', #23627 ) ;
#7515 = CARTESIAN_POINT ( 'NONE',  ( 4.000000000000000000, -3.518949890710769246, 3.686287386450715076E-15 ) ) ;
#7516 = CARTESIAN_POINT ( 'NONE',  ( 3.044812012439969795, 216.5253028482143520, 102.3988620819214361 ) ) ;
#7517 = CARTESIAN_POINT ( 'NONE',  ( 65.87499999726880162, 171.3844434931184253, -7.942151717890132712E-15 ) ) ;
#7518 = CARTESIAN_POINT ( 'NONE',  ( 0.05014649552810505201, 217.5146222423826714, 40.25113791807856956 ) ) ;
#7519 = CARTESIAN_POINT ( 'NONE',  ( -10.01549611932653860, 203.7984951890123284, 30.35113791807856742 ) ) ;
#7520 = CARTESIAN_POINT ( 'NONE',  ( 32.50000000000000000, 155.0000000000000000, -6.938893903907228378E-15 ) ) ;
#7521 = CIRCLE ( 'NONE', #12960, 2.149999999999985256 ) ;
#7522 = PRODUCT_CONTEXT ( 'NONE', #18785, 'mechanical' ) ;
#7523 = CARTESIAN_POINT ( 'NONE',  ( 4.903702542908435547, 213.8346818373419751, 84.54886208192144181 ) ) ;
#7524 = CARTESIAN_POINT ( 'NONE',  ( 83.80000000000002558, 142.6655632788954620, 8.961492836873471646 ) ) ;
#7525 = DIRECTION ( 'NONE',  ( 1.000000000000000000, 0.000000000000000000, 0.000000000000000000 ) ) ;
#7526 = CARTESIAN_POINT ( 'NONE',  ( 10.00000000000000178, 0.000000000000000000, -5.400000000000002132 ) ) ;
#7527 = CARTESIAN_POINT ( 'NONE',  ( -12.01549611932652972, 203.1486557965464499, 3.351137918078566091 ) ) ;
#7528 = PLANE ( 'NONE',  #8592 ) ;
#7529 = CARTESIAN_POINT ( 'NONE',  ( 48.27499999726880731, 160.0630714827496206, 15.58253174999999402 ) ) ;
#7530 = ADVANCED_FACE ( 'NONE', ( #22378 ), #6882, .T. ) ;
#7531 = CARTESIAN_POINT ( 'NONE',  ( 6.220909254589536808, 215.4770327129947702, 52.55113791807858092 ) ) ;
#7532 = EDGE_CURVE ( 'NONE', #6694, #14046, #24978, .T. ) ;
#7533 = FACE_OUTER_BOUND ( 'NONE', #31859, .T. ) ;
#7534 = CARTESIAN_POINT ( 'NONE',  ( 77.91132485994280898, 163.8167787843871110, -12.13525491562423397 ) ) ;
#7535 = CARTESIAN_POINT ( 'NONE',  ( -3.044812012439970683, 197.4746971517856196, 1.898862081921434353 ) ) ;
#7536 = CARTESIAN_POINT ( 'NONE',  ( 55.19999999453763451, 146.4771138417591203, 11.73074641843673227 ) ) ;
#7537 = ORIENTED_EDGE ( 'NONE', *, *, #13328, .F. ) ;
#7538 = CARTESIAN_POINT ( 'NONE',  ( -3.662846001190052991, 218.4274158808045740, 25.10113791807856742 ) ) ;
#7539 = EDGE_CURVE ( 'NONE', #31727, #24269, #16809, .T. ) ;
#7540 = ADVANCED_FACE ( 'NONE', ( #18123 ), #7738, .F. ) ;
#7541 = DIRECTION ( 'NONE',  ( 1.000000000000000000, 0.000000000000000000, 0.000000000000000000 ) ) ;
#7542 = CARTESIAN_POINT ( 'NONE',  ( -10.00000000000000711, 206.9523078486584495, 14.49886208192143577 ) ) ;
#7543 = AXIS2_PLACEMENT_3D ( 'NONE', #9665, #1156, #1495 ) ;
#7544 = CARTESIAN_POINT ( 'NONE',  ( 5.000000000000000000, 0.000000000000000000, 0.000000000000000000 ) ) ;
#7545 = EDGE_LOOP ( 'NONE', ( #22267, #16346 ) ) ;
#7546 = CARTESIAN_POINT ( 'NONE',  ( 10.00000000000000711, 206.9523078486586201, 11.00113791807856600 ) ) ;
#7547 = CARTESIAN_POINT ( 'NONE',  ( -6.139770520408369237, 215.5359834540460042, 69.95113791807857240 ) ) ;
#7548 = EDGE_LOOP ( 'NONE', ( #19714, #12605, #14002, #22948 ) ) ;
#7549 = CARTESIAN_POINT ( 'NONE',  ( 4.984841277089891776, 200.2242689037093726, 28.44886208192142973 ) ) ;
#7550 = CARTESIAN_POINT ( 'NONE',  ( 80.78867513459482552, 155.0000000000000000, -15.00000000000002487 ) ) ;
#7551 = ORIENTED_EDGE ( 'NONE', *, *, #22218, .F. ) ;
#7552 = CARTESIAN_POINT ( 'NONE',  ( 4.903702542908601636, 200.1653181626581102, 5.451137918078566180 ) ) ;
#7553 = CARTESIAN_POINT ( 'NONE',  ( -7.375838497908014268, 196.7627149292498530, 89.04886208192142760 ) ) ;
#7554 = CARTESIAN_POINT ( 'NONE',  ( 38.67499999726880588, 141.7447067706911810, 9.630534252274376428 ) ) ;
#7555 = EDGE_LOOP ( 'NONE', ( #30664, #29064 ) ) ;
#7556 = CARTESIAN_POINT ( 'NONE',  ( 43.72499999726881015, 169.8198683612136222, 4.815267126137181997 ) ) ;
#7557 = CARTESIAN_POINT ( 'NONE',  ( 117.5000000000000000, 155.0000000000000000, -6.938893903907228378E-15 ) ) ;
#7558 = CARTESIAN_POINT ( 'NONE',  ( -9.984503880673473830, 210.2968891136704315, 3.651137918078565026 ) ) ;
#7559 = AXIS2_PLACEMENT_3D ( 'NONE', #20749, #7812, #15634 ) ;
#7560 = CARTESIAN_POINT ( 'NONE',  ( 3.044812012439969795, 216.5253028482143520, 75.39886208192143613 ) ) ;
#7561 = CARTESIAN_POINT ( 'NONE',  ( 47.97499999726881015, 169.8198683612136222, 4.815267126137181997 ) ) ;
#7562 = CARTESIAN_POINT ( 'NONE',  ( -52.50000000000002132, 0.000000000000000000, 20.00000000000001776 ) ) ;
#7563 = CARTESIAN_POINT ( 'NONE',  ( 10.01549611932653860, 210.2015048109876716, 13.85113791807856742 ) ) ;
#7564 = DIRECTION ( 'NONE',  ( -1.000000000000000000, -0.000000000000000000, -0.000000000000000000 ) ) ;
#7565 = AXIS2_PLACEMENT_3D ( 'NONE', #15783, #2844, #18518 ) ;
#7566 = CARTESIAN_POINT ( 'NONE',  ( 65.29999999999999716, 163.5228861582408797, 11.73074641843673049 ) ) ;
#7567 = CARTESIAN_POINT ( 'NONE',  ( -0.05014649552810635652, 196.4853777576173002, 101.7511379180785411 ) ) ;
#7568 = LINE ( 'NONE', #5662, #18598 ) ;
#7569 = CARTESIAN_POINT ( 'NONE',  ( -8.118202686958039038, 201.1607312380087080, 75.20113791807857240 ) ) ;
#7570 = CARTESIAN_POINT ( 'NONE',  ( -27.50000000000000000, 2.688867821578062145, -0.05704280876259919253 ) ) ;
#7571 = CARTESIAN_POINT ( 'NONE',  ( 117.5000000000000000, 129.0854607986834424, -100.8678580070900921 ) ) ;
#7572 = CARTESIAN_POINT ( 'NONE',  ( -7.456977232089471386, 217.1783343296987709, 86.94886208192144750 ) ) ;
#7573 = AXIS2_PLACEMENT_3D ( 'NONE', #4287, #9912, #4631 ) ;
#7574 = CARTESIAN_POINT ( 'NONE',  ( 73.42499999726881299, 168.2552932293087906, -9.630534252274385310 ) ) ;
#7575 = VERTEX_POINT ( 'NONE', #28180 ) ;
#7576 = CARTESIAN_POINT ( 'NONE',  ( -60.91993774119386984, 194.9950632347986641, -0.6485596632537811157 ) ) ;
#7577 = CARTESIAN_POINT ( 'NONE',  ( 36.19999999453762740, 163.5228861582408797, -11.73074641843674470 ) ) ;
#7578 = CARTESIAN_POINT ( 'NONE',  ( -12.01549611932652972, 203.1486557965464499, 93.35113791807857808 ) ) ;
#7579 = CARTESIAN_POINT ( 'NONE',  ( -10.57145583983291992, 206.1290730434410534, 104.2695288710567780 ) ) ;
#7580 = EDGE_LOOP ( 'NONE', ( #491, #16696, #2434, #19920 ) ) ;
#7581 = CARTESIAN_POINT ( 'NONE',  ( 10.01549611932659367, 203.7984951890124421, 88.14886208192143613 ) ) ;
#7582 = CARTESIAN_POINT ( 'NONE',  ( 12.00000000000000711, 207.0476921513415220, 27.99886208192144110 ) ) ;
#7583 = CARTESIAN_POINT ( 'NONE',  ( -54.75000000000000711, -7.347880794884118356E-15, -35.00000000000000000 ) ) ;
#7584 = AXIS2_PLACEMENT_3D ( 'NONE', #16928, #22046, #22214 ) ;
#7585 = CARTESIAN_POINT ( 'NONE',  ( -10.01549611932653860, 203.7984951890123284, 42.35113791807855677 ) ) ;
#7586 = ORIENTED_EDGE ( 'NONE', *, *, #31980, .T. ) ;
#7587 = CARTESIAN_POINT ( 'NONE',  ( -6.139770520408224463, 198.4640165459539389, 98.04886208192141339 ) ) ;
#7588 = AXIS2_PLACEMENT_3D ( 'NONE', #21114, #33566, #28793 ) ;
#7589 = CARTESIAN_POINT ( 'NONE',  ( -4.984841277089726574, 200.2242689037092305, 87.05113791807856671 ) ) ;
#7590 = CARTESIAN_POINT ( 'NONE',  ( 92.60208470531341618, 155.0000000000000000, 13.00000000000002487 ) ) ;
#7591 = ORIENTED_EDGE ( 'NONE', *, *, #13098, .F. ) ;
#7592 = CARTESIAN_POINT ( 'NONE',  ( 4.903702542908435547, 213.8346818373419751, 84.54886208192144181 ) ) ;
#7593 = ORIENTED_EDGE ( 'NONE', *, *, #17095, .T. ) ;
#7594 = CIRCLE ( 'NONE', #22111, 19.99999999999998934 ) ;
#7595 = CARTESIAN_POINT ( 'NONE',  ( 33.81132485994280756, 159.8737954434936057, -15.00000000000002665 ) ) ;
#7596 = VERTEX_POINT ( 'NONE', #20842 ) ;
#7597 = DIRECTION ( 'NONE',  ( 0.7071067811865474617, 0.000000000000000000, -0.7071067811865474617 ) ) ;
#7598 = CARTESIAN_POINT ( 'NONE',  ( 7.984503880673485376, 204.3529502787953902, 59.15113791807857524 ) ) ;
#7599 = CARTESIAN_POINT ( 'NONE',  ( 83.42499999726882720, 168.2552932293087906, -9.630534252274385310 ) ) ;
#7600 = CARTESIAN_POINT ( 'NONE',  ( 34.49999999999999289, -72.99999999999998579, 30.00000000000000000 ) ) ;
#7601 = CARTESIAN_POINT ( 'NONE',  ( 4.984841277089725686, 213.7757310962907411, 91.55113791807858092 ) ) ;
#7602 = LINE ( 'NONE', #20532, #16221 ) ;
#7603 = CARTESIAN_POINT ( 'NONE',  ( 47.20000000000000284, 167.3344367211045096, 8.961492836873468093 ) ) ;
#7604 = CARTESIAN_POINT ( 'NONE',  ( 7.984503880673422316, 209.6470497212048372, 60.84886208192144608 ) ) ;
#7605 = CIRCLE ( 'NONE', #26105, 4.250000000000000000 ) ;
#7606 = CARTESIAN_POINT ( 'NONE',  ( 38.51132485994280330, 163.8167787843871110, 12.13525491562421621 ) ) ;
#7607 = CARTESIAN_POINT ( 'NONE',  ( -3.135527875058821579, 197.5041725223112223, 2.901137918078565914 ) ) ;
#7608 = CARTESIAN_POINT ( 'NONE',  ( -125.0000000000000000, 0.000000000000000000, -35.00000000000000000 ) ) ;
#7609 = CARTESIAN_POINT ( 'NONE',  ( 42.49999999999999289, -72.99999999999998579, -20.00000000000000000 ) ) ;
#7610 = CARTESIAN_POINT ( 'NONE',  ( 59.42499999726880588, 168.2552932293087906, -9.630534252274387086 ) ) ;
#7611 = CARTESIAN_POINT ( 'NONE',  ( 67.67499999726881299, 168.2552932293087906, -9.630534252274385310 ) ) ;
#7612 = CARTESIAN_POINT ( 'NONE',  ( 7.456977232089302632, 217.1783343296989131, 67.55113791807856671 ) ) ;
#7613 = CARTESIAN_POINT ( 'NONE',  ( 105.9028607166213192, 155.0000000000000000, 0.000000000000000000 ) ) ;
#7614 = CARTESIAN_POINT ( 'NONE',  ( 9.736236675707914401, 214.0148392665762458, 13.70113791807856707 ) ) ;
#7615 = CARTESIAN_POINT ( 'NONE',  ( -6.220909254589537696, 198.5229672870051445, 87.05113791807856671 ) ) ;
#7616 = CARTESIAN_POINT ( 'NONE',  ( -9.680171189290716072, 199.9079932115567146, 56.19886208192144039 ) ) ;
#7617 = CARTESIAN_POINT ( 'NONE',  ( -10.00000000000000711, 206.9523078486584495, 56.49886208192143755 ) ) ;
#7618 = DIRECTION ( 'NONE',  ( 0.000000000000000000, 0.000000000000000000, -1.000000000000000000 ) ) ;
#7619 = CARTESIAN_POINT ( 'NONE',  ( -9.736236675707914401, 199.9851607334237542, 99.20113791807858661 ) ) ;
#7620 = CARTESIAN_POINT ( 'NONE',  ( 68.31132485994278625, 169.2658477444273331, 4.635254915624208216 ) ) ;
#7621 = CARTESIAN_POINT ( 'NONE',  ( 3.044812012440130555, 197.4746971517856764, -0.3988620819214342972 ) ) ;
#7622 = CARTESIAN_POINT ( 'NONE',  ( -6.139770520408224463, 198.4640165459539389, 68.04886208192142760 ) ) ;
#7623 = EDGE_CURVE ( 'NONE', #610, #23163, #18711, .T. ) ;
#7624 = EDGE_LOOP ( 'NONE', ( #7154, #11094, #19759, #328, #5716 ) ) ;
#7625 = CARTESIAN_POINT ( 'NONE',  ( -3.662846001189865142, 195.5725841191952838, 79.89886208192143613 ) ) ;
#7626 = CARTESIAN_POINT ( 'NONE',  ( 6.139770520408368348, 198.4640165459539674, 92.45113791807857240 ) ) ;
#7627 = ORIENTED_EDGE ( 'NONE', *, *, #10604, .T. ) ;
#7628 = CARTESIAN_POINT ( 'NONE',  ( 81.27499999726877888, 149.9369285172503510, -15.58253175000000823 ) ) ;
#7629 = CARTESIAN_POINT ( 'NONE',  ( 7.984503880673422316, 209.6470497212048372, 54.84886208192144608 ) ) ;
#7630 = EDGE_LOOP ( 'NONE', ( #17846, #14093, #16426, #11938, #7709, #13815 ) ) ;
#7631 =( BOUNDED_CURVE ( )  B_SPLINE_CURVE ( 2, ( #30758, #12528, #25640, #17463, #28370, #25815, #5192, #2306, #12860, #33477, #28023 ),
 .UNSPECIFIED., .F., .F. ) 
 B_SPLINE_CURVE_WITH_KNOTS ( ( 3, 2, 2, 2, 2, 3 ),
 ( 0.8392857142857144126, 0.8428571428571429713, 0.8464285714285715301, 0.8500000000000000888, 0.8535714285714286476, 0.8571428571428572063 ),
 .UNSPECIFIED. ) 
 CURVE ( )  GEOMETRIC_REPRESENTATION_ITEM ( )  RATIONAL_B_SPLINE_CURVE ( ( 0.9999999999999984457, 0.9510565162951549745, 1.000000000000000000, 0.9510565162951534202, 1.000000000000000000, 0.9510565162951534202, 1.000000000000000000, 0.9510565162951534202, 1.000000000000000000, 0.9510565162951518658, 1.000000000000001554 ) ) 
 REPRESENTATION_ITEM ( '' )  );
#7632 = CARTESIAN_POINT ( 'NONE',  ( 73.92499999726881299, 164.1591823560292198, 12.60653300113718167 ) ) ;
#7633 = DIRECTION ( 'NONE',  ( -0.000000000000000000, -0.000000000000000000, 1.000000000000000000 ) ) ;
#7634 = CARTESIAN_POINT ( 'NONE',  ( -57.69437687863553776, 194.9296432668266732, -2.372230612754127499 ) ) ;
#7635 = CARTESIAN_POINT ( 'NONE',  ( 61.92499999726882010, 164.1591823560292198, 12.60653300113718167 ) ) ;
#7636 = CARTESIAN_POINT ( 'NONE',  ( -7.500000000000000000, 4.730921838224027454, -7.493596905200499592 ) ) ;
#7637 = CARTESIAN_POINT ( 'NONE',  ( 8.062137200540822946, 212.9164362838583315, 51.69886208192143329 ) ) ;
#7638 = VERTEX_POINT ( 'NONE', #12505 ) ;
#7639 = CARTESIAN_POINT ( 'NONE',  ( 0.000000000000000000, 0.000000000000000000, -7.381345277524544279 ) ) ;
#7640 = CARTESIAN_POINT ( 'NONE',  ( 7.922281120364393914, -4.573931137438282057, -8.047472243342932430 ) ) ;
#7641 = CARTESIAN_POINT ( 'NONE',  ( -2.517493886309087880, 214.5937144450984135, 39.09886208192143897 ) ) ;
#7642 = CARTESIAN_POINT ( 'NONE',  ( 3.135527875058820690, 216.4958274776887492, 67.40113791807857524 ) ) ;
#7643 = DIRECTION ( 'NONE',  ( -0.000000000000000000, -0.000000000000000000, 1.000000000000000000 ) ) ;
#7644 = CARTESIAN_POINT ( 'NONE',  ( 10.00000000000000711, 206.9523078486586201, 59.00113791807857666 ) ) ;
#7645 = ITEM_DEFINED_TRANSFORMATION ( 'NONE', 'NONE', #692,  #2404 ) ;
#7646 = CARTESIAN_POINT ( 'NONE',  ( 0.05014649552810505201, 217.5146222423826714, 31.25113791807857311 ) ) ;
#7647 = CARTESIAN_POINT ( 'NONE',  ( 8.015496119326531499, 209.5516654185219636, 19.85113791807856387 ) ) ;
#7648 = CARTESIAN_POINT ( 'NONE',  ( -6.500000000000005329, 3.752776749732560813, -6.177802698399430525 ) ) ;
#7649 = CARTESIAN_POINT ( 'NONE',  ( -65.20000000000000284, -7.347880794884118356E-15, 19.29999999999998295 ) ) ;
#7650 = CARTESIAN_POINT ( 'NONE',  ( 40.42499999726881299, 141.7447067706911810, 9.630534252274376428 ) ) ;
#7651 = CARTESIAN_POINT ( 'NONE',  ( -7.456977232089304408, 196.8216656703010301, 36.05113791807855961 ) ) ;
#7652 = FACE_OUTER_BOUND ( 'NONE', #694, .T. ) ;
#7653 = CARTESIAN_POINT ( 'NONE',  ( -9.984503880673473830, 210.2968891136704315, 81.65113791807857524 ) ) ;
#7654 = CARTESIAN_POINT ( 'NONE',  ( 8.118202686958039038, 212.8392687619912635, 55.70113791807857950 ) ) ;
#7655 = DIRECTION ( 'NONE',  ( 0.000000000000000000, 0.000000000000000000, -1.000000000000000000 ) ) ;
#7656 = CARTESIAN_POINT ( 'NONE',  ( 12.01549611932659367, 203.1486557965466773, 25.14886208192143258 ) ) ;
#7657 = CARTESIAN_POINT ( 'NONE',  ( 10.01549611932659367, 203.7984951890124421, 31.14886208192143613 ) ) ;
#7658 = CARTESIAN_POINT ( 'NONE',  ( 73.19999999453763451, 146.4771138417591203, 11.73074641843673227 ) ) ;
#7659 = ORIENTED_EDGE ( 'NONE', *, *, #12243, .T. ) ;
#7660 = CARTESIAN_POINT ( 'NONE',  ( 11.98450388067348271, 203.0532714938637753, 71.15113791807857524 ) ) ;
#7661 = CARTESIAN_POINT ( 'NONE',  ( 4.903702542908601636, 200.1653181626581102, 83.45113791807857240 ) ) ;
#7662 = CARTESIAN_POINT ( 'NONE',  ( 3.135527875058981895, 197.5041725223112792, 43.59886208192143897 ) ) ;
#7663 = EDGE_CURVE ( 'NONE', #5501, #10405, #33627, .T. ) ;
#7664 = CARTESIAN_POINT ( 'NONE',  ( 75.71132485994280614, 155.0000000000000000, -15.00000000000002487 ) ) ;
#7665 = ORIENTED_EDGE ( 'NONE', *, *, #28275, .T. ) ;
#7666 = CARTESIAN_POINT ( 'NONE',  ( -3.753561863808878130, 218.3979405102790281, 51.09886208192143897 ) ) ;
#7667 = EDGE_LOOP ( 'NONE', ( #14684, #22306 ) ) ;
#7668 = VERTEX_POINT ( 'NONE', #10306 ) ;
#7669 = CARTESIAN_POINT ( 'NONE',  ( 32.50000000000000000, 155.0000000000000000, -6.938893903907228378E-15 ) ) ;
#7670 = EDGE_CURVE ( 'NONE', #23420, #10127, #20682, .T. ) ;
#7671 = CARTESIAN_POINT ( 'NONE',  ( 1.750000000000016209, -3.031088913245524985, 0.000000000000000000 ) ) ;
#7672 = VERTEX_POINT ( 'NONE', #2629 ) ;
#7673 = CARTESIAN_POINT ( 'NONE',  ( 2.426778023690261410, 199.3768101843759837, 44.60113791807857098 ) ) ;
#7674 = CARTESIAN_POINT ( 'NONE',  ( 44.78867513459481842, 155.0000000000000000, -15.00000000000002487 ) ) ;
#7675 = CARTESIAN_POINT ( 'NONE',  ( 3.135527875058981895, 197.5041725223112792, 19.59886208192143542 ) ) ;
#7676 = CARTESIAN_POINT ( 'NONE',  ( 65.97499999726881015, 169.8198683612136222, 4.815267126137181997 ) ) ;
#7677 = ORIENTED_EDGE ( 'NONE', *, *, #27899, .T. ) ;
#7678 = CARTESIAN_POINT ( 'NONE',  ( 5.047120108843200725, -5.746297884371399434, -0.1007566405101860824 ) ) ;
#7679 = PRESENTATION_STYLE_ASSIGNMENT (( #9893 ) ) ;
#7680 = DIRECTION ( 'NONE',  ( 0.8660254037844381525, -0.5000000000000007772, 0.000000000000000000 ) ) ;
#7681 = CARTESIAN_POINT ( 'NONE',  ( 0.05014649552828262524, 198.5883022060938572, 4.748862081921434886 ) ) ;
#7682 = CARTESIAN_POINT ( 'NONE',  ( -8.062137200540920645, 212.9164362838581894, 39.80113791807857382 ) ) ;
#7683 = EDGE_CURVE ( 'NONE', #3136, #27139, #31245, .T. ) ;
#7684 = CARTESIAN_POINT ( 'NONE',  ( -3.044812012440131443, 216.5253028482142952, 28.10113791807857098 ) ) ;
#7685 = DIRECTION ( 'NONE',  ( 0.000000000000000000, -0.04769215134144032253, 0.9988620819214358848 ) ) ;
#7686 = PRODUCT_CONTEXT ( 'NONE', #29882, 'mechanical' ) ;
#7687 = VECTOR ( 'NONE', #19891, 1000.000000000000000 ) ;
#7688 = CARTESIAN_POINT ( 'NONE',  ( -2.517493886309087880, 214.5937144450984135, 81.09886208192143897 ) ) ;
#7689 = CARTESIAN_POINT ( 'NONE',  ( 34.92499999726881299, 145.8408176439707802, -12.60653300113719588 ) ) ;
#7690 = CARTESIAN_POINT ( 'NONE',  ( 119.7500000000000000, 3.125910954823619074E-14, -35.00000000000000000 ) ) ;
#7691 = FACE_OUTER_BOUND ( 'NONE', #29821, .T. ) ;
#7692 = CARTESIAN_POINT ( 'NONE',  ( 3.662846001190051659, 195.5725841191953691, 11.60113791807856742 ) ) ;
#7693 = CARTESIAN_POINT ( 'NONE',  ( 48.38867513459482694, 140.7341522555726669, -4.635254915624220651 ) ) ;
#7694 = CARTESIAN_POINT ( 'NONE',  ( 53.77499999726881441, 169.8198683612136222, -4.815267126137197984 ) ) ;
#7695 = ADVANCED_FACE ( 'NONE', ( #15729 ), #28003, .F. ) ;
#7696 = CARTESIAN_POINT ( 'NONE',  ( -8.118202686958039038, 201.1607312380087080, 54.20113791807857240 ) ) ;
#7697 = CARTESIAN_POINT ( 'NONE',  ( 34.81132485994281467, 150.1262045565062522, 14.99999999999989697 ) ) ;
#7698 = DIRECTION ( 'NONE',  ( -0.9945218953682714025, 0.000000000000000000, 0.1045284632676720116 ) ) ;
#7699 = CARTESIAN_POINT ( 'NONE',  ( -8.118202686958138514, 212.8392687619910930, 2.798862081921434708 ) ) ;
#7700 = CARTESIAN_POINT ( 'NONE',  ( 52.89999999453763024, 159.7113355953771077, 14.49999999999999289 ) ) ;
#7701 = ORIENTED_EDGE ( 'NONE', *, *, #25197, .T. ) ;
#7702 = CARTESIAN_POINT ( 'NONE',  ( 7.375838497908181246, 196.7627149292499666, 41.45113791807857240 ) ) ;
#7703 = CARTESIAN_POINT ( 'NONE',  ( 46.91132485994280188, 146.1832212156128890, 12.13525491562421976 ) ) ;
#7704 = CARTESIAN_POINT ( 'NONE',  ( -10.01549611932659722, 210.2015048109875011, 14.64886208192143258 ) ) ;
#7705 = CARTESIAN_POINT ( 'NONE',  ( 95.59906517536109050, 155.0000000000000000, -31.00000000000000000 ) ) ;
#7706 = ORIENTED_EDGE ( 'NONE', *, *, #11621, .T. ) ;
#7707 = CARTESIAN_POINT ( 'NONE',  ( -9.984503880673473830, 210.2968891136704315, 12.65113791807856281 ) ) ;
#7708 = CARTESIAN_POINT ( 'NONE',  ( 6.139770520408368348, 198.4640165459539674, 68.45113791807858661 ) ) ;
#7709 = ORIENTED_EDGE ( 'NONE', *, *, #24398, .T. ) ;
#7710 = CARTESIAN_POINT ( 'NONE',  ( -2.426778023690076225, 199.3768101843759553, 28.89886208192143613 ) ) ;
#7711 = CARTESIAN_POINT ( 'NONE',  ( 44.31132485994280046, 169.2658477444273331, 4.635254915624208216 ) ) ;
#7712 = ORIENTED_EDGE ( 'NONE', *, *, #8553, .T. ) ;
#7713 = CARTESIAN_POINT ( 'NONE',  ( -4.903702542908602524, 213.8346818373418898, 15.95113791807856707 ) ) ;
#7714 = EDGE_CURVE ( 'NONE', #21804, #19123, #4304, .T. ) ;
#7715 = EDGE_CURVE ( 'NONE', #10473, #546, #21711, .T. ) ;
#7716 = CARTESIAN_POINT ( 'NONE',  ( -0.05014649552828442242, 219.6175466908591716, 102.2488620819214447 ) ) ;
#7717 = CARTESIAN_POINT ( 'NONE',  ( 45.27499999726880731, 149.9369285172503510, -15.58253175000000823 ) ) ;
#7718 = ORIENTED_EDGE ( 'NONE', *, *, #26985, .F. ) ;
#7719 = CARTESIAN_POINT ( 'NONE',  ( 51.22499999726881015, 160.0630714827496206, -15.58253175000000823 ) ) ;
#7720 = CARTESIAN_POINT ( 'NONE',  ( 123.6258236071137731, 5.113356552508689923, 35.00001199999999812 ) ) ;
#7721 = CARTESIAN_POINT ( 'NONE',  ( 0.05014649552810505201, 217.5146222423826714, 10.25113791807856778 ) ) ;
#7722 = CARTESIAN_POINT ( 'NONE',  ( 0.05014649552828275708, 196.4853777576173002, 70.74886208192143044 ) ) ;
#7723 = CARTESIAN_POINT ( 'NONE',  ( 46.77499999726881441, 140.1801316387863778, 4.815267126137185549 ) ) ;
#7724 = CARTESIAN_POINT ( 'NONE',  ( -67.50001199999999812, 138.8682562219734109, 5.477666192157156999 ) ) ;
#7725 = CARTESIAN_POINT ( 'NONE',  ( 6.139770520408368348, 198.4640165459539674, 11.45113791807856707 ) ) ;
#7726 = CYLINDRICAL_SURFACE ( 'NONE', #6162, 4.199999999999988631 ) ;
#7727 = EDGE_CURVE ( 'NONE', #6493, #1409, #24418, .T. ) ;
#7728 = CARTESIAN_POINT ( 'NONE',  ( 67.50000000000000000, 155.0000000000000000, 14.49999999999999467 ) ) ;
#7729 = CARTESIAN_POINT ( 'NONE',  ( 8.062137200540920645, 201.0835637161417822, 98.30113791807858092 ) ) ;
#7730 = CARTESIAN_POINT ( 'NONE',  ( 38.78867513459481842, 155.0000000000000000, -15.00000000000002487 ) ) ;
#7731 = CARTESIAN_POINT ( 'NONE',  ( 3.044812012440130555, 197.4746971517856764, 86.60113791807857808 ) ) ;
#7732 = CARTESIAN_POINT ( 'NONE',  ( -27.50000000000000000, 6.731471899275967452, -0.4522261538067093301 ) ) ;
#7733 = CARTESIAN_POINT ( 'NONE',  ( 92.60208470531341618, 155.0000000000000000, 0.000000000000000000 ) ) ;
#7734 = EDGE_CURVE ( 'NONE', #1695, #25076, #24402, .T. ) ;
#7735 = CARTESIAN_POINT ( 'NONE',  ( -0.05014649552828442242, 219.6175466908591716, 96.24886208192144466 ) ) ;
#7736 = CARTESIAN_POINT ( 'NONE',  ( 69.82499999726880446, 168.2552932293087906, 9.630534252274372875 ) ) ;
#7737 = VERTEX_POINT ( 'NONE', #18788 ) ;
#7738 = CYLINDRICAL_SURFACE ( 'NONE', #32579, 2.149999999999994138 ) ;
#7739 = AXIS2_PLACEMENT_3D ( 'NONE', #17395, #30007, #20287 ) ;
#7740 = CARTESIAN_POINT ( 'NONE',  ( 86.37499999726881583, 155.0000000000000000, 15.58253174999999402 ) ) ;
#7741 = CARTESIAN_POINT ( 'NONE',  ( 7.456977232089302632, 217.1783343296989131, 100.5511379180785809 ) ) ;
#7742 = CARTESIAN_POINT ( 'NONE',  ( 1.500000000000001332, 9.797174393178825657E-16, -8.000000000000000000 ) ) ;
#7743 = ORIENTED_EDGE ( 'NONE', *, *, #15182, .F. ) ;
#7744 = CARTESIAN_POINT ( 'NONE',  ( 9.984503880673420539, 210.2968891136705736, 81.84886208192143897 ) ) ;
#7745 = CONICAL_SURFACE ( 'NONE', #8788, 32.00000000000002842, 0.1047197551196784177 ) ;
#7746 = CARTESIAN_POINT ( 'NONE',  ( 9.736236675708031640, 199.9851607334238963, 25.29886208192143826 ) ) ;
#7747 = DIRECTION ( 'NONE',  ( 1.000000000000000000, 0.000000000000000000, 0.000000000000000000 ) ) ;
#7748 = CARTESIAN_POINT ( 'NONE',  ( -8.062137200540920645, 212.9164362838581894, 45.80113791807856671 ) ) ;
#7749 = ORIENTED_EDGE ( 'NONE', *, *, #4342, .F. ) ;
#7750 = CARTESIAN_POINT ( 'NONE',  ( -4.984841277089891776, 213.7757310962905990, 5.948862081921435063 ) ) ;
#7751 = FACE_OUTER_BOUND ( 'NONE', #1183, .T. ) ;
#7752 = ORIENTED_EDGE ( 'NONE', *, *, #8496, .T. ) ;
#7753 = CARTESIAN_POINT ( 'NONE',  ( 2.517493886309087436, 199.4062855549015865, 88.59886208192143897 ) ) ;
#7754 = ORIENTED_EDGE ( 'NONE', *, *, #10342, .F. ) ;
#7755 = CARTESIAN_POINT ( 'NONE',  ( 6.500168698208129925, 211.6636982574063381, 34.70113791807857240 ) ) ;
#7756 = DIRECTION ( 'NONE',  ( -0.000000000000000000, -0.000000000000000000, 1.000000000000000000 ) ) ;
#7757 = VERTEX_POINT ( 'NONE', #28847 ) ;
#7758 = DIRECTION ( 'NONE',  ( -1.000000000000000000, 0.000000000000000000, 0.000000000000000000 ) ) ;
#7759 = AXIS2_PLACEMENT_3D ( 'NONE', #13361, #21032, #18647 ) ;
#7760 = CARTESIAN_POINT ( 'NONE',  ( 84.52499999726880731, 140.1801316387863778, 4.815267126137185549 ) ) ;
#7761 = LINE ( 'NONE', #23428, #2913 ) ;
#7762 = CARTESIAN_POINT ( 'NONE',  ( 4.903702542908601636, 200.1653181626581102, 89.45113791807857240 ) ) ;
#7763 = CARTESIAN_POINT ( 'NONE',  ( -125.0000000000000000, 25.00000000000000000, 35.00000000000000000 ) ) ;
#7765 = CIRCLE ( 'NONE', #26783, 17.00000000000000355 ) ;
#7764 = DIRECTION ( 'NONE',  ( 1.000000000000000000, 0.000000000000000000, 0.000000000000000000 ) ) ;
#7766 = CARTESIAN_POINT ( 'NONE',  ( 49.80000000000000426, 142.6655632788954620, 8.961492836873471646 ) ) ;
#7767 = CARTESIAN_POINT ( 'NONE',  ( 4.984841277089891776, 200.2242689037093726, 61.44886208192144039 ) ) ;
#7768 = DIRECTION ( 'NONE',  ( -0.9891821073486152249, -0.1466927349985424900, -2.962715634069391535E-17 ) ) ;
#7769 = AXIS2_PLACEMENT_3D ( 'NONE', #13707, #32277, #11504 ) ;
#7770 = CARTESIAN_POINT ( 'NONE',  ( 53.52499999726881441, 169.8198683612136222, -4.815267126137197984 ) ) ;
#7771 = LINE ( 'NONE', #5040, #5586 ) ;
#7772 = CYLINDRICAL_SURFACE ( 'NONE', #22768, 24.99999999999999289 ) ;
#7773 = CARTESIAN_POINT ( 'NONE',  ( 60.32499999726881157, 145.8408176439707802, 12.60653300113718345 ) ) ;
#7774 = CARTESIAN_POINT ( 'NONE',  ( 67.77499999726880731, 169.8198683612136222, -4.815267126137197984 ) ) ;
#7775 = CARTESIAN_POINT ( 'NONE',  ( 7.456977232089302632, 217.1783343296989131, 64.55113791807856671 ) ) ;
#7776 = CARTESIAN_POINT ( 'NONE',  ( 64.50000000000000000, -73.00000000000000000, 30.00000000000000000 ) ) ;
#7777 = CARTESIAN_POINT ( 'NONE',  ( 9.680171189290831535, 199.9079932115568852, 8.301137918078564937 ) ) ;
#7778 = CARTESIAN_POINT ( 'NONE',  ( 6.139770520408367460, 198.4640165459539389, 89.45113791807857240 ) ) ;
#7779 = CARTESIAN_POINT ( 'NONE',  ( -0.05014649552828442242, 219.6175466908591716, 48.24886208192144466 ) ) ;
#7780 = VECTOR ( 'NONE', #3568, 1000.000000000000000 ) ;
#7781 = CARTESIAN_POINT ( 'NONE',  ( -10.00000000000000711, 206.9523078486584495, 53.49886208192143755 ) ) ;
#7782 = CARTESIAN_POINT ( 'NONE',  ( -3.753561863808691168, 195.6020594897209435, 95.90113791807857524 ) ) ;
#7783 = DIRECTION ( 'NONE',  ( 0.000000000000000000, 0.000000000000000000, -1.000000000000000000 ) ) ;
#7784 = CARTESIAN_POINT ( 'NONE',  ( 8.118202686958039038, 212.8392687619912635, 13.70113791807856707 ) ) ;
#7785 = CARTESIAN_POINT ( 'NONE',  ( -8.062137200540822946, 201.0835637161416400, 77.19886208192143329 ) ) ;
#7786 = VERTEX_POINT ( 'NONE', #29348 ) ;
#7787 = CARTESIAN_POINT ( 'NONE',  ( 7.456977232089471386, 196.8216656703012006, 79.44886208192144750 ) ) ;
#7788 = CARTESIAN_POINT ( 'NONE',  ( -9.984503880673473830, 210.2968891136704315, 96.65113791807857524 ) ) ;
#7789 = AXIS2_PLACEMENT_3D ( 'NONE', #28682, #5341, #2632 ) ;
#7790 = ORIENTED_EDGE ( 'NONE', *, *, #30352, .T. ) ;
#7791 = CARTESIAN_POINT ( 'NONE',  ( 76.27499999726877888, 160.0630714827496206, 15.58253174999999402 ) ) ;
#7792 = CARTESIAN_POINT ( 'NONE',  ( 6.444103211790928043, 211.7408657792734061, 54.69886208192144039 ) ) ;
#7793 = ORIENTED_EDGE ( 'NONE', *, *, #31597, .F. ) ;
#7794 = CIRCLE ( 'NONE', #13755, 2.149999999999985256 ) ;
#7795 = CARTESIAN_POINT ( 'NONE',  ( 69.22499999726881015, 160.0630714827496206, -15.58253175000000823 ) ) ;
#7796 = FACE_BOUND ( 'NONE', #12090, .T. ) ;
#7797 = CARTESIAN_POINT ( 'NONE',  ( 92.60208470531341618, 155.0000000000000000, 0.000000000000000000 ) ) ;
#7798 = CARTESIAN_POINT ( 'NONE',  ( 63.02499999726882152, 149.9369285172503510, -15.58253175000000823 ) ) ;
#7799 = CARTESIAN_POINT ( 'NONE',  ( -7.894706624614703294, -0.7534108004380160040, -7.590222617908770175 ) ) ;
#7800 = CARTESIAN_POINT ( 'NONE',  ( -0.05014649552828403384, 217.5146222423826714, 51.24886208192143755 ) ) ;
#7801 = ORIENTED_EDGE ( 'NONE', *, *, #30794, .T. ) ;
#7802 = CARTESIAN_POINT ( 'NONE',  ( 4.000000000000000000, 3.518949890710768802, -4.770489558936219510E-15 ) ) ;
#7803 = AXIS2_PLACEMENT_3D ( 'NONE', #4921, #4748, #7655 ) ;
#7804 = CARTESIAN_POINT ( 'NONE',  ( -60.00000000000000000, -7.347880794884118356E-15, -20.00000000000001776 ) ) ;
#7805 = CARTESIAN_POINT ( 'NONE',  ( -7.984503880673422316, 204.3529502787951628, 32.34886208192143897 ) ) ;
#7806 = CARTESIAN_POINT ( 'NONE',  ( -10.00000000000000711, 207.0476921513413515, 66.50113791807856956 ) ) ;
#7807 = CARTESIAN_POINT ( 'NONE',  ( 44.98867513459482836, 163.8167787843871110, -12.13525491562423397 ) ) ;
#7808 = ADVANCED_FACE ( 'NONE', ( #31566 ), #21180, .T. ) ;
#7809 = CARTESIAN_POINT ( 'NONE',  ( 8.062137200540920645, 201.0835637161417822, 56.30113791807857382 ) ) ;
#7810 = CARTESIAN_POINT ( 'NONE',  ( 10.00000000000000711, 206.9523078486586201, 32.00113791807856956 ) ) ;
#7811 = CARTESIAN_POINT ( 'NONE',  ( 4.984841277089725686, 213.7757310962907411, 16.55113791807857027 ) ) ;
#7812 = DIRECTION ( 'NONE',  ( 0.000000000000000000, -1.000000000000000000, 0.000000000000000000 ) ) ;
#7813 = VECTOR ( 'NONE', #5726, 1000.000000000000114 ) ;
#7814 = FACE_OUTER_BOUND ( 'NONE', #8127, .T. ) ;
#7815 = CARTESIAN_POINT ( 'NONE',  ( 36.72499999726881015, 140.1801316387863778, -4.815267126137194431 ) ) ;
#7816 = CARTESIAN_POINT ( 'NONE',  ( -11.98450388067348804, 210.9467285061362247, 36.65113791807856103 ) ) ;
#7817 = CARTESIAN_POINT ( 'NONE',  ( 5.698650001973517121, -4.592339236403569558, -6.344532336093708480 ) ) ;
#7818 = AXIS2_PLACEMENT_3D ( 'NONE', #15570, #15903, #5185 ) ;
#7819 = CARTESIAN_POINT ( 'NONE',  ( 6.220909254589536808, 215.4770327129947702, 85.55113791807858092 ) ) ;
#7820 = CARTESIAN_POINT ( 'NONE',  ( 8.062137200540920645, 201.0835637161417822, 56.30113791807857382 ) ) ;
#7821 = AXIS2_PLACEMENT_3D ( 'NONE', #1400, #27129, #1229 ) ;
#7822 = DIRECTION ( 'NONE',  ( 1.000000000000000000, -0.000000000000000000, -0.000000000000000000 ) ) ;
#7823 = CARTESIAN_POINT ( 'NONE',  ( -9.680171189290716072, 199.9079932115567146, 23.19886208192143684 ) ) ;
#7824 = CARTESIAN_POINT ( 'NONE',  ( -3.135527875058982783, 216.4958274776886924, 24.09886208192143542 ) ) ;
#7825 = CARTESIAN_POINT ( 'NONE',  ( 77.79999999453762882, 146.4771138417591203, -11.73074641843674470 ) ) ;
#7826 = CARTESIAN_POINT ( 'NONE',  ( -11.98450388067348804, 210.9467285061362247, 63.65113791807855392 ) ) ;
#7827 = CARTESIAN_POINT ( 'NONE',  ( 4.903702542908601636, 200.1653181626581102, 86.45113791807858661 ) ) ;
#7828 =( BOUNDED_CURVE ( )  B_SPLINE_CURVE ( 2, ( #24196, #11252, #18758, #32030, #2923, #18915, #5789, #26252, #26920, #10602, #16185 ),
 .UNSPECIFIED., .F., .T. ) 
 B_SPLINE_CURVE_WITH_KNOTS ( ( 3, 2, 2, 2, 2, 3 ),
 ( 0.4464285714285713969, 0.4499999999999999556, 0.4535714285714285143, 0.4571428571428570731, 0.4607142857142856318, 0.4642857142857142461 ),
 .UNSPECIFIED. ) 
 CURVE ( )  GEOMETRIC_REPRESENTATION_ITEM ( )  RATIONAL_B_SPLINE_CURVE ( ( 1.000000000000000666, 0.9510565162951526430, 1.000000000000000000, 0.9510565162951534202, 1.000000000000000000, 0.9510565162951534202, 1.000000000000000000, 0.9510565162951534202, 1.000000000000000000, 0.9510565162951541973, 0.9999999999999992228 ) ) 
 REPRESENTATION_ITEM ( '' )  );
#7829 = CARTESIAN_POINT ( 'NONE',  ( -10.01549611932659722, 210.2015048109875011, 44.64886208192143613 ) ) ;
#7830 = LINE ( 'NONE', #33213, #368 ) ;
#7831 = ORIENTED_EDGE ( 'NONE', *, *, #33511, .F. ) ;
#7832 = CARTESIAN_POINT ( 'NONE',  ( 3.662846001189864698, 218.4274158808046593, 51.39886208192144323 ) ) ;
#7833 = STYLED_ITEM ( 'NONE', ( #7679 ), #1094 ) ;
#7834 = ORIENTED_EDGE ( 'NONE', *, *, #31181, .T. ) ;
#7835 =( GEOMETRIC_REPRESENTATION_CONTEXT ( 3 ) GLOBAL_UNCERTAINTY_ASSIGNED_CONTEXT ( ( #4584 ) ) GLOBAL_UNIT_ASSIGNED_CONTEXT ( ( #13398, #31309, #18358 ) ) REPRESENTATION_CONTEXT ( 'NONE', 'WORKASPACE' ) );
#7836 = EDGE_LOOP ( 'NONE', ( #20686, #24416, #10641, #2396 ) ) ;
#7837 = DIRECTION ( 'NONE',  ( 1.000000000000000000, 0.000000000000000000, 0.000000000000000000 ) ) ;
#7838 = LINE ( 'NONE', #28283, #2391 ) ;
#7839 = ORIENTED_EDGE ( 'NONE', *, *, #13501, .T. ) ;
#7840 = VECTOR ( 'NONE', #20784, 1000.000000000000000 ) ;
#7841 = CARTESIAN_POINT ( 'NONE',  ( 6.500168698208129925, 211.6636982574063381, 40.70113791807857240 ) ) ;
#7842 = CIRCLE ( 'NONE', #749, 3.999999999999999112 ) ;
#7843 = CARTESIAN_POINT ( 'NONE',  ( 82.41132485994280898, 167.7597621252805880, 9.270509831248428867 ) ) ;
#7844 = CARTESIAN_POINT ( 'NONE',  ( -3.135527875058982783, 216.4958274776886924, 27.09886208192143542 ) ) ;
#7845 = CARTESIAN_POINT ( 'NONE',  ( 62.67499999726879878, 141.7447067706911810, 9.630534252274376428 ) ) ;
#7846 = ORIENTED_EDGE ( 'NONE', *, *, #22042, .F. ) ;
#7847 = CARTESIAN_POINT ( 'NONE',  ( 68.38867513459481984, 140.7341522555726669, -4.635254915624220651 ) ) ;
#7848 =( NAMED_UNIT ( * ) SI_UNIT ( $, .STERADIAN. ) SOLID_ANGLE_UNIT ( ) );
#7849 = CARTESIAN_POINT ( 'NONE',  ( 0.000000000000000000, 0.000000000000000000, -2.899999999999999911 ) ) ;
#7850 = CARTESIAN_POINT ( 'NONE',  ( -7.984503880673422316, 204.3529502787951628, 2.348862081921434974 ) ) ;
#7851 = CARTESIAN_POINT ( 'NONE',  ( 3.135527875058820690, 216.4958274776887492, 43.40113791807856813 ) ) ;
#7852 = CARTESIAN_POINT ( 'NONE',  ( 36.71132485994280614, 155.0000000000000000, 15.00000000000001243 ) ) ;
#7853 = EDGE_CURVE ( 'NONE', #4513, #3461, #23729, .T. ) ;
#7854 = CARTESIAN_POINT ( 'NONE',  ( -8.118202686958039038, 201.1607312380087080, 24.20113791807856884 ) ) ;
#7855 = CARTESIAN_POINT ( 'NONE',  ( 10.01549611932659367, 203.7984951890124421, 100.1488620819214361 ) ) ;
#7856 = CARTESIAN_POINT ( 'NONE',  ( 7.984503880673422316, 209.6470497212048372, 93.84886208192143897 ) ) ;
#7857 = CARTESIAN_POINT ( 'NONE',  ( 35.22499999726881015, 160.0630714827496206, -15.58253175000000823 ) ) ;
#7858 = FILL_AREA_STYLE ('',( #28801 ) ) ;
#7859 = CARTESIAN_POINT ( 'NONE',  ( -2.000000000000000888, 2.449293598294707893E-16, -2.899999999999999911 ) ) ;
#7860 = CARTESIAN_POINT ( 'NONE',  ( 3.753561863808689836, 218.3979405102790565, 13.40113791807856636 ) ) ;
#7861 = CARTESIAN_POINT ( 'NONE',  ( 0.000000000000000000, 0.000000000000000000, -10.00000000000000000 ) ) ;
#7862 = CARTESIAN_POINT ( 'NONE',  ( 60.17499999726881299, 164.1591823560292198, 12.60653300113718167 ) ) ;
#7863 = CARTESIAN_POINT ( 'NONE',  ( -8.062137200540920645, 212.9164362838581894, 51.80113791807857382 ) ) ;
#7864 = CYLINDRICAL_SURFACE ( 'NONE', #20831, 15.00000000000001776 ) ;
#7865 = EDGE_CURVE ( 'NONE', #6856, #5501, #25002, .T. ) ;
#7866 = CARTESIAN_POINT ( 'NONE',  ( 7.500000000000000000, 4.330127018922190096, -10.00000000000000000 ) ) ;
#7867 = CARTESIAN_POINT ( 'NONE',  ( 105.0000000000000142, 3.061616997868383121E-14, 35.00200000000000244 ) ) ;
#7868 = CARTESIAN_POINT ( 'NONE',  ( 51.89999999453762314, 150.2886644046228639, -14.50000000000000888 ) ) ;
#7869 = EDGE_LOOP ( 'NONE', ( #24489, #16038 ) ) ;
#7870 = CARTESIAN_POINT ( 'NONE',  ( 0.05014649552807549926, 219.6175466908591716, 34.25113791807857666 ) ) ;
#7871 = AXIS2_PLACEMENT_3D ( 'NONE', #991, #21438, #21935 ) ;
#7872 = DIRECTION ( 'NONE',  ( 1.000000000000000000, -0.000000000000000000, -0.000000000000000000 ) ) ;
#7873 = CARTESIAN_POINT ( 'NONE',  ( -8.062137200540822946, 201.0835637161416400, 11.19886208192143506 ) ) ;
#7874 = FACE_OUTER_BOUND ( 'NONE', #18824, .T. ) ;
#7875 = ORIENTED_EDGE ( 'NONE', *, *, #19865, .T. ) ;
#7876 = CARTESIAN_POINT ( 'NONE',  ( -6.220909254589537696, 198.5229672870051161, 12.05113791807856671 ) ) ;
#7877 = CARTESIAN_POINT ( 'NONE',  ( -3.135527875058821579, 197.5041725223112223, 71.90113791807857524 ) ) ;
#7878 = EDGE_CURVE ( 'NONE', #8582, #28277, #23384, .T. ) ;
#7879 = VERTEX_POINT ( 'NONE', #26448 ) ;
#7880 = CARTESIAN_POINT ( 'NONE',  ( -2.426778023690076225, 199.3768101843759553, 34.89886208192144323 ) ) ;
#7881 = PRESENTATION_LAYER_ASSIGNMENT (  '', '', ( #32320 ) ) ;
#7882 = CARTESIAN_POINT ( 'NONE',  ( -64.50000000000000000, -95.00000000000000000, 20.00000000000001776 ) ) ;
#7883 = ORIENTED_EDGE ( 'NONE', *, *, #18291, .F. ) ;
#7884 = CARTESIAN_POINT ( 'NONE',  ( 4.903702542908601636, 200.1653181626581102, 11.45113791807856529 ) ) ;
#7885 = EDGE_CURVE ( 'NONE', #21434, #6342, #22819, .T. ) ;
#7886 = CARTESIAN_POINT ( 'NONE',  ( 7.456977232089471386, 196.8216656703012006, 94.44886208192143329 ) ) ;
#7887 = CARTESIAN_POINT ( 'NONE',  ( 41.97499999726881015, 169.8198683612136222, 4.815267126137181997 ) ) ;
#7888 = ORIENTED_EDGE ( 'NONE', *, *, #5436, .F. ) ;
#7889 = CARTESIAN_POINT ( 'NONE',  ( 52.12499999726881583, 155.0000000000000000, 15.58253174999999402 ) ) ;
#7890 = DIRECTION ( 'NONE',  ( -1.000000000000000000, 0.000000000000000000, -0.000000000000000000 ) ) ;
#7891 = CARTESIAN_POINT ( 'NONE',  ( -3.135527875058821579, 197.5041725223112223, 11.90113791807856636 ) ) ;
#7892 = CARTESIAN_POINT ( 'NONE',  ( 10.00000000000000711, 207.0476921513415220, 81.99886208192143044 ) ) ;
#7893 = CARTESIAN_POINT ( 'NONE',  ( 52.47499999726881015, 149.9369285172503510, 15.58253174999999580 ) ) ;
#7894 = CARTESIAN_POINT ( 'NONE',  ( 79.51132485994280330, 146.1832212156128890, -12.13525491562423042 ) ) ;
#7895 = CARTESIAN_POINT ( 'NONE',  ( 3.135527875058820690, 216.4958274776887492, 16.40113791807856813 ) ) ;
#7896 = DIRECTION ( 'NONE',  ( 1.000000000000000000, 0.000000000000000000, 0.000000000000000000 ) ) ;
#7897 = EDGE_CURVE ( 'NONE', #20665, #16872, #16820, .T. ) ;
#7898 = CARTESIAN_POINT ( 'NONE',  ( 66.50000000000000000, 155.0000000000000000, -14.50000000000000711 ) ) ;
#7899 = DIRECTION ( 'NONE',  ( 0.000000000000000000, -0.4999999999999990563, 0.8660254037844391517 ) ) ;
#7900 = CARTESIAN_POINT ( 'NONE',  ( 16.66875746037182537, 22.13055319862716175, -0.1142222407377223303 ) ) ;
#7901 = CARTESIAN_POINT ( 'NONE',  ( 3.135527875058820690, 216.4958274776887492, 88.40113791807857524 ) ) ;
#7902 = FACE_OUTER_BOUND ( 'NONE', #19210, .T. ) ;
#7903 = CARTESIAN_POINT ( 'NONE',  ( 36.47499999726881015, 149.9369285172503510, 15.58253174999999580 ) ) ;
#7904 = CARTESIAN_POINT ( 'NONE',  ( -3.662846001189865142, 195.5725841191952838, 100.8988620819214361 ) ) ;
#7905 = CARTESIAN_POINT ( 'NONE',  ( 71.52499999726882152, 169.8198683612136222, -4.815267126137197984 ) ) ;
#7906 = ORIENTED_EDGE ( 'NONE', *, *, #32091, .T. ) ;
#7907 = CARTESIAN_POINT ( 'NONE',  ( -60.48684543773389066, 194.9711049089068808, 1.526260319620769579 ) ) ;
#7908 = CARTESIAN_POINT ( 'NONE',  ( 37.99999999453762456, 155.0000000000000000, -14.50000000000000711 ) ) ;
#7909 = CARTESIAN_POINT ( 'NONE',  ( 11.98450388067348271, 203.0532714938637753, 98.15113791807856103 ) ) ;
#7910 = PRODUCT_DEFINITION_SHAPE ( 'NONE', 'NONE',  #33704 ) ;
#7911 = EDGE_CURVE ( 'NONE', #23405, #14849, #9758, .T. ) ;
#7912 = DIRECTION ( 'NONE',  ( 1.000000000000000000, 0.000000000000000000, 0.000000000000000000 ) ) ;
#7913 = EDGE_LOOP ( 'NONE', ( #6052, #24624, #29853, #24629, #19097, #24379, #25639 ) ) ;
#7914 = CARTESIAN_POINT ( 'NONE',  ( 8.118202686958138514, 201.1607312380088501, 85.29886208192144181 ) ) ;
#7915 = CARTESIAN_POINT ( 'NONE',  ( 9.736236675708031640, 199.9851607334238963, 19.29886208192143471 ) ) ;
#7916 = CARTESIAN_POINT ( 'NONE',  ( 2.000000000000000000, 0.8865213383406687075, -1.535500000000000975 ) ) ;
#7917 = CARTESIAN_POINT ( 'NONE',  ( -0.05014649552810635652, 196.4853777576173002, 41.75113791807855534 ) ) ;
#7918 = ORIENTED_EDGE ( 'NONE', *, *, #26651, .F. ) ;
#7919 = EDGE_CURVE ( 'NONE', #3834, #3719, #23594, .T. ) ;
#7920 = CARTESIAN_POINT ( 'NONE',  ( 6.444103211790928043, 211.7408657792734061, 6.698862081921435063 ) ) ;
#7921 = DIRECTION ( 'NONE',  ( 1.000000000000000000, -4.625929269271484928E-16, 0.000000000000000000 ) ) ;
#7922 = ORIENTED_EDGE ( 'NONE', *, *, #23130, .F. ) ;
#7923 = CARTESIAN_POINT ( 'NONE',  ( -4.903702542908436435, 200.1653181626580249, 92.04886208192142760 ) ) ;
#7924 = EDGE_CURVE ( 'NONE', #4349, #5869, #18470, .T. ) ;
#7925 = VERTEX_POINT ( 'NONE', #16556 ) ;
#7926 = CARTESIAN_POINT ( 'NONE',  ( -0.05014649552807731031, 198.5883022060938572, 29.75113791807856956 ) ) ;
#7927 = CARTESIAN_POINT ( 'NONE',  ( 67.50000000000000000, 155.0000000000000000, -13.49999999999997691 ) ) ;
#7928 = ORIENTED_EDGE ( 'NONE', *, *, #324, .T. ) ;
#7929 = DIRECTION ( 'NONE',  ( 1.000000000000000000, -0.000000000000000000, -0.000000000000000000 ) ) ;
#7930 = CARTESIAN_POINT ( 'NONE',  ( 86.52499999726882152, 140.1801316387863778, 4.815267126137185549 ) ) ;
#7931 = DIRECTION ( 'NONE',  ( 0.000000000000000000, 0.000000000000000000, 1.000000000000000000 ) ) ;
#7932 = CARTESIAN_POINT ( 'NONE',  ( 6.500168698208129925, 211.6636982574063381, 91.70113791807857240 ) ) ;
#7933 = DIRECTION ( 'NONE',  ( 1.000000000000000000, 1.804112415015879378E-16, 0.000000000000000000 ) ) ;
#7934 = CARTESIAN_POINT ( 'NONE',  ( 0.000000000000000000, 0.000000000000000000, 0.000000000000000000 ) ) ;
#7935 = CARTESIAN_POINT ( 'NONE',  ( 46.90000000000000568, 168.7903194862797420, -4.480746418436745593 ) ) ;
#7936 = CARTESIAN_POINT ( 'NONE',  ( -8.015496119326597224, 209.5516654185217362, 62.64886208192143613 ) ) ;
#7937 = FACE_OUTER_BOUND ( 'NONE', #9195, .T. ) ;
#7938 = CARTESIAN_POINT ( 'NONE',  ( 48.72499999726881725, 140.1801316387863778, -4.815267126137194431 ) ) ;
#7939 = DIRECTION ( 'NONE',  ( 0.000000000000000000, 0.000000000000000000, -1.000000000000000000 ) ) ;
#7940 = DIRECTION ( 'NONE',  ( 1.000000000000000000, 0.000000000000000000, 0.000000000000000000 ) ) ;
#7941 = CARTESIAN_POINT ( 'NONE',  ( 54.82499999726880446, 141.7447067706911810, -9.630534252274387086 ) ) ;
#7942 = CARTESIAN_POINT ( 'NONE',  ( 68.37499999726881583, 155.0000000000000000, 15.58253174999999402 ) ) ;
#7943 = CARTESIAN_POINT ( 'NONE',  ( -9.736236675707914401, 199.9851607334237542, 72.20113791807857240 ) ) ;
#7944 = CARTESIAN_POINT ( 'NONE',  ( 68.78867513459482552, 155.0000000000000000, -15.00000000000002487 ) ) ;
#7945 = CARTESIAN_POINT ( 'NONE',  ( -9.736236675707914401, 199.9851607334237542, 9.201137918078563516 ) ) ;
#7946 = EDGE_CURVE ( 'NONE', #18759, #1785, #6497, .T. ) ;
#7947 = CARTESIAN_POINT ( 'NONE',  ( 8.062137200540920645, 201.0835637161417822, 89.30113791807858092 ) ) ;
#7948 = CARTESIAN_POINT ( 'NONE',  ( 117.5000000000000000, 51.09158283380784837, 28.95509836041906837 ) ) ;
#7949 = CARTESIAN_POINT ( 'NONE',  ( -3.753561863808878130, 218.3979405102790281, 48.09886208192143897 ) ) ;
#7950 = CARTESIAN_POINT ( 'NONE',  ( 10.00000000000000711, 207.0476921513415220, 57.99886208192143044 ) ) ;
#7951 = CARTESIAN_POINT ( 'NONE',  ( -11.98450388067348804, 210.9467285061362247, 99.65113791807858945 ) ) ;
#7952 = CARTESIAN_POINT ( 'NONE',  ( -67.50001199999999812, 172.0000000000000000, 1.112647398146393130 ) ) ;
#7953 = CARTESIAN_POINT ( 'NONE',  ( -10.01549611932653860, 203.7984951890123284, 12.35113791807856387 ) ) ;
#7954 = EDGE_CURVE ( 'NONE', #9032, #12934, #25540, .T. ) ;
#7955 = CARTESIAN_POINT ( 'NONE',  ( 8.062137200540822946, 212.9164362838583315, 81.69886208192143329 ) ) ;
#7956 = ORIENTED_EDGE ( 'NONE', *, *, #26662, .T. ) ;
#7957 = CARTESIAN_POINT ( 'NONE',  ( -9.736236675708031640, 214.0148392665760753, 80.79886208192144181 ) ) ;
#7958 = PLANE ( 'NONE',  #26289 ) ;
#7959 = EDGE_LOOP ( 'NONE', ( #16994, #25241 ) ) ;
#7960 = CARTESIAN_POINT ( 'NONE',  ( 2.818872373871549124E-16, 8.716839668575678601, -7.700121441565840996 ) ) ;
#7961 = CARTESIAN_POINT ( 'NONE',  ( -4.984841277089891776, 213.7757310962905990, 56.94886208192144039 ) ) ;
#7962 = ORIENTED_EDGE ( 'NONE', *, *, #1054, .T. ) ;
#7963 = CARTESIAN_POINT ( 'NONE',  ( 77.22499999726881015, 160.0630714827496206, -15.58253175000000823 ) ) ;
#7964 = CARTESIAN_POINT ( 'NONE',  ( 95.59906517536109050, 155.0000000000000000, -31.00000000000000000 ) ) ;
#7965 = CARTESIAN_POINT ( 'NONE',  ( -3.750000000000007105, -6.495190528383289141, 0.000000000000000000 ) ) ;
#7966 = UNCERTAINTY_MEASURE_WITH_UNIT (LENGTH_MEASURE( 1.000000000000000082E-05 ), #24310, 'distance_accuracy_value', 'NONE');
#7967 = CARTESIAN_POINT ( 'NONE',  ( 64.22499999726881015, 149.9369285172503510, 15.58253174999999580 ) ) ;
#7968 = CARTESIAN_POINT ( 'NONE',  ( -7.500000000000000000, -1.572902445675612659, -7.069816568113127531 ) ) ;
#7969 = CARTESIAN_POINT ( 'NONE',  ( 10.01549611932659545, 203.7984951890123853, 52.14886208192142192 ) ) ;
#7970 = AXIS2_PLACEMENT_3D ( 'NONE', #27319, #19826, #3814 ) ;
#7971 = VERTEX_POINT ( 'NONE', #3610 ) ;
#7972 = DIRECTION ( 'NONE',  ( -1.000000000000000000, 0.000000000000000000, 0.000000000000000000 ) ) ;
#7973 = CLOSED_SHELL ( 'NONE', ( #3484, #25957, #2672, #18424, #3265, #6612, #28681, #17173, #8373, #10222, #435, #2538, #15019, #23489, #10262, #33684, #3305, #3700, #6129, #27391, #14810, #23421, #2254, #22405, #28711, #1208, #29491, #27695, #26811, #2909, #30948, #9322 ) ) ;
#7974 = SURFACE_SIDE_STYLE ('',( #16117 ) ) ;
#7975 = DIRECTION ( 'NONE',  ( -1.000000000000000000, 0.000000000000000000, 0.000000000000000000 ) ) ;
#7976 = CARTESIAN_POINT ( 'NONE',  ( 8.000000000000008882, 207.0476921513415220, 33.99886208192143755 ) ) ;
#7977 = CARTESIAN_POINT ( 'NONE',  ( -6.220909254589537696, 198.5229672870051161, 84.05113791807855250 ) ) ;
#7978 = CARTESIAN_POINT ( 'NONE',  ( 63.58867513459481557, 163.8167787843871110, 12.13525491562421621 ) ) ;
#7979 = CARTESIAN_POINT ( 'NONE',  ( -6.139770520408369237, 215.5359834540460042, 51.95113791807857950 ) ) ;
#7980 = VECTOR ( 'NONE', #22285, 1000.000000000000000 ) ;
#7981 = CARTESIAN_POINT ( 'NONE',  ( 9.984503880673470277, 203.7031108863295401, 29.15113791807856103 ) ) ;
#7982 = CARTESIAN_POINT ( 'NONE',  ( 8.015496119326531499, 209.5516654185219636, 13.85113791807856742 ) ) ;
#7983 = DIRECTION ( 'NONE',  ( -1.000000000000000000, 0.000000000000000000, -0.000000000000000000 ) ) ;
#7984 = CARTESIAN_POINT ( 'NONE',  ( -6.830473686658677934E-14, -4.041451884327390331, -0.3126073911696551910 ) ) ;
#7985 = CARTESIAN_POINT ( 'NONE',  ( 35.32499999726881157, 164.1591823560292198, -12.60653300113719766 ) ) ;
#7986 = CARTESIAN_POINT ( 'NONE',  ( 3.753561863808689836, 218.3979405102790565, 43.40113791807856813 ) ) ;
#7987 = CARTESIAN_POINT ( 'NONE',  ( 112.4999999999999858, 155.0000000000000000, -50.00000000000000711 ) ) ;
#7988 = CARTESIAN_POINT ( 'NONE',  ( -6.139770520408369237, 215.5359834540460042, 87.95113791807858661 ) ) ;
#7989 = CARTESIAN_POINT ( 'NONE',  ( -8.118202686958039038, 201.1607312380087080, 57.20113791807857950 ) ) ;
#7990 = CARTESIAN_POINT ( 'NONE',  ( 7.375838497908012492, 217.2372850707501186, 24.54886208192144181 ) ) ;
#7991 = CARTESIAN_POINT ( 'NONE',  ( 8.062137200540822946, 212.9164362838583315, 27.69886208192143684 ) ) ;
#7992 = CARTESIAN_POINT ( 'NONE',  ( 81.39999999453763735, 141.2096805137202580, 4.480746418436733158 ) ) ;
#7993 = CARTESIAN_POINT ( 'NONE',  ( 12.00000000000000711, 206.9523078486586485, 65.00113791807856956 ) ) ;
#7994 = CARTESIAN_POINT ( 'NONE',  ( 4.984841277089725686, 213.7757310962907411, 88.55113791807858092 ) ) ;
#7995 = CARTESIAN_POINT ( 'NONE',  ( 10.01549611932659545, 203.7984951890123853, 49.14886208192143613 ) ) ;
#7996 = AXIS2_PLACEMENT_3D ( 'NONE', #27970, #25585, #15527 ) ;
#7997 = LINE ( 'NONE', #13756, #10185 ) ;
#7998 = EDGE_CURVE ( 'NONE', #860, #29176, #10858, .T. ) ;
#7999 = ORIENTED_EDGE ( 'NONE', *, *, #20345, .T. ) ;
#8000 = CARTESIAN_POINT ( 'NONE',  ( -7.375838497908014268, 196.7627149292498530, 56.04886208192144181 ) ) ;
#8001 = COLOUR_RGB ( '', 0.09019608, 0.27058824, 0.51372549) ;
#8002 = ORIENTED_EDGE ( 'NONE', *, *, #25487, .T. ) ;
#8003 = ORIENTED_EDGE ( 'NONE', *, *, #12373, .T. ) ;
#8004 = CIRCLE ( 'NONE', #12346, 12.99999999999998401 ) ;
#8005 = CARTESIAN_POINT ( 'NONE',  ( 51.48867513459483547, 167.7597621252805880, 9.270509831248428867 ) ) ;
#8006 = DIRECTION ( 'NONE',  ( 1.000000000000000000, 0.000000000000000000, 0.000000000000000000 ) ) ;
#8007 = CARTESIAN_POINT ( 'NONE',  ( 8.015496119326531499, 209.5516654185219636, 40.85113791807856387 ) ) ;
#8008 = CARTESIAN_POINT ( 'NONE',  ( -58.50000000000002132, 194.9217985566782829, 2.500000000000000000 ) ) ;
#8009 = CARTESIAN_POINT ( 'NONE',  ( 0.05014649552828275708, 196.4853777576173002, 25.74886208192143400 ) ) ;
#8010 = CARTESIAN_POINT ( 'NONE',  ( 61.87499999726880162, 171.3844434931184253, -7.942151717890134290E-15 ) ) ;
#8011 = ORIENTED_EDGE ( 'NONE', *, *, #10969, .T. ) ;
#8012 = DIRECTION ( 'NONE',  ( -0.8309481877611850642, 0.02653351925882575443, 0.5557167278498498231 ) ) ;
#8013 = DIRECTION ( 'NONE',  ( -0.000000000000000000, -0.000000000000000000, 1.000000000000000000 ) ) ;
#8014 = CARTESIAN_POINT ( 'NONE',  ( 2.426778023690075337, 214.6231898156240447, 9.398862081921436129 ) ) ;
#8015 = CIRCLE ( 'NONE', #25955, 32.10452846326769816 ) ;
#8016 = CARTESIAN_POINT ( 'NONE',  ( -10.00000000000000711, 207.0476921513413515, 45.50113791807857666 ) ) ;
#8017 = CARTESIAN_POINT ( 'NONE',  ( 6.220909254589536808, 215.4770327129947702, 31.55113791807857382 ) ) ;
#8018 = DIRECTION ( 'NONE',  ( -0.000000000000000000, -0.000000000000000000, 1.000000000000000000 ) ) ;
#8019 = VECTOR ( 'NONE', #20260, 1000.000000000000000 ) ;
#8020 =( NAMED_UNIT ( * ) SI_UNIT ( $, .STERADIAN. ) SOLID_ANGLE_UNIT ( ) );
#8021 = AXIS2_PLACEMENT_3D ( 'NONE', #4259, #30497, #14317 ) ;
#8022 = CARTESIAN_POINT ( 'NONE',  ( -8.000000000000008882, 206.9523078486584780, 95.49886208192144466 ) ) ;
#8023 = CARTESIAN_POINT ( 'NONE',  ( 38.82499999726881157, 141.7447067706911810, -9.630534252274385310 ) ) ;
#8024 = CARTESIAN_POINT ( 'NONE',  ( -57.84141927132884575, 194.9260988872778171, 2.433575273292319707 ) ) ;
#8025 = DIRECTION ( 'NONE',  ( 0.000000000000000000, 0.000000000000000000, -1.000000000000000000 ) ) ;
#8026 = CARTESIAN_POINT ( 'NONE',  ( -9.680171189290831535, 214.0920067884431148, 6.801137918078565825 ) ) ;
#8027 = CARTESIAN_POINT ( 'NONE',  ( 83.71132485994282035, 155.0000000000000000, -15.00000000000002487 ) ) ;
#8028 = CARTESIAN_POINT ( 'NONE',  ( 59.97499999726881015, 169.8198683612136222, 4.815267126137181997 ) ) ;
#8029 = CARTESIAN_POINT ( 'NONE',  ( -3.135527875058821579, 197.5041725223112223, 59.90113791807856813 ) ) ;
#8030 = CARTESIAN_POINT ( 'NONE',  ( 8.062137200540920645, 201.0835637161417822, 29.30113791807857027 ) ) ;
#8031 = AXIS2_PLACEMENT_3D ( 'NONE', #19112, #11123, #29848 ) ;
#8032 = CARTESIAN_POINT ( 'NONE',  ( 127.5000000000000000, 157.1499999999996362, -106.0000000000000284 ) ) ;
#8033 = CARTESIAN_POINT ( 'NONE',  ( -13.75000000000001954, 23.81569860407205752, -18.00000000000000000 ) ) ;
#8034 = CARTESIAN_POINT ( 'NONE',  ( 65.31132485994281467, 140.7341522555726669, -4.635254915624220651 ) ) ;
#8035 = CARTESIAN_POINT ( 'NONE',  ( 60.29999999453761461, 167.3344367211045096, -8.961492836873482304 ) ) ;
#8036 = ORIENTED_EDGE ( 'NONE', *, *, #9090, .T. ) ;
#8037 = CARTESIAN_POINT ( 'NONE',  ( -12.00000000000000711, 207.0476921513413515, 42.50113791807856245 ) ) ;
#8038 = CARTESIAN_POINT ( 'NONE',  ( 76.71132485994280614, 155.0000000000000000, 15.00000000000001243 ) ) ;
#8039 = CARTESIAN_POINT ( 'NONE',  ( -8.118202686958138514, 212.8392687619910930, 20.79886208192143471 ) ) ;
#8040 = CARTESIAN_POINT ( 'NONE',  ( 71.78867513459482552, 155.0000000000000000, 15.00000000000001243 ) ) ;
#8041 = ORIENTED_EDGE ( 'NONE', *, *, #2430, .F. ) ;
#8042 = CARTESIAN_POINT ( 'NONE',  ( 10.00000000000000711, 206.9523078486586201, 68.00113791807856956 ) ) ;
#8043 = AXIS2_PLACEMENT_3D ( 'NONE', #5274, #31021, #13114 ) ;
#8044 = VERTEX_POINT ( 'NONE', #11957 ) ;
#8045 = ADVANCED_FACE ( 'NONE', ( #1563, #32393 ), #17230, .T. ) ;
#8046 = CIRCLE ( 'NONE', #30327, 2.149999999999985256 ) ;
#8047 = CARTESIAN_POINT ( 'NONE',  ( -4.336808689942017736E-14, -31.75426480542944319, -15.54379906938135214 ) ) ;
#8048 = CIRCLE ( 'NONE', #12361, 4.400000000000001243 ) ;
#8049 = CARTESIAN_POINT ( 'NONE',  ( 107.5000000000000000, 155.0000000000000000, -6.938893903907228378E-15 ) ) ;
#8050 = ORIENTED_EDGE ( 'NONE', *, *, #27650, .T. ) ;
#8051 = CARTESIAN_POINT ( 'NONE',  ( 4.903702542908601636, 200.1653181626581102, 17.45113791807856174 ) ) ;
#8052 = CARTESIAN_POINT ( 'NONE',  ( 12.00000000000000711, 207.0476921513415220, 99.99886208192143044 ) ) ;
#8053 = CARTESIAN_POINT ( 'NONE',  ( 41.37499999726880873, 155.0000000000000000, -15.58253175000000823 ) ) ;
#8055 = VERTEX_POINT ( 'NONE', #32727 ) ;
#8054 = CIRCLE ( 'NONE', #1493, 32.00000000000000000 ) ;
#8056 = CARTESIAN_POINT ( 'NONE',  ( 53.42499999726879878, 168.2552932293087906, -9.630534252274385310 ) ) ;
#8057 = CARTESIAN_POINT ( 'NONE',  ( 7.500000000000002665, 3.988838049906435312, -0.8529248949437669980 ) ) ;
#8058 = CARTESIAN_POINT ( 'NONE',  ( -3.044812012440131443, 216.5253028482142952, 10.10113791807856565 ) ) ;
#8059 = CARTESIAN_POINT ( 'NONE',  ( 3.044812012439969795, 216.5253028482143520, 81.39886208192145034 ) ) ;
#8060 = CARTESIAN_POINT ( 'NONE',  ( 50.87499999726881583, 138.6155565068815463, -3.929120461958505118E-15 ) ) ;
#8061 = DIRECTION ( 'NONE',  ( 0.000000000000000000, 0.000000000000000000, -1.000000000000000000 ) ) ;
#8062 = CARTESIAN_POINT ( 'NONE',  ( -6.220909254589537696, 198.5229672870051161, 12.05113791807856671 ) ) ;
#8063 = DIRECTION ( 'NONE',  ( -1.000000000000000000, 0.000000000000000000, 0.000000000000000000 ) ) ;
#8064 = CARTESIAN_POINT ( 'NONE',  ( 67.59999999999998010, 150.2886644046228639, 14.49999999999999645 ) ) ;
#8065 = LINE ( 'NONE', #21323, #25780 ) ;
#8066 = LINE ( 'NONE', #20675, #13150 ) ;
#8067 = CARTESIAN_POINT ( 'NONE',  ( -3.044812012440131443, 216.5253028482142952, 85.10113791807857808 ) ) ;
#8068 = AXIS2_PLACEMENT_3D ( 'NONE', #7136, #29801, #25182 ) ;
#8069 = CARTESIAN_POINT ( 'NONE',  ( 86.08867513459483689, 142.2402378747194405, 9.270509831248432420 ) ) ;
#8070 = CARTESIAN_POINT ( 'NONE',  ( 35.97499999726881015, 169.8198683612136222, 4.815267126137181997 ) ) ;
#8071 = CARTESIAN_POINT ( 'NONE',  ( -9.736236675708031640, 214.0148392665760753, 92.79886208192142760 ) ) ;
#8072 = CIRCLE ( 'NONE', #18920, 32.10452846326769816 ) ;
#8073 = CARTESIAN_POINT ( 'NONE',  ( 69.72499999726881015, 169.8198683612136222, 4.815267126137181997 ) ) ;
#8074 = ORIENTED_EDGE ( 'NONE', *, *, #28746, .T. ) ;
#8075 = CARTESIAN_POINT ( 'NONE',  ( 48.01132485994280330, 167.7597621252805880, -9.270509831248443078 ) ) ;
#8076 = CARTESIAN_POINT ( 'NONE',  ( 38.19999999453763451, 163.5228861582408797, -11.73074641843674470 ) ) ;
#8077 = CARTESIAN_POINT ( 'NONE',  ( 7.456977232089471386, 196.8216656703012006, 4.448862081921434175 ) ) ;
#8078 = EDGE_CURVE ( 'NONE', #18459, #25811, #1360, .T. ) ;
#8079 = DIRECTION ( 'NONE',  ( 1.000000000000000000, -0.000000000000000000, -0.000000000000000000 ) ) ;
#8080 = AXIS2_PLACEMENT_3D ( 'NONE', #5990, #24222, #19281 ) ;
#8081 = ORIENTED_EDGE ( 'NONE', *, *, #28510, .F. ) ;
#8082 = CARTESIAN_POINT ( 'NONE',  ( -9.984503880673420539, 203.7031108863293980, 98.34886208192143897 ) ) ;
#8083 = CARTESIAN_POINT ( 'NONE',  ( 9.736236675708031640, 199.9851607334238963, 22.29886208192143826 ) ) ;
#8084 = CARTESIAN_POINT ( 'NONE',  ( 0.000000000000000000, -1.773042676681340524, 1.734723475976807094E-15 ) ) ;
#8085 = CARTESIAN_POINT ( 'NONE',  ( 8.118202686958039038, 212.8392687619912635, 37.70113791807857240 ) ) ;
#8086 = VERTEX_POINT ( 'NONE', #4451 ) ;
#8087 = CARTESIAN_POINT ( 'NONE',  ( -2.426778023690076225, 199.3768101843759553, 1.898862081921434797 ) ) ;
#8088 = EDGE_CURVE ( 'NONE', #10405, #5632, #4110, .T. ) ;
#8089 = CARTESIAN_POINT ( 'NONE',  ( 5.000000000000000000, 0.000000000000000000, 0.000000000000000000 ) ) ;
#8090 = ORIENTED_EDGE ( 'NONE', *, *, #11237, .T. ) ;
#8091 = CARTESIAN_POINT ( 'NONE',  ( 0.05014649552828262524, 198.5883022060938572, 85.74886208192143044 ) ) ;
#8092 = B_SPLINE_CURVE_WITH_KNOTS ( 'NONE', 3,
 ( #3876, #16825, #32832, #1496, #11890, #12395 ),
 .UNSPECIFIED., .F., .F.,
 ( 4, 2, 4 ),
 ( -6.326732604037524437E-06, 0.0006895418312384076452, 0.001385410395080852695 ),
 .UNSPECIFIED. ) ;
#8093 = AXIS2_PLACEMENT_3D ( 'NONE', #4131, #16743, #24420 ) ;
#8094 = CARTESIAN_POINT ( 'NONE',  ( -4.903702542908602524, 213.8346818373418898, 27.95113791807857240 ) ) ;
#8095 = CARTESIAN_POINT ( 'NONE',  ( 0.000000000000000000, 0.000000000000000000, -18.00000000000000000 ) ) ;
#8096 = ORIENTED_EDGE ( 'NONE', *, *, #2094, .T. ) ;
#8097 = CARTESIAN_POINT ( 'NONE',  ( 127.5000000000000000, 261.0000000000000000, 2.149999999999985256 ) ) ;
#8098 = ADVANCED_FACE ( 'NONE', ( #29854 ), #23906, .F. ) ;
#8099 = CARTESIAN_POINT ( 'NONE',  ( 86.42499999726881299, 141.7447067706911810, 9.630534252274376428 ) ) ;
#8100 = DIRECTION ( 'NONE',  ( -1.000000000000000000, -0.000000000000000000, -0.000000000000000000 ) ) ;
#8101 = CARTESIAN_POINT ( 'NONE',  ( -0.05014649552807731031, 198.5883022060938572, 92.75113791807858377 ) ) ;
#8102 = CONICAL_SURFACE ( 'NONE', #20049, 3.499999999999999556, 1.047197551196589638 ) ;
#8103 = SURFACE_STYLE_USAGE ( .BOTH. , #10823 ) ;
#8104 = CARTESIAN_POINT ( 'NONE',  ( 50.70000000000000284, 163.5228861582408797, -11.73074641843674470 ) ) ;
#8105 = CARTESIAN_POINT ( 'NONE',  ( -0.05014649552828365914, 215.4116977939061144, 60.24886208192144466 ) ) ;
#8106 = CARTESIAN_POINT ( 'NONE',  ( 92.60756280994512224, 155.0000000000000000, -12.10452846326762177 ) ) ;
#8107 = ADVANCED_FACE ( 'NONE', ( #16891 ), #14175, .F. ) ;
#8108 = CARTESIAN_POINT ( 'NONE',  ( 49.52499999726880731, 169.8198683612136222, -4.815267126137197984 ) ) ;
#8110 = ORIENTED_EDGE ( 'NONE', *, *, #24556, .F. ) ;
#8109 = CARTESIAN_POINT ( 'NONE',  ( -3.044812012440131443, 216.5253028482142952, 1.101137918078565869 ) ) ;
#8111 = DIRECTION ( 'NONE',  ( 1.000000000000000000, 0.000000000000000000, 0.000000000000000000 ) ) ;
#8112 = CARTESIAN_POINT ( 'NONE',  ( 66.62499999726881583, 138.6155565068815747, -3.929120461958505118E-15 ) ) ;
#8113 = CARTESIAN_POINT ( 'NONE',  ( 69.57499999726881867, 164.1591823560292198, -12.60653300113719766 ) ) ;
#8114 = CARTESIAN_POINT ( 'NONE',  ( 12.00000000000000711, 206.9523078486586485, 71.00113791807856956 ) ) ;
#8115 = CARTESIAN_POINT ( 'NONE',  ( 49.41132485994282320, 142.2402378747194405, -9.270509831248439525 ) ) ;
#8116 = AXIS2_PLACEMENT_3D ( 'NONE', #16259, #23931, #13692 ) ;
#8117 = CARTESIAN_POINT ( 'NONE',  ( -3.044812012440131443, 216.5253028482142952, 88.10113791807857808 ) ) ;
#8118 = CARTESIAN_POINT ( 'NONE',  ( 84.88867513459487668, 159.8737954434937478, -14.99999999999992362 ) ) ;
#8119 = AXIS2_PLACEMENT_3D ( 'NONE', #14659, #17386, #25559 ) ;
#8120 = CARTESIAN_POINT ( 'NONE',  ( -9.680171189290716072, 199.9079932115567146, 53.19886208192144039 ) ) ;
#8121 = CARTESIAN_POINT ( 'NONE',  ( 10.00000000000000711, 207.0476921513415220, 69.99886208192143044 ) ) ;
#8122 = CARTESIAN_POINT ( 'NONE',  ( -0.05014649552807705357, 194.3824533091408000, 92.75113791807858377 ) ) ;
#8123 = CARTESIAN_POINT ( 'NONE',  ( -6.500000000000000000, 3.752776749732564809, -8.000000000000000000 ) ) ;
#8124 = CARTESIAN_POINT ( 'NONE',  ( -10.00000000000000711, 207.0476921513413515, 9.501137918078566003 ) ) ;
#8125 = CARTESIAN_POINT ( 'NONE',  ( 6.139770520408223575, 215.5359834540460611, 78.54886208192144181 ) ) ;
#8126 = CIRCLE ( 'NONE', #24428, 2.500000000000000000 ) ;
#8127 = EDGE_LOOP ( 'NONE', ( #7338, #30034, #21469, #31896 ) ) ;
#8128 = CARTESIAN_POINT ( 'NONE',  ( 6.220909254589536808, 215.4770327129947702, 97.55113791807855250 ) ) ;
#8129 = ORIENTED_EDGE ( 'NONE', *, *, #4121, .F. ) ;
#8130 = CARTESIAN_POINT ( 'NONE',  ( 2.047034997319582939, 2.859595677584332307, 1.982057096575062005E-15 ) ) ;
#8131 = CARTESIAN_POINT ( 'NONE',  ( -2.517493886309087880, 214.5937144450984135, 63.09886208192143187 ) ) ;
#8132 = VERTEX_POINT ( 'NONE', #22010 ) ;
#8133 = CARTESIAN_POINT ( 'NONE',  ( 77.82499999726880446, 168.2552932293087906, 9.630534252274372875 ) ) ;
#8134 = CARTESIAN_POINT ( 'NONE',  ( -16.00000000000000000, 1.959434878635765131E-15, -1.400415076419418092 ) ) ;
#8135 = CARTESIAN_POINT ( 'NONE',  ( 15.61000000000001364, 0.000000000000000000, 0.000000000000000000 ) ) ;
#8136 = AXIS2_PLACEMENT_3D ( 'NONE', #5827, #890, #11287 ) ;
#8137 = CARTESIAN_POINT ( 'NONE',  ( 71.52499999726882152, 169.8198683612136222, -4.815267126137197984 ) ) ;
#8138 = CARTESIAN_POINT ( 'NONE',  ( -0.05014649552807731031, 198.5883022060938572, 62.75113791807856245 ) ) ;
#8139 = EDGE_CURVE ( 'NONE', #9805, #18384, #28167, .T. ) ;
#8140 = CARTESIAN_POINT ( 'NONE',  ( 117.5000000000000000, 63.20130719884917170, -52.99999999999946709 ) ) ;
#8141 = ADVANCED_FACE ( 'NONE', ( #25238 ), #1605, .F. ) ;
#8142 = CARTESIAN_POINT ( 'NONE',  ( 115.4999999999999858, 155.0000000000000000, -100.0000000000000000 ) ) ;
#8143 = CARTESIAN_POINT ( 'NONE',  ( -47.49999999999998579, 155.0000000000000000, -6.938893903907228378E-15 ) ) ;
#8144 = CARTESIAN_POINT ( 'NONE',  ( 4.903702542908435547, 213.8346818373419751, 33.54886208192144181 ) ) ;
#8145 = CARTESIAN_POINT ( 'NONE',  ( -6.139770520408369237, 215.5359834540460042, 78.95113791807858661 ) ) ;
#8146 = PLANE ( 'NONE',  #24550 ) ;
#8147 = EDGE_CURVE ( 'NONE', #33389, #21429, #1225, .T. ) ;
#8148 = CARTESIAN_POINT ( 'NONE',  ( 8.118202686958039038, 212.8392687619912635, 55.70113791807857950 ) ) ;
#8149 = CARTESIAN_POINT ( 'NONE',  ( -0.05014649552810635652, 196.4853777576173002, 23.75113791807855890 ) ) ;
#8150 = CARTESIAN_POINT ( 'NONE',  ( 8.000000000000008882, 206.9523078486586485, 17.00113791807856956 ) ) ;
#8151 = CARTESIAN_POINT ( 'NONE',  ( 121.7736297201317370, -4.198250922590419876, 35.00001200000000523 ) ) ;
#8152 = CARTESIAN_POINT ( 'NONE',  ( 6.500000000000002665, 2.501851166488374911, -5.848636054922036642 ) ) ;
#8153 = CARTESIAN_POINT ( 'NONE',  ( 44.82499999726880446, 141.7447067706911810, -9.630534252274387086 ) ) ;
#8154 = CARTESIAN_POINT ( 'NONE',  ( -3.662846001190052991, 218.4274158808045740, 37.10113791807855677 ) ) ;
#8155 = FACE_OUTER_BOUND ( 'NONE', #26546, .T. ) ;
#8156 = ADVANCED_FACE ( 'NONE', ( #22171 ), #21834, .F. ) ;
#8157 = CARTESIAN_POINT ( 'NONE',  ( -9.984503880673473830, 210.2968891136704315, 84.65113791807857524 ) ) ;
#8158 = CARTESIAN_POINT ( 'NONE',  ( -6.139770520408368348, 215.5359834540460042, 60.95113791807857240 ) ) ;
#8159 = CARTESIAN_POINT ( 'NONE',  ( -3.662846001189865142, 195.5725841191952838, 25.89886208192143613 ) ) ;
#8160 = CARTESIAN_POINT ( 'NONE',  ( -8.118202686958138514, 212.8392687619910930, 26.79886208192143826 ) ) ;
#8161 = CARTESIAN_POINT ( 'NONE',  ( 76.89999999453763735, 159.7113355953771077, 14.49999999999999289 ) ) ;
#8162 = CARTESIAN_POINT ( 'NONE',  ( -3.753561863808691168, 195.6020594897209435, 65.90113791807856103 ) ) ;
#8163 = AXIS2_PLACEMENT_3D ( 'NONE', #19746, #27412, #3569 ) ;
#8164 = CARTESIAN_POINT ( 'NONE',  ( -2.517493886308901807, 199.4062855549015012, 92.90113791807857524 ) ) ;
#8165 = CARTESIAN_POINT ( 'NONE',  ( -0.05014649552828403384, 217.5146222423826714, 48.24886208192142334 ) ) ;
#8166 = DIRECTION ( 'NONE',  ( 0.000000000000000000, 0.000000000000000000, 1.000000000000000000 ) ) ;
#8167 = ORIENTED_EDGE ( 'NONE', *, *, #16367, .F. ) ;
#8168 = CARTESIAN_POINT ( 'NONE',  ( 9.736236675708031640, 199.9851607334238963, 49.29886208192143471 ) ) ;
#8169 = VERTEX_POINT ( 'NONE', #9396 ) ;
#8170 = ORIENTED_EDGE ( 'NONE', *, *, #28609, .F. ) ;
#8171 = CARTESIAN_POINT ( 'NONE',  ( 78.17499999726881299, 164.1591823560292198, 12.60653300113718167 ) ) ;
#8172 = DIRECTION ( 'NONE',  ( 0.000000000000000000, 0.000000000000000000, -1.000000000000000000 ) ) ;
#8173 = CARTESIAN_POINT ( 'NONE',  ( 47.78867513459482552, 155.0000000000000000, 15.00000000000001243 ) ) ;
#8174 = CARTESIAN_POINT ( 'NONE',  ( -6.444103211791042618, 211.7408657792732356, 42.80113791807857382 ) ) ;
#8175 = CARTESIAN_POINT ( 'NONE',  ( 7.922281120364393914, 4.573931137438269623, -8.047472243342930653 ) ) ;
#8176 = CARTESIAN_POINT ( 'NONE',  ( -3.135527875058982783, 216.4958274776886924, 21.09886208192143897 ) ) ;
#8177 = CARTESIAN_POINT ( 'NONE',  ( 65.47499999726881015, 160.0630714827496206, -15.58253175000000823 ) ) ;
#8178 = EDGE_LOOP ( 'NONE', ( #1837, #29659, #17373, #33643 ) ) ;
#8179 = CARTESIAN_POINT ( 'NONE',  ( 62.68867513459484542, 150.1262045565065364, -15.00000000000012434 ) ) ;
#8180 = SURFACE_SIDE_STYLE ('',( #832 ) ) ;
#8181 = CARTESIAN_POINT ( 'NONE',  ( 115.4999999999999858, 257.3881375866408803, -27.43481878086871717 ) ) ;
#8182 = CARTESIAN_POINT ( 'NONE',  ( 8.000000000000008882, 207.0476921513415220, 3.998862081921434442 ) ) ;
#8183 = CARTESIAN_POINT ( 'NONE',  ( 3.135527875058820690, 216.4958274776887492, 52.40113791807857524 ) ) ;
#8184 = FACE_OUTER_BOUND ( 'NONE', #1738, .T. ) ;
#8185 = PRODUCT_DEFINITION_SHAPE ( 'NONE', 'NONE',  #33712 ) ;
#8186 = CARTESIAN_POINT ( 'NONE',  ( -6.220909254589537696, 198.5229672870051161, 27.05113791807856671 ) ) ;
#8187 = CARTESIAN_POINT ( 'NONE',  ( 86.37499999726881583, 155.0000000000000000, 15.58253174999999402 ) ) ;
#8188 = APPLICATION_PROTOCOL_DEFINITION ( 'draft international standard', 'automotive_design', 1998, #7246 ) ;
#8189 = CARTESIAN_POINT ( 'NONE',  ( -8.000000000000008882, 206.9523078486584780, 89.49886208192144466 ) ) ;
#8190 = CARTESIAN_POINT ( 'NONE',  ( 37.02499999726880020, 149.9369285172503510, -15.58253175000000823 ) ) ;
#8191 = CARTESIAN_POINT ( 'NONE',  ( 35.78867513459482552, 155.0000000000000000, 15.00000000000001243 ) ) ;
#8192 = CARTESIAN_POINT ( 'NONE',  ( 32.50000000000000000, 155.0000000000000000, -6.938893903907228378E-15 ) ) ;
#8193 = CARTESIAN_POINT ( 'NONE',  ( -11.98450388067348804, 210.9467285061362247, 9.651137918078566358 ) ) ;
#8194 = DIRECTION ( 'NONE',  ( 1.000000000000000000, 0.000000000000000000, 0.000000000000000000 ) ) ;
#8195 = CARTESIAN_POINT ( 'NONE',  ( 58.07499999726880446, 168.2552932293087906, 9.630534252274372875 ) ) ;
#8196 = CARTESIAN_POINT ( 'NONE',  ( 0.05014649552810505201, 217.5146222423826714, 52.25113791807856245 ) ) ;
#8197 = CARTESIAN_POINT ( 'NONE',  ( -10.00000000000000711, 207.0476921513413515, 33.50113791807856956 ) ) ;
#8198 = CYLINDRICAL_SURFACE ( 'NONE', #33357, 5.249999999999991118 ) ;
#8199 = CARTESIAN_POINT ( 'NONE',  ( 55.28867513459483973, 170.7719333635740497, -7.904646289410545231E-15 ) ) ;
#8200 = CARTESIAN_POINT ( 'NONE',  ( 0.05014649552828275014, 196.4853777576173002, 1.748862081921434442 ) ) ;
#8201 = CARTESIAN_POINT ( 'NONE',  ( 57.49999999453763166, 139.7537977485451393, -4.138211985947621020E-15 ) ) ;
#8202 = ORIENTED_EDGE ( 'NONE', *, *, #10868, .F. ) ;
#8203 = CARTESIAN_POINT ( 'NONE',  ( 7.456977232089302632, 217.1783343296989131, 43.55113791807857382 ) ) ;
#8204 = CYLINDRICAL_SURFACE ( 'NONE', #24684, 15.00000000000001776 ) ;
#8205 = CARTESIAN_POINT ( 'NONE',  ( 6.139770520408223575, 215.5359834540460611, 24.54886208192143471 ) ) ;
#8206 = CARTESIAN_POINT ( 'NONE',  ( 70.98867513459484258, 163.8167787843871110, -12.13525491562423397 ) ) ;
#8207 = EDGE_LOOP ( 'NONE', ( #18147, #28369, #4988, #23570 ) ) ;
#8208 = CARTESIAN_POINT ( 'NONE',  ( -8.118202686958039038, 201.1607312380087080, 72.20113791807857240 ) ) ;
#8209 = ORIENTED_EDGE ( 'NONE', *, *, #7715, .T. ) ;
#8210 = CYLINDRICAL_SURFACE ( 'NONE', #24907, 5.250000000000004441 ) ;
#8211 = CYLINDRICAL_SURFACE ( 'NONE', #13776, 2.500000000000000000 ) ;
#8212 = ORIENTED_EDGE ( 'NONE', *, *, #16174, .T. ) ;
#8213 = CARTESIAN_POINT ( 'NONE',  ( 2.426778023690261410, 199.3768101843759837, 8.601137918078565647 ) ) ;
#8214 = CARTESIAN_POINT ( 'NONE',  ( 9.736236675708031640, 199.9851607334238963, 94.29886208192142760 ) ) ;
#8215 = CARTESIAN_POINT ( 'NONE',  ( 45.97499999726881015, 169.8198683612136222, 4.815267126137181997 ) ) ;
#8216 = EDGE_LOOP ( 'NONE', ( #3274, #18721, #19449, #27462 ) ) ;
#8217 = CARTESIAN_POINT ( 'NONE',  ( 49.82499999726881157, 168.2552932293087906, 9.630534252274372875 ) ) ;
#8218 = DIRECTION ( 'NONE',  ( -1.000000000000000000, 0.000000000000000000, 0.000000000000000000 ) ) ;
#8219 = CARTESIAN_POINT ( 'NONE',  ( 9.984503880673470277, 203.7031108863295401, 5.151137918078567246 ) ) ;
#8220 = CARTESIAN_POINT ( 'NONE',  ( 8.062137200540822946, 212.9164362838583315, 84.69886208192144750 ) ) ;
#8221 = CARTESIAN_POINT ( 'NONE',  ( 55.17499999726881299, 145.8408176439707802, -12.60653300113719588 ) ) ;
#8222 = CARTESIAN_POINT ( 'NONE',  ( -10.01549611932653860, 203.7984951890123284, 24.35113791807855677 ) ) ;
#8223 = DIRECTION ( 'NONE',  ( 0.000000000000000000, -0.7071067811865506814, -0.7071067811865442421 ) ) ;
#8224 = CARTESIAN_POINT ( 'NONE',  ( 73.00000000000001421, 170.2462022514548323, -7.872454543227099337E-15 ) ) ;
#8225 = CARTESIAN_POINT ( 'NONE',  ( -10.00000000000000711, 207.0476921513413515, 99.50113791807856956 ) ) ;
#8226 = CARTESIAN_POINT ( 'NONE',  ( -27.50000000000000000, -2.682974265912531742, 2.093865445612630438E-15 ) ) ;
#8227 = CARTESIAN_POINT ( 'NONE',  ( -0.05014649552810635652, 196.4853777576173002, 89.75113791807854113 ) ) ;
#8228 = DIRECTION ( 'NONE',  ( 0.000000000000000000, 0.000000000000000000, -1.000000000000000000 ) ) ;
#8229 = CARTESIAN_POINT ( 'NONE',  ( 40.87499999726880873, 138.6155565068815463, -3.929120461958505118E-15 ) ) ;
#8230 = CARTESIAN_POINT ( 'NONE',  ( 12.01549611932659367, 203.1486557965466773, 97.14886208192146455 ) ) ;
#8231 = EDGE_CURVE ( 'NONE', #32863, #13926, #19286, .T. ) ;
#8232 = CARTESIAN_POINT ( 'NONE',  ( 68.72499999726881015, 140.1801316387863778, -4.815267126137194431 ) ) ;
#8233 = VERTEX_POINT ( 'NONE', #19792 ) ;
#8234 = DIRECTION ( 'NONE',  ( 1.000000000000000000, -0.000000000000000000, -0.000000000000000000 ) ) ;
#8235 = CARTESIAN_POINT ( 'NONE',  ( 38.79999999453762882, 163.5228861582408797, 11.73074641843673049 ) ) ;
#8236 = CARTESIAN_POINT ( 'NONE',  ( 89.50000000000002842, 155.0000000000000000, 0.000000000000000000 ) ) ;
#8237 = CARTESIAN_POINT ( 'NONE',  ( 4.999999999999999112, -5.773502691896267081, -7.063244554130005071 ) ) ;
#8238 = ORIENTED_EDGE ( 'NONE', *, *, #28899, .T. ) ;
#8239 = CARTESIAN_POINT ( 'NONE',  ( 0.05014649552828275014, 196.4853777576173002, 97.74886208192141623 ) ) ;
#8240 = AXIS2_PLACEMENT_3D ( 'NONE', #30806, #7468, #17852 ) ;
#8241 = CARTESIAN_POINT ( 'NONE',  ( 11.98450388067341876, 210.9467285061363953, 30.84886208192143542 ) ) ;
#8242 = DIRECTION ( 'NONE',  ( 0.000000000000000000, 0.000000000000000000, -1.000000000000000000 ) ) ;
#8243 = CARTESIAN_POINT ( 'NONE',  ( 9.984503880673470277, 203.7031108863295401, 41.15113791807855392 ) ) ;
#8244 = B_SPLINE_CURVE_WITH_KNOTS ( 'NONE', 3,
 ( #12445, #9376, #22835, #32883, #20274 ),
 .UNSPECIFIED., .F., .F.,
 ( 4, 1, 4 ),
 ( 5.644705275899819452E-20, 0.003752776749732567464, 0.007505553499465136662 ),
 .UNSPECIFIED. ) ;
#8245 = VERTEX_POINT ( 'NONE', #30186 ) ;
#8246 = CARTESIAN_POINT ( 'NONE',  ( -10.05084501415679732, 217.6133941545940047, 104.9910338291041683 ) ) ;
#8247 = DIRECTION ( 'NONE',  ( 1.000000000000000000, 0.000000000000000000, 0.000000000000000000 ) ) ;
#8248 = ORIENTED_EDGE ( 'NONE', *, *, #16047, .F. ) ;
#8249 = CARTESIAN_POINT ( 'NONE',  ( 6.500168698208244500, 202.3363017425938324, 91.29886208192142760 ) ) ;
#8250 = CARTESIAN_POINT ( 'NONE',  ( 2.517493886308900919, 214.5937144450984420, 31.40113791807857879 ) ) ;
#8251 = DIRECTION ( 'NONE',  ( -0.000000000000000000, -0.000000000000000000, 1.000000000000000000 ) ) ;
#8252 = VERTEX_POINT ( 'NONE', #30014 ) ;
#8253 = CARTESIAN_POINT ( 'NONE',  ( 33.32499999726881157, 164.1591823560292198, -12.60653300113719766 ) ) ;
#8254 = CARTESIAN_POINT ( 'NONE',  ( 87.72499999726882436, 169.8198683612136222, 4.815267126137181997 ) ) ;
#8255 = CARTESIAN_POINT ( 'NONE',  ( 16.00000000000000000, 1.610000000000000098, 0.000000000000000000 ) ) ;
#8256 = CARTESIAN_POINT ( 'NONE',  ( -4.903702542908602524, 213.8346818373418898, 84.95113791807858661 ) ) ;
#8257 = AXIS2_PLACEMENT_3D ( 'NONE', #19279, #32895, #4103 ) ;
#8258 = DIRECTION ( 'NONE',  ( 1.000000000000000000, 0.000000000000000000, 0.000000000000000000 ) ) ;
#8259 = CARTESIAN_POINT ( 'NONE',  ( 54.10000000000000142, 141.2096805137202580, -4.480746418436742040 ) ) ;
#8260 = CARTESIAN_POINT ( 'NONE',  ( 4.984841277089891776, 200.2242689037093726, 70.44886208192144750 ) ) ;
#8261 = CARTESIAN_POINT ( 'NONE',  ( 84.51132485994280330, 163.8167787843871110, 12.13525491562421621 ) ) ;
#8262 = EDGE_CURVE ( 'NONE', #26876, #23763, #32903, .T. ) ;
#8263 = CARTESIAN_POINT ( 'NONE',  ( 50.82499999726880446, 141.7447067706911810, -9.630534252274385310 ) ) ;
#8265 = VERTEX_POINT ( 'NONE', #12123 ) ;
#8264 = CARTESIAN_POINT ( 'NONE',  ( 8.118202686958039038, 212.8392687619912635, 13.70113791807856707 ) ) ;
#8266 = DIRECTION ( 'NONE',  ( -0.000000000000000000, -0.000000000000000000, -1.000000000000000000 ) ) ;
#8267 = AXIS2_PLACEMENT_3D ( 'NONE', #32413, #9080, #27309 ) ;
#8268 = CARTESIAN_POINT ( 'NONE',  ( 61.42499999726882010, 168.2552932293087906, -9.630534252274387086 ) ) ;
#8269 = CARTESIAN_POINT ( 'NONE',  ( 78.77499999726880731, 140.1801316387863778, 4.815267126137185549 ) ) ;
#8270 = CARTESIAN_POINT ( 'NONE',  ( -11.98450388067348804, 210.9467285061362247, 78.65113791807858945 ) ) ;
#8271 = DIRECTION ( 'NONE',  ( -0.000000000000000000, -0.000000000000000000, 1.000000000000000000 ) ) ;
#8272 = EDGE_CURVE ( 'NONE', #33266, #12632, #22284, .T. ) ;
#8273 = CARTESIAN_POINT ( 'NONE',  ( -3.135527875058821579, 197.5041725223112223, 95.90113791807858945 ) ) ;
#8274 = CARTESIAN_POINT ( 'NONE',  ( -10.17386985161379620, 208.0352956435529563, 102.7846294209004441 ) ) ;
#8275 = EDGE_CURVE ( 'NONE', #16362, #546, #17569, .T. ) ;
#8276 = VERTEX_POINT ( 'NONE', #28478 ) ;
#8277 = CARTESIAN_POINT ( 'NONE',  ( -0.05014649552828442242, 219.6175466908591716, 63.24886208192142334 ) ) ;
#8278 = CARTESIAN_POINT ( 'NONE',  ( -8.118202686958138514, 212.8392687619910930, 71.79886208192142760 ) ) ;
#8279 = CARTESIAN_POINT ( 'NONE',  ( -9.680171189290716072, 199.9079932115567146, 5.198862081921434175 ) ) ;
#8280 = FACE_OUTER_BOUND ( 'NONE', #3869, .T. ) ;
#8281 = CARTESIAN_POINT ( 'NONE',  ( 0.05014649552810505201, 217.5146222423826714, 13.25113791807856778 ) ) ;
#8282 = CARTESIAN_POINT ( 'NONE',  ( 10.01549611932659545, 203.7984951890123853, 82.14886208192140771 ) ) ;
#8283 = EDGE_LOOP ( 'NONE', ( #2139, #7290, #365, #32066 ) ) ;
#8284 = FACE_OUTER_BOUND ( 'NONE', #2835, .T. ) ;
#8285 = ORIENTED_EDGE ( 'NONE', *, *, #3345, .T. ) ;
#8286 = DIRECTION ( 'NONE',  ( 0.000000000000000000, 0.000000000000000000, 1.000000000000000000 ) ) ;
#8287 = CARTESIAN_POINT ( 'NONE',  ( -7.984503880673422316, 204.3529502787951628, 59.34886208192144608 ) ) ;
#8288 = EDGE_LOOP ( 'NONE', ( #3326, #25894, #8285, #9877 ) ) ;
#8289 = EDGE_CURVE ( 'NONE', #12471, #31786, #7605, .T. ) ;
#8290 = CARTESIAN_POINT ( 'NONE',  ( 79.92499999726881299, 164.1591823560292198, 12.60653300113718167 ) ) ;
#8291 = CYLINDRICAL_SURFACE ( 'NONE', #29310, 15.00000000000001776 ) ;
#8292 = DIRECTION ( 'NONE',  ( 0.000000000000000000, 0.000000000000000000, -1.000000000000000000 ) ) ;
#8293 = AXIS2_PLACEMENT_3D ( 'NONE', #31550, #11109, #32207 ) ;
#8294 = EDGE_CURVE ( 'NONE', #8132, #2210, #19551, .T. ) ;
#8295 = AXIS2_PLACEMENT_3D ( 'NONE', #9450, #22388, #1612 ) ;
#8296 = CARTESIAN_POINT ( 'NONE',  ( 71.72499999726881015, 169.8198683612136222, 4.815267126137181997 ) ) ;
#8297 = CARTESIAN_POINT ( 'NONE',  ( 4.903702542908601636, 200.1653181626581102, 62.45113791807857240 ) ) ;
#8298 = CARTESIAN_POINT ( 'NONE',  ( 4.200000000000001954, 0.000000000000000000, -2.200000000000001066 ) ) ;
#8299 = DIRECTION ( 'NONE',  ( 1.000000000000000000, -0.000000000000000000, -0.000000000000000000 ) ) ;
#8300 = CARTESIAN_POINT ( 'NONE',  ( -2.426778023690076225, 199.3768101843759553, 37.89886208192144323 ) ) ;
#8301 = CARTESIAN_POINT ( 'NONE',  ( -6.139770520408369237, 215.5359834540460042, 84.95113791807858661 ) ) ;
#8302 = DIRECTION ( 'NONE',  ( -1.000000000000000000, 0.000000000000000000, 0.000000000000000000 ) ) ;
#8303 = CARTESIAN_POINT ( 'NONE',  ( 6.220909254589536808, 215.4770327129947702, 64.55113791807858092 ) ) ;
#8304 = AXIS2_PLACEMENT_3D ( 'NONE', #19613, #4621, #33058 ) ;
#8305 = DIRECTION ( 'NONE',  ( 0.000000000000000000, 0.000000000000000000, 1.000000000000000000 ) ) ;
#8306 = CARTESIAN_POINT ( 'NONE',  ( 7.984503880673485376, 204.3529502787953902, 14.15113791807856991 ) ) ;
#8307 = DIRECTION ( 'NONE',  ( -0.000000000000000000, 0.000000000000000000, -1.000000000000000000 ) ) ;
#8308 = CARTESIAN_POINT ( 'NONE',  ( 4.000000000000000000, 3.518949890710768802, -4.770489558936219510E-15 ) ) ;
#8309 = CARTESIAN_POINT ( 'NONE',  ( 43.32499999726881157, 164.1591823560292198, -12.60653300113719766 ) ) ;
#8310 = CARTESIAN_POINT ( 'NONE',  ( 11.98450388067348271, 203.0532714938637753, 53.15113791807857524 ) ) ;
#8311 = CARTESIAN_POINT ( 'NONE',  ( 7.500000000000000000, -1.645076096015019695, -7.030022527230891605 ) ) ;
#8312 = CARTESIAN_POINT ( 'NONE',  ( 10.01549611932653860, 210.2015048109876716, 94.85113791807857808 ) ) ;
#8313 = CARTESIAN_POINT ( 'NONE',  ( 10.00000000000000711, 206.9523078486586201, 59.00113791807857666 ) ) ;
#8314 = CARTESIAN_POINT ( 'NONE',  ( -12.01549611932659722, 210.8513442034533227, 26.64886208192143968 ) ) ;
#8315 = CARTESIAN_POINT ( 'NONE',  ( 10.01549611932659367, 203.7984951890124421, 37.14886208192142192 ) ) ;
#8316 = CARTESIAN_POINT ( 'NONE',  ( 77.89999999453763735, 150.2886644046228639, -14.50000000000000888 ) ) ;
#8317 = AXIS2_PLACEMENT_3D ( 'NONE', #29351, #13341, #3613 ) ;
#8318 = CARTESIAN_POINT ( 'NONE',  ( 9.736236675707914401, 214.0148392665762458, 67.70113791807857240 ) ) ;
#8319 = CARTESIAN_POINT ( 'NONE',  ( -4.984841277089726574, 200.2242689037092305, 93.05113791807858092 ) ) ;
#8320 = CIRCLE ( 'NONE', #6112, 6.999999999999950262 ) ;
#8321 = ADVANCED_FACE ( 'NONE', ( #18250 ), #7184, .F. ) ;
#8322 = CARTESIAN_POINT ( 'NONE',  ( 6.220909254589681581, 198.5229672870052582, 46.44886208192141908 ) ) ;
#8323 = CARTESIAN_POINT ( 'NONE',  ( 49.38867513459482694, 169.2658477444273331, 4.635254915624208216 ) ) ;
#8324 = VERTEX_POINT ( 'NONE', #2585 ) ;
#8325 = CARTESIAN_POINT ( 'NONE',  ( -7.456977232089471386, 217.1783343296987709, 53.94886208192144039 ) ) ;
#8326 = ORIENTED_EDGE ( 'NONE', *, *, #15823, .F. ) ;
#8327 = VERTEX_POINT ( 'NONE', #33417 ) ;
#8328 = EDGE_CURVE ( 'NONE', #5394, #24271, #13567, .T. ) ;
#8329 = CARTESIAN_POINT ( 'NONE',  ( 74.97499999726881015, 140.1801316387863778, -4.815267126137194431 ) ) ;
#8330 = CARTESIAN_POINT ( 'NONE',  ( 5.000000000000000000, 2.342598717236900718, -4.057500000000001883 ) ) ;
#8331 = CIRCLE ( 'NONE', #27356, 40.00000000000000711 ) ;
#8332 = CARTESIAN_POINT ( 'NONE',  ( 4.102348501002488490, 207.3577873115561943, -8.835681806194324750 ) ) ;
#8333 = CARTESIAN_POINT ( 'NONE',  ( 4.903702542908601636, 200.1653181626581102, 50.45113791807857240 ) ) ;
#8334 = EDGE_CURVE ( 'NONE', #16034, #8252, #23367, .T. ) ;
#8335 = CARTESIAN_POINT ( 'NONE',  ( 4.200000000000001954, 0.000000000000000000, 0.000000000000000000 ) ) ;
#8336 = CARTESIAN_POINT ( 'NONE',  ( -8.062137200540822946, 201.0835637161416400, 35.19886208192143329 ) ) ;
#8337 = CARTESIAN_POINT ( 'NONE',  ( 66.17499999726881299, 164.1591823560292198, 12.60653300113718167 ) ) ;
#8338 = EDGE_LOOP ( 'NONE', ( #19377, #29267 ) ) ;
#8339 = CARTESIAN_POINT ( 'NONE',  ( 42.50000000000000000, -103.0000000000000142, -51.04834939252008041 ) ) ;
#8340 = CIRCLE ( 'NONE', #11066, 5.249999999999997335 ) ;
#8341 = CARTESIAN_POINT ( 'NONE',  ( -7.640563834021360018E-16, -9.147862274876560562, -8.047472243342937759 ) ) ;
#8342 = CARTESIAN_POINT ( 'NONE',  ( -2.426778023690076225, 199.3768101843759553, 7.898862081921436129 ) ) ;
#8343 = AXIS2_PLACEMENT_3D ( 'NONE', #737, #897, #14012 ) ;
#8344 = CARTESIAN_POINT ( 'NONE',  ( 10.01549611932653860, 210.2015048109876716, 52.85113791807854966 ) ) ;
#8345 = CARTESIAN_POINT ( 'NONE',  ( 83.58867513459483689, 163.8167787843871110, 12.13525491562421621 ) ) ;
#8346 = CARTESIAN_POINT ( 'NONE',  ( 10.01549611932653860, 210.2015048109876716, 37.85113791807854966 ) ) ;
#8347 = CARTESIAN_POINT ( 'NONE',  ( 81.67499999726881299, 168.2552932293087906, -9.630534252274385310 ) ) ;
#8348 = AXIS2_PLACEMENT_3D ( 'NONE', #27979, #4646, #15030 ) ;
#8349 = CARTESIAN_POINT ( 'NONE',  ( -7.984503880673422316, 204.3529502787951628, 95.34886208192143897 ) ) ;
#8350 = CARTESIAN_POINT ( 'NONE',  ( 38.02499999726881441, 160.0630714827496206, 15.58253174999999402 ) ) ;
#8351 = FILL_AREA_STYLE ('',( #32175 ) ) ;
#8352 = DIRECTION ( 'NONE',  ( 0.000000000000000000, 0.000000000000000000, -1.000000000000000000 ) ) ;
#8353 = CARTESIAN_POINT ( 'NONE',  ( 9.680171189290831535, 199.9079932115568852, 5.301137918078565825 ) ) ;
#8354 = CARTESIAN_POINT ( 'NONE',  ( 82.38867513459483405, 140.7341522555726669, -4.635254915624220651 ) ) ;
#8355 = CARTESIAN_POINT ( 'NONE',  ( 58.87499999726880162, 138.6155565068815463, -3.929120461958505118E-15 ) ) ;
#8356 = CARTESIAN_POINT ( 'NONE',  ( 9.984503880673470277, 203.7031108863295401, 68.15113791807857524 ) ) ;
#8357 = CARTESIAN_POINT ( 'NONE',  ( 0.05014649552810506589, 217.5146222423826714, 31.25113791807857311 ) ) ;
#8358 = CARTESIAN_POINT ( 'NONE',  ( 2.000000000000000000, 0.000000000000000000, 0.000000000000000000 ) ) ;
#8359 = FACE_OUTER_BOUND ( 'NONE', #12850, .T. ) ;
#8360 = CARTESIAN_POINT ( 'NONE',  ( 8.062137200540822946, 212.9164362838583315, 12.69886208192143506 ) ) ;
#8361 = CARTESIAN_POINT ( 'NONE',  ( 62.79999999453762882, 163.5228861582408797, 11.73074641843673049 ) ) ;
#8362 = ORIENTED_EDGE ( 'NONE', *, *, #5823, .F. ) ;
#8363 = CARTESIAN_POINT ( 'NONE',  ( 9.736236675707914401, 214.0148392665762458, 34.70113791807856529 ) ) ;
#8364 = DIRECTION ( 'NONE',  ( -1.000000000000000000, 0.000000000000000000, -0.000000000000000000 ) ) ;
#8365 = CARTESIAN_POINT ( 'NONE',  ( -9.984503880673420539, 203.7031108863293980, 26.34886208192142831 ) ) ;
#8366 = EDGE_CURVE ( 'NONE', #8954, #31727, #31642, .T. ) ;
#8367 = ORIENTED_EDGE ( 'NONE', *, *, #11235, .F. ) ;
#8368 = CIRCLE ( 'NONE', #21413, 30.00000000000000000 ) ;
#8369 =( BOUNDED_CURVE ( )  B_SPLINE_CURVE ( 2, ( #8822, #5606, #15999, #3720, #21447, #1162, #31829, #21112, #8495, #29282, #5933 ),
 .UNSPECIFIED., .F., .F. ) 
 B_SPLINE_CURVE_WITH_KNOTS ( ( 3, 2, 2, 2, 2, 3 ),
 ( 0.8214285714285713969, 0.8249999999999999556, 0.8285714285714285143, 0.8321428571428570731, 0.8357142857142856318, 0.8392857142857141906 ),
 .UNSPECIFIED. ) 
 CURVE ( )  GEOMETRIC_REPRESENTATION_ITEM ( )  RATIONAL_B_SPLINE_CURVE ( ( 1.000000000000000000, 0.9510565162951534202, 1.000000000000000000, 0.9510565162951534202, 1.000000000000000000, 0.9510565162951534202, 1.000000000000000000, 0.9510565162951534202, 1.000000000000000000, 0.9510565162951534202, 1.000000000000000000 ) ) 
 REPRESENTATION_ITEM ( '' )  );
#8370 = CARTESIAN_POINT ( 'NONE',  ( 6.220909254589536808, 215.4770327129947702, 79.55113791807855250 ) ) ;
#8371 = VECTOR ( 'NONE', #12478, 1000.000000000000000 ) ;
#8372 = ORIENTED_EDGE ( 'NONE', *, *, #2117, .F. ) ;
#8373 = ADVANCED_FACE ( 'NONE', ( #25743 ), #30519, .T. ) ;
#8374 = AXIS2_PLACEMENT_3D ( 'NONE', #16026, #13303, #18756 ) ;
#8375 = DIRECTION ( 'NONE',  ( -0.000000000000000000, -0.000000000000000000, 1.000000000000000000 ) ) ;
#8376 = DIRECTION ( 'NONE',  ( -1.000000000000000000, 0.000000000000000000, 0.000000000000000000 ) ) ;
#8377 = ORIENTED_EDGE ( 'NONE', *, *, #15569, .T. ) ;
#8378 = CARTESIAN_POINT ( 'NONE',  ( 8.015496119326531499, 209.5516654185219636, 10.85113791807856565 ) ) ;
#8379 = CARTESIAN_POINT ( 'NONE',  ( 6.500000000000000000, 3.752776749732563921, -6.064240316920399110 ) ) ;
#8380 = CARTESIAN_POINT ( 'NONE',  ( 3.662846001189864698, 218.4274158808046593, 102.3988620819214361 ) ) ;
#8381 = CARTESIAN_POINT ( 'NONE',  ( 46.17499999726881299, 164.1591823560292198, 12.60653300113718167 ) ) ;
#8382 = ORIENTED_EDGE ( 'NONE', *, *, #24563, .T. ) ;
#8383 = CARTESIAN_POINT ( 'NONE',  ( 50.02499999726880020, 160.0630714827496206, 15.58253174999999402 ) ) ;
#8384 = CARTESIAN_POINT ( 'NONE',  ( -52.50000000000002132, 155.0000000000000000, 6.938893903907228378E-15 ) ) ;
#8385 = CARTESIAN_POINT ( 'NONE',  ( 16.00000000000000000, 0.000000000000000000, 0.000000000000000000 ) ) ;
#8386 = CARTESIAN_POINT ( 'NONE',  ( 8.118202686958138514, 201.1607312380088501, 76.29886208192144181 ) ) ;
#8387 = CARTESIAN_POINT ( 'NONE',  ( 50.67499999726880588, 141.7447067706911810, 9.630534252274376428 ) ) ;
#8388 = CARTESIAN_POINT ( 'NONE',  ( 8.062137200540920645, 201.0835637161417822, 23.30113791807856671 ) ) ;
#8389 = CARTESIAN_POINT ( 'NONE',  ( 47.18867513459482410, 169.2658477444273331, -4.635254915624224203 ) ) ;
#8390 = VECTOR ( 'NONE', #31681, 1000.000000000000000 ) ;
#8391 = CARTESIAN_POINT ( 'NONE',  ( 75.70000000000000284, 146.4771138417591203, 11.73074641843673227 ) ) ;
#8392 = CARTESIAN_POINT ( 'NONE',  ( 62.11132485994280472, 169.2658477444273331, -4.635254915624224203 ) ) ;
#8393 = DIRECTION ( 'NONE',  ( 1.000000000000000000, 0.000000000000000000, 0.000000000000000000 ) ) ;
#8394 = CARTESIAN_POINT ( 'NONE',  ( 3.044812012440130555, 197.4746971517856764, 89.60113791807857808 ) ) ;
#8395 = CARTESIAN_POINT ( 'NONE',  ( 6.831985876597697072, -3.295913427296349951, -6.443925148804115821 ) ) ;
#8396 = CIRCLE ( 'NONE', #31777, 6.500000000000000888 ) ;
#8397 = CARTESIAN_POINT ( 'NONE',  ( 36.07499999726880446, 168.2552932293087906, 9.630534252274372875 ) ) ;
#8398 = CARTESIAN_POINT ( 'NONE',  ( -12.01549611932659722, 210.8513442034533227, 92.64886208192143613 ) ) ;
#8399 = CARTESIAN_POINT ( 'NONE',  ( 74.12499999726881583, 155.0000000000000000, 15.58253174999999402 ) ) ;
#8400 = VERTEX_POINT ( 'NONE', #15186 ) ;
#8401 = DIRECTION ( 'NONE',  ( 0.000000000000000000, 0.9949972439410068592, -0.09990237509589369735 ) ) ;
#8402 = CARTESIAN_POINT ( 'NONE',  ( 44.39999999453763024, 168.7903194862797420, -4.480746418436745593 ) ) ;
#8403 = CARTESIAN_POINT ( 'NONE',  ( -3.499999999999999556, -0.3414694520252371523, -2.900000000000000355 ) ) ;
#8404 = CARTESIAN_POINT ( 'NONE',  ( -5.335963852939856089, -6.035591050534137025, -7.593821156097342318 ) ) ;
#8405 = VERTEX_POINT ( 'NONE', #2243 ) ;
#8406 =( GEOMETRIC_REPRESENTATION_CONTEXT ( 3 ) GLOBAL_UNCERTAINTY_ASSIGNED_CONTEXT ( ( #14795 ) ) GLOBAL_UNIT_ASSIGNED_CONTEXT ( ( #17725, #27944, #7167 ) ) REPRESENTATION_CONTEXT ( 'NONE', 'WORKASPACE' ) );
#8407 = CARTESIAN_POINT ( 'NONE',  ( -10.00000000000000711, 206.9523078486584495, 92.49886208192144466 ) ) ;
#8408 = CARTESIAN_POINT ( 'NONE',  ( 3.662846001189864698, 218.4274158808046593, 36.39886208192143613 ) ) ;
#8409 = DIRECTION ( 'NONE',  ( -1.000000000000000000, 0.000000000000000000, 0.000000000000000000 ) ) ;
#8410 = CARTESIAN_POINT ( 'NONE',  ( 10.00000000000000711, 206.9523078486586201, 50.00113791807856956 ) ) ;
#8411 = ORIENTED_EDGE ( 'NONE', *, *, #22871, .F. ) ;
#8412 = CARTESIAN_POINT ( 'NONE',  ( 8.000000000000008882, 207.0476921513415220, 3.998862081921434442 ) ) ;
#8413 = CARTESIAN_POINT ( 'NONE',  ( 0.000000000000000000, 0.000000000000000000, -9.974600000000000577 ) ) ;
#8414 = EDGE_LOOP ( 'NONE', ( #31093, #16234, #31622, #32687 ) ) ;
#8415 = CARTESIAN_POINT ( 'NONE',  ( 8.015496119326595448, 204.4483345814782638, 88.14886208192143613 ) ) ;
#8416 = CARTESIAN_POINT ( 'NONE',  ( 4.984841277089725686, 213.7757310962907411, 28.55113791807857027 ) ) ;
#8417 = CARTESIAN_POINT ( 'NONE',  ( 7.499999999999999112, -4.330127018922205195, -1.000000000000000888 ) ) ;
#8418 = ORIENTED_EDGE ( 'NONE', *, *, #8366, .T. ) ;
#8419 = CARTESIAN_POINT ( 'NONE',  ( -64.50000000000000000, 155.0000000000000000, 6.938893903907228378E-15 ) ) ;
#8420 = CARTESIAN_POINT ( 'NONE',  ( 34.67499999726880588, 141.7447067706911810, 9.630534252274376428 ) ) ;
#8421 = CARTESIAN_POINT ( 'NONE',  ( 0.000000000000000000, 0.000000000000000000, -9.226681596905677907 ) ) ;
#8422 = CARTESIAN_POINT ( 'NONE',  ( -2.426778023690262742, 214.6231898156240163, 100.1011379180785781 ) ) ;
#8423 = CARTESIAN_POINT ( 'NONE',  ( 52.50000000000002132, 155.0000000000000000, 6.613633252161577047E-15 ) ) ;
#8424 = CARTESIAN_POINT ( 'NONE',  ( 55.30000000000000426, 163.5228861582408797, 11.73074641843673049 ) ) ;
#8425 = CARTESIAN_POINT ( 'NONE',  ( -2.426778023690076225, 199.3768101843759553, 73.89886208192143613 ) ) ;
#8426 = DIRECTION ( 'NONE',  ( 1.000000000000000000, -0.000000000000000000, -0.000000000000000000 ) ) ;
#8427 = CARTESIAN_POINT ( 'NONE',  ( 60.72499999726881015, 140.1801316387863778, -4.815267126137194431 ) ) ;
#8429 = ORIENTED_EDGE ( 'NONE', *, *, #28844, .T. ) ;
#8428 = CARTESIAN_POINT ( 'NONE',  ( 3.135527875058820690, 216.4958274776887492, 10.40113791807856636 ) ) ;
#8430 = CARTESIAN_POINT ( 'NONE',  ( 32.50000000000000000, 155.0000000000000000, -6.938893903907228378E-15 ) ) ;
#8431 = CARTESIAN_POINT ( 'NONE',  ( 61.32499999726881157, 164.1591823560292198, -12.60653300113719766 ) ) ;
#8432 = CARTESIAN_POINT ( 'NONE',  ( 77.07499999726881867, 141.7447067706911810, -9.630534252274385310 ) ) ;
#8433 = CARTESIAN_POINT ( 'NONE',  ( 9.736236675707914401, 214.0148392665762458, 79.70113791807857240 ) ) ;
#8434 = DIRECTION ( 'NONE',  ( -1.000000000000000000, -0.000000000000000000, -0.000000000000000000 ) ) ;
#8435 = CARTESIAN_POINT ( 'NONE',  ( -9.984503880673475606, 210.2968891136704315, 99.65113791807856103 ) ) ;
#8436 = DIRECTION ( 'NONE',  ( 0.000000000000000000, 0.000000000000000000, -1.000000000000000000 ) ) ;
#8437 = VERTEX_POINT ( 'NONE', #23020 ) ;
#8438 = CARTESIAN_POINT ( 'NONE',  ( -12.00000000000000711, 206.9523078486584780, 62.49886208192143044 ) ) ;
#8439 = CARTESIAN_POINT ( 'NONE',  ( -10.00000000000000711, 206.9523078486584495, 65.49886208192143044 ) ) ;
#8440 = CARTESIAN_POINT ( 'NONE',  ( -9.736236675707914401, 199.9851607334237542, 102.2011379180785866 ) ) ;
#8441 = CARTESIAN_POINT ( 'NONE',  ( -67.50001199999998391, 163.5195614605670187, -14.75313718340010460 ) ) ;
#8442 = CARTESIAN_POINT ( 'NONE',  ( -10.01549611932653860, 203.7984951890123284, 15.35113791807856565 ) ) ;
#8443 = CARTESIAN_POINT ( 'NONE',  ( -10.00000000000000711, 206.9523078486584495, 74.49886208192144466 ) ) ;
#8444 = EDGE_LOOP ( 'NONE', ( #25598, #29017 ) ) ;
#8445 = CARTESIAN_POINT ( 'NONE',  ( -8.118202686958039038, 201.1607312380087080, 102.2011379180785866 ) ) ;
#8446 = ORIENTED_EDGE ( 'NONE', *, *, #8328, .T. ) ;
#8447 = CARTESIAN_POINT ( 'NONE',  ( -54.79999999999999716, -6.711064459327494323E-15, 20.00000000000001776 ) ) ;
#8448 = CARTESIAN_POINT ( 'NONE',  ( 2.426778023690075337, 214.6231898156240447, 57.39886208192144323 ) ) ;
#8449 = ORIENTED_EDGE ( 'NONE', *, *, #33554, .F. ) ;
#8450 = PRODUCT_DEFINITION_SHAPE ( 'NONE', 'NONE',  #33698 ) ;
#8451 = EDGE_CURVE ( 'NONE', #28157, #33083, #29357, .T. ) ;
#8452 = CARTESIAN_POINT ( 'NONE',  ( 80.92499999726882720, 145.8408176439707802, -12.60653300113719588 ) ) ;
#8453 = ORIENTED_EDGE ( 'NONE', *, *, #2694, .F. ) ;
#8454 = DIRECTION ( 'NONE',  ( 0.5000000000000001110, 0.000000000000000000, 0.8660254037844385966 ) ) ;
#8455 = CARTESIAN_POINT ( 'NONE',  ( 72.12499999726881583, 155.0000000000000000, 15.58253174999999402 ) ) ;
#8456 = CARTESIAN_POINT ( 'NONE',  ( -4.984841277089726574, 200.2242689037092305, 69.05113791807856671 ) ) ;
#8457 = DIRECTION ( 'NONE',  ( 1.000000000000000000, 0.000000000000000000, 0.000000000000000000 ) ) ;
#8458 = CARTESIAN_POINT ( 'NONE',  ( -9.790104562688519252, 205.9634215358804852, 104.4517247136924709 ) ) ;
#8459 = EDGE_CURVE ( 'NONE', #2009, #25327, #1594, .T. ) ;
#8460 = CARTESIAN_POINT ( 'NONE',  ( 36.40000000000000568, 150.2886644046228639, -14.50000000000000888 ) ) ;
#8461 = CARTESIAN_POINT ( 'NONE',  ( 7.984503880673422316, 209.6470497212048372, 48.84886208192143897 ) ) ;
#8462 = CARTESIAN_POINT ( 'NONE',  ( -8.062137200540920645, 212.9164362838581894, 81.80113791807858092 ) ) ;
#8463 = CARTESIAN_POINT ( 'NONE',  ( -6.220909254589537696, 198.5229672870051161, 63.05113791807858092 ) ) ;
#8464 = DIRECTION ( 'NONE',  ( 1.000000000000000000, -0.000000000000000000, -0.000000000000000000 ) ) ;
#8465 = CARTESIAN_POINT ( 'NONE',  ( 2.517493886308900919, 214.5937144450984420, 22.40113791807856813 ) ) ;
#8466 = CARTESIAN_POINT ( 'NONE',  ( 0.1999999999999987899, 0.000000000000000000, 3.500000000000000000 ) ) ;
#8467 = CARTESIAN_POINT ( 'NONE',  ( -0.8808064505788995024, 6.997019658119450369, -5.875704392893736916 ) ) ;
#8468 = CARTESIAN_POINT ( 'NONE',  ( 42.62499999726881583, 138.6155565068815747, -3.929120461958505118E-15 ) ) ;
#8469 = CARTESIAN_POINT ( 'NONE',  ( -9.680171189290831535, 214.0920067884431148, 48.80113791807857382 ) ) ;
#8470 = CARTESIAN_POINT ( 'NONE',  ( -6.220909254589537696, 198.5229672870051161, 99.05113791807858092 ) ) ;
#8471 = CARTESIAN_POINT ( 'NONE',  ( 6.139770520408367460, 198.4640165459539389, 68.45113791807858661 ) ) ;
#8472 = CARTESIAN_POINT ( 'NONE',  ( -7.375838497908014268, 196.7627149292498530, 29.04886208192143471 ) ) ;
#8473 = CARTESIAN_POINT ( 'NONE',  ( 10.00000000000000711, 207.0476921513415220, 42.99886208192143044 ) ) ;
#8474 = CARTESIAN_POINT ( 'NONE',  ( 81.59999999453762598, 141.2096805137202580, -4.480746418436742040 ) ) ;
#8475 = CARTESIAN_POINT ( 'NONE',  ( 12.01549611932652972, 210.8513442034534933, 73.85113791807857808 ) ) ;
#8476 = CARTESIAN_POINT ( 'NONE',  ( 7.984503880673485376, 204.3529502787953902, 89.15113791807856103 ) ) ;
#8477 = EDGE_CURVE ( 'NONE', #7112, #10267, #1076, .T. ) ;
#8478 = CARTESIAN_POINT ( 'NONE',  ( 9.984503880673420539, 210.2968891136705167, 45.84886208192141765 ) ) ;
#8479 = DIRECTION ( 'NONE',  ( -1.000000000000000000, -0.000000000000000000, -0.000000000000000000 ) ) ;
#8480 = EDGE_LOOP ( 'NONE', ( #18089, #29553, #27544, #23084 ) ) ;
#8481 = CARTESIAN_POINT ( 'NONE',  ( -3.753561863808878130, 218.3979405102790281, 60.09886208192143897 ) ) ;
#8482 = ORIENTED_EDGE ( 'NONE', *, *, #33140, .F. ) ;
#8483 = CARTESIAN_POINT ( 'NONE',  ( 6.444103211790928043, 211.7408657792734061, 33.69886208192144039 ) ) ;
#8484 = ORIENTED_EDGE ( 'NONE', *, *, #29774, .F. ) ;
#8485 = EDGE_CURVE ( 'NONE', #28367, #29320, #683, .T. ) ;
#8486 = CIRCLE ( 'NONE', #25369, 70.00000000000002842 ) ;
#8487 = CARTESIAN_POINT ( 'NONE',  ( 76.47499999726881015, 149.9369285172503510, 15.58253174999999580 ) ) ;
#8488 = CARTESIAN_POINT ( 'NONE',  ( 87.38867513459483405, 169.2658477444273331, 4.635254915624208216 ) ) ;
#8489 = DIRECTION ( 'NONE',  ( 1.000000000000000000, 0.000000000000000000, 0.000000000000000000 ) ) ;
#8490 = CARTESIAN_POINT ( 'NONE',  ( 0.05014649552807626948, 215.4116977939061144, 49.25113791807856956 ) ) ;
#8491 = CARTESIAN_POINT ( 'NONE',  ( 32.50000000000000000, 155.0000000000000000, 15.00000000000001243 ) ) ;
#8492 = CARTESIAN_POINT ( 'NONE',  ( 6.139770520408223575, 215.5359834540460611, 33.54886208192143471 ) ) ;
#8493 = CARTESIAN_POINT ( 'NONE',  ( 72.47499999726879594, 149.9369285172503510, 15.58253174999999580 ) ) ;
#8494 = EDGE_LOOP ( 'NONE', ( #25927, #29907, #8776, #12592, #26213, #9621, #3922, #30363, #23000, #9037, #20055, #1323, #14481, #14807, #30873, #7922, #32906, #23821, #23212, #23249, #19722, #33253, #5917, #30755, #8767, #21101, #22648, #4215, #31331, #30757, #8167, #9703, #14954, #26612, #14901, #21314, #30666, #9569, #20021, #4925, #30528, #821, #24150, #2205, #14321, #21807, #22009, #20811, #2305, #33553, #5479, #1274, #8985, #20576, #27595, #12465, #15612 ) ) ;
#8495 = CARTESIAN_POINT ( 'NONE',  ( 40.98867513459482126, 163.8167787843871110, -12.13525491562423397 ) ) ;
#8496 = EDGE_CURVE ( 'NONE', #9032, #22445, #20970, .T. ) ;
#8497 = CARTESIAN_POINT ( 'NONE',  ( 42.88867513459482694, 159.8737954434936057, -15.00000000000002665 ) ) ;
#8498 = CARTESIAN_POINT ( 'NONE',  ( 2.517493886309087436, 199.4062855549015865, 19.59886208192143897 ) ) ;
#8499 = CARTESIAN_POINT ( 'NONE',  ( -9.984503880673473830, 210.2968891136704315, 48.65113791807858235 ) ) ;
#8500 = CARTESIAN_POINT ( 'NONE',  ( -7.640563834021360018E-16, -9.147862274876560562, -8.047472243342937759 ) ) ;
#8501 = CARTESIAN_POINT ( 'NONE',  ( -10.01549611932653860, 203.7984951890123284, 36.35113791807857098 ) ) ;
#8502 = CARTESIAN_POINT ( 'NONE',  ( 85.57499999726880446, 164.1591823560292198, -12.60653300113719766 ) ) ;
#8503 = CARTESIAN_POINT ( 'NONE',  ( 7.984503880673422316, 209.6470497212048372, 87.84886208192142476 ) ) ;
#8504 = CARTESIAN_POINT ( 'NONE',  ( 36.72499999726881015, 140.1801316387863778, -4.815267126137194431 ) ) ;
#8505 = CARTESIAN_POINT ( 'NONE',  ( -3.750000000000004885, 6.495190528383289141, 0.000000000000000000 ) ) ;
#8506 = CARTESIAN_POINT ( 'NONE',  ( -3.662846001190052991, 218.4274158808045740, 19.10113791807856742 ) ) ;
#8507 = CARTESIAN_POINT ( 'NONE',  ( -2.688402820137703930, -5.953403407568491623, -0.01956314070068837160 ) ) ;
#8508 = CARTESIAN_POINT ( 'NONE',  ( 59.67499999726880588, 168.2552932293087906, -9.630534252274385310 ) ) ;
#8509 = EDGE_CURVE ( 'NONE', #26453, #31583, #15852, .T. ) ;
#8510 = CARTESIAN_POINT ( 'NONE',  ( 10.01549611932653860, 210.2015048109876716, 70.85113791807854966 ) ) ;
#8511 = CARTESIAN_POINT ( 'NONE',  ( -0.05014649552810635652, 196.4853777576173002, 38.75113791807856956 ) ) ;
#8512 = AXIS2_PLACEMENT_3D ( 'NONE', #31371, #8693, #5637 ) ;
#8513 = LINE ( 'NONE', #21791, #13735 ) ;
#8514 = AXIS2_PLACEMENT_3D ( 'NONE', #15063, #14558, #4340 ) ;
#8515 = DIRECTION ( 'NONE',  ( 0.000000000000000000, -0.5000000000000008882, -0.8660254037844381525 ) ) ;
#8516 = CARTESIAN_POINT ( 'NONE',  ( -6.139770520408224463, 198.4640165459539105, 11.04886208192143648 ) ) ;
#8517 = CARTESIAN_POINT ( 'NONE',  ( 62.99999999453763166, 155.0000000000000000, 14.49999999999999467 ) ) ;
#8518 = EDGE_LOOP ( 'NONE', ( #27416, #4308, #11147, #5435 ) ) ;
#8519 = CARTESIAN_POINT ( 'NONE',  ( 9.680171189290831535, 199.9079932115568852, 47.30113791807856671 ) ) ;
#8520 = CARTESIAN_POINT ( 'NONE',  ( 77.71132485994280614, 155.0000000000000000, -15.00000000000002487 ) ) ;
#8521 = CARTESIAN_POINT ( 'NONE',  ( -10.00000000000000711, 206.9523078486584495, 20.49886208192143755 ) ) ;
#8522 = DIRECTION ( 'NONE',  ( 1.000000000000000000, -0.000000000000000000, -0.000000000000000000 ) ) ;
#8523 = VECTOR ( 'NONE', #2354, 1000.000000000000000 ) ;
#8524 = ORIENTED_EDGE ( 'NONE', *, *, #32787, .F. ) ;
#8525 = CARTESIAN_POINT ( 'NONE',  ( 0.05014649552810505201, 217.5146222423826714, 76.25113791807855534 ) ) ;
#8526 = VERTEX_POINT ( 'NONE', #10752 ) ;
#8527 = FACE_OUTER_BOUND ( 'NONE', #22213, .T. ) ;
#8528 = CARTESIAN_POINT ( 'NONE',  ( -0.8808064505793390397, -6.997019658119205232, -5.875704392894199657 ) ) ;
#8529 = EDGE_LOOP ( 'NONE', ( #10613, #15556, #22875, #2463 ) ) ;
#8530 = CARTESIAN_POINT ( 'NONE',  ( -8.015496119326531499, 204.4483345814780364, 21.35113791807856742 ) ) ;
#8531 = DIRECTION ( 'NONE',  ( -1.000000000000000000, 0.000000000000000000, 0.000000000000000000 ) ) ;
#8532 = AXIS2_PLACEMENT_3D ( 'NONE', #18716, #21260, #29429 ) ;
#8533 = CARTESIAN_POINT ( 'NONE',  ( 6.220909254589681581, 198.5229672870052582, 1.448862081921434397 ) ) ;
#8534 = CARTESIAN_POINT ( 'NONE',  ( 49.87499999726880873, 171.3844434931184253, -7.942151717890134290E-15 ) ) ;
#8535 = ORIENTED_EDGE ( 'NONE', *, *, #17294, .T. ) ;
#8536 = CARTESIAN_POINT ( 'NONE',  ( 58.32499999726881157, 145.8408176439707802, 12.60653300113718345 ) ) ;
#8537 = CARTESIAN_POINT ( 'NONE',  ( 32.50000000000000000, 155.0000000000000000, -15.00000000000002487 ) ) ;
#8538 = CARTESIAN_POINT ( 'NONE',  ( -3.376928366568182163E-14, -72.99999999999997158, 20.00000000000000000 ) ) ;
#8539 = MECHANICAL_DESIGN_GEOMETRIC_PRESENTATION_REPRESENTATION (  '', ( #11796 ), #22696 ) ;
#8540 = CARTESIAN_POINT ( 'NONE',  ( 117.5000000000000000, 183.9550983604194698, 103.9084171661920095 ) ) ;
#8541 = CARTESIAN_POINT ( 'NONE',  ( -8.118202686958138514, 212.8392687619910930, 89.79886208192144181 ) ) ;
#8542 = CARTESIAN_POINT ( 'NONE',  ( 52.27499999726880020, 160.0630714827496206, 15.58253174999999402 ) ) ;
#8543 = CARTESIAN_POINT ( 'NONE',  ( 0.05014649552810505201, 217.5146222423826714, 19.25113791807856600 ) ) ;
#8544 = DIRECTION ( 'NONE',  ( -0.000000000000000000, -0.000000000000000000, 1.000000000000000000 ) ) ;
#8545 = EDGE_CURVE ( 'NONE', #15361, #33178, #1397, .T. ) ;
#8546 = EDGE_CURVE ( 'NONE', #12687, #31608, #16285, .T. ) ;
#8547 = CARTESIAN_POINT ( 'NONE',  ( -12.00000000000000711, 206.9523078486584780, 80.49886208192144466 ) ) ;
#8548 = CIRCLE ( 'NONE', #5293, 24.99999999999999289 ) ;
#8549 = CARTESIAN_POINT ( 'NONE',  ( 73.29999999999999716, 163.5228861582408797, 11.73074641843673049 ) ) ;
#8550 = CARTESIAN_POINT ( 'NONE',  ( 62.31132485994281467, 169.2658477444273331, 4.635254915624208216 ) ) ;
#8551 = CYLINDRICAL_SURFACE ( 'NONE', #32710, 112.0000000000000711 ) ;
#8552 = CARTESIAN_POINT ( 'NONE',  ( -3.044812012440131443, 216.5253028482142952, 97.10113791807857808 ) ) ;
#8553 = EDGE_CURVE ( 'NONE', #17539, #1999, #24957, .T. ) ;
#8554 = CARTESIAN_POINT ( 'NONE',  ( 36.97499999726881015, 140.1801316387863778, -4.815267126137194431 ) ) ;
#8555 = ADVANCED_FACE ( 'NONE', ( #8359 ), #14660, .T. ) ;
#8556 = CARTESIAN_POINT ( 'NONE',  ( 0.05014649552810505201, 217.5146222423826714, 40.25113791807856956 ) ) ;
#8557 = CARTESIAN_POINT ( 'NONE',  ( 76.12499999726881583, 155.0000000000000000, 15.58253174999999402 ) ) ;
#8558 = ORIENTED_EDGE ( 'NONE', *, *, #16401, .F. ) ;
#8559 = CARTESIAN_POINT ( 'NONE',  ( 67.50000000000000000, 155.0000000000000000, -6.938893903907228378E-15 ) ) ;
#8560 = CARTESIAN_POINT ( 'NONE',  ( 43.59999999453763309, 141.2096805137202580, -4.480746418436742040 ) ) ;
#8561 =( BOUNDED_CURVE ( )  B_SPLINE_CURVE ( 2, ( #22242, #4524, #19686, #8958, #14574, #24635, #24464, #24975, #1628, #1126, #22404 ),
 .UNSPECIFIED., .F., .T. ) 
 B_SPLINE_CURVE_WITH_KNOTS ( ( 3, 2, 2, 2, 2, 3 ),
 ( 0.2142857142857139685, 0.2178571428571426383, 0.2214285714285711970, 0.2249999999999997280, 0.2285714285714282867, 0.2321428571428568455 ),
 .UNSPECIFIED. ) 
 CURVE ( )  GEOMETRIC_REPRESENTATION_ITEM ( )  RATIONAL_B_SPLINE_CURVE ( ( 1.000000000000003109, 0.9510565162951504226, 1.000000000000000000, 0.9510565162951534202, 1.000000000000000000, 0.9510565162951534202, 1.000000000000000000, 0.9510565162951534202, 1.000000000000000000, 0.9510565162951568619, 0.9999999999999965583 ) ) 
 REPRESENTATION_ITEM ( '' )  );
#8562 = CARTESIAN_POINT ( 'NONE',  ( -3.753561863808691168, 195.6020594897209435, 20.90113791807856813 ) ) ;
#8563 = AXIS2_PLACEMENT_3D ( 'NONE', #4613, #6655, #4433 ) ;
#8564 = ADVANCED_FACE ( 'NONE', ( #29302 ), #28969, .T. ) ;
#8565 = CARTESIAN_POINT ( 'NONE',  ( 40.51132485994280330, 163.8167787843871110, 12.13525491562421621 ) ) ;
#8566 = AXIS2_PLACEMENT_3D ( 'NONE', #1820, #20216, #28051 ) ;
#8567 = CARTESIAN_POINT ( 'NONE',  ( 0.000000000000000000, 0.000000000000000000, 6.500000000000000888 ) ) ;
#8568 = VERTEX_POINT ( 'NONE', #26089 ) ;
#8569 = CARTESIAN_POINT ( 'NONE',  ( -3.044812012439970683, 197.4746971517856196, 91.89886208192143613 ) ) ;
#8570 = AXIS2_PLACEMENT_3D ( 'NONE', #22774, #7442, #2163 ) ;
#8571 = B_SPLINE_CURVE_WITH_KNOTS ( 'NONE', 3,
 ( #8417, #23748, #28862, #13522, #13191, #746, #26633, #18307 ),
 .UNSPECIFIED., .F., .F.,
 ( 4, 2, 2, 4 ),
 ( 0.006061689441712453386, 0.007174127271521678166, 0.008286565101330902947, 0.01051144076094935251 ),
 .UNSPECIFIED. ) ;
#8572 = CARTESIAN_POINT ( 'NONE',  ( 9.736236675708031640, 199.9851607334238963, 37.29886208192143471 ) ) ;
#8573 = CARTESIAN_POINT ( 'NONE',  ( -10.33420400187145027, 207.8560350444080598, 102.5922263069843581 ) ) ;
#8574 = CARTESIAN_POINT ( 'NONE',  ( -6.220909254589537696, 198.5229672870051161, 48.05113791807858092 ) ) ;
#8575 = ORIENTED_EDGE ( 'NONE', *, *, #23263, .F. ) ;
#8576 = CARTESIAN_POINT ( 'NONE',  ( 8.015496119326595448, 204.4483345814782638, 13.14886208192143613 ) ) ;
#8577 = CARTESIAN_POINT ( 'NONE',  ( -27.50000000000000000, 15.87713240271469672, -18.00000000000000000 ) ) ;
#8578 = VERTEX_POINT ( 'NONE', #16343 ) ;
#8579 = CARTESIAN_POINT ( 'NONE',  ( 6.500168698208244500, 202.3363017425938324, 97.29886208192142760 ) ) ;
#8580 = CARTESIAN_POINT ( 'NONE',  ( -6.500168698208129925, 202.3363017425936050, 39.20113791807857240 ) ) ;
#8581 = DIRECTION ( 'NONE',  ( 0.000000000000000000, 0.000000000000000000, -1.000000000000000000 ) ) ;
#8582 = VERTEX_POINT ( 'NONE', #26737 ) ;
#8583 = CARTESIAN_POINT ( 'NONE',  ( 34.02499999726880731, 160.0630714827496206, 15.58253174999999402 ) ) ;
#8584 = CARTESIAN_POINT ( 'NONE',  ( -6.220909254589682469, 215.4770327129946850, 53.94886208192144039 ) ) ;
#8585 = CARTESIAN_POINT ( 'NONE',  ( 86.82499999726879025, 141.7447067706911810, -9.630534252274385310 ) ) ;
#8586 = FACE_OUTER_BOUND ( 'NONE', #2136, .T. ) ;
#8587 = CARTESIAN_POINT ( 'NONE',  ( -7.984503880673488041, 209.6470497212046098, 96.65113791807858945 ) ) ;
#8588 = DIRECTION ( 'NONE',  ( -1.000000000000000000, 0.000000000000000000, 6.123233995736766036E-17 ) ) ;
#8589 = CARTESIAN_POINT ( 'NONE',  ( 54.59999999999999432, 159.7113355953771077, -14.50000000000000888 ) ) ;
#8590 = CARTESIAN_POINT ( 'NONE',  ( -2.426778023690076225, 199.3768101843759553, 70.89886208192143613 ) ) ;
#8591 = CARTESIAN_POINT ( 'NONE',  ( 125.5000000000000000, 155.0000000000000000, -6.938893903907228378E-15 ) ) ;
#8592 = AXIS2_PLACEMENT_3D ( 'NONE', #26236, #8194, #18579 ) ;
#8593 = CARTESIAN_POINT ( 'NONE',  ( 55.12499999726881583, 155.0000000000000000, -15.58253175000000823 ) ) ;
#8594 = CARTESIAN_POINT ( 'NONE',  ( -10.00000000000000711, 207.0476921513413515, 6.501137918078566003 ) ) ;
#8595 = CARTESIAN_POINT ( 'NONE',  ( -6.826296012759691223, -2.664253980652245168, -6.325071479460635970 ) ) ;
#8596 = CARTESIAN_POINT ( 'NONE',  ( 60.92499999726882010, 145.8408176439707802, -12.60653300113719588 ) ) ;
#8597 = CARTESIAN_POINT ( 'NONE',  ( 79.67499999726881299, 168.2552932293087906, -9.630534252274385310 ) ) ;
#8598 = CARTESIAN_POINT ( 'NONE',  ( 9.736236675707914401, 214.0148392665762458, 76.70113791807857240 ) ) ;
#8599 = CARTESIAN_POINT ( 'NONE',  ( -10.01549611932653860, 203.7984951890123000, 93.35113791807857808 ) ) ;
#8600 = DIRECTION ( 'NONE',  ( 0.000000000000000000, 0.000000000000000000, 1.000000000000000000 ) ) ;
#8601 = VERTEX_POINT ( 'NONE', #16019 ) ;
#8602 = CARTESIAN_POINT ( 'NONE',  ( -9.984503880673420539, 203.7031108863293980, 5.348862081921433642 ) ) ;
#8603 = CARTESIAN_POINT ( 'NONE',  ( -7.456977232089471386, 217.1783343296987709, 62.94886208192144039 ) ) ;
#8604 = CARTESIAN_POINT ( 'NONE',  ( -3.135527875058982783, 216.4958274776886924, 63.09886208192143187 ) ) ;
#8605 = CARTESIAN_POINT ( 'NONE',  ( -0.05014649552828442242, 219.6175466908591716, 3.248862081921433997 ) ) ;
#8606 = DIRECTION ( 'NONE',  ( -0.000000000000000000, -0.000000000000000000, 1.000000000000000000 ) ) ;
#8607 = AXIS2_PLACEMENT_3D ( 'NONE', #6793, #17181, #4405 ) ;
#8608 = CARTESIAN_POINT ( 'NONE',  ( 6.139770520408368348, 198.4640165459539674, 26.45113791807856884 ) ) ;
#8609 = CARTESIAN_POINT ( 'NONE',  ( 10.00000000000000711, 207.0476921513415220, 87.99886208192144466 ) ) ;
#8610 = VECTOR ( 'NONE', #15992, 1000.000000000000114 ) ;
#8611 = VERTEX_POINT ( 'NONE', #3072 ) ;
#8612 = CARTESIAN_POINT ( 'NONE',  ( 2.690931834596283156, -5.951943280390046276, -5.793705359219412742E-15 ) ) ;
#8613 = VERTEX_POINT ( 'NONE', #23851 ) ;
#8614 = CARTESIAN_POINT ( 'NONE',  ( 3.214438021527930012, 2.185595227304852450, -0.2174200650117560363 ) ) ;
#8615 = CARTESIAN_POINT ( 'NONE',  ( 6.500168698208244500, 202.3363017425938324, 61.29886208192144892 ) ) ;
#8616 = ORIENTED_EDGE ( 'NONE', *, *, #5953, .F. ) ;
#8617 = VECTOR ( 'NONE', #17652, 1000.000000000000114 ) ;
#8618 = CARTESIAN_POINT ( 'NONE',  ( 79.12499999726881583, 155.0000000000000000, -15.58253175000000823 ) ) ;
#8619 = ORIENTED_EDGE ( 'NONE', *, *, #18971, .T. ) ;
#8620 = CARTESIAN_POINT ( 'NONE',  ( -3.250000000000004441, 5.629165124598849879, 0.000000000000000000 ) ) ;
#8621 = CARTESIAN_POINT ( 'NONE',  ( 69.52499999726880731, 169.8198683612136222, -4.815267126137197984 ) ) ;
#8622 = CARTESIAN_POINT ( 'NONE',  ( -7.984503880673488041, 209.6470497212046098, 66.65113791807856103 ) ) ;
#8623 = CARTESIAN_POINT ( 'NONE',  ( 10.00000000000000888, 207.0000000000002842, 5.551115123125782702E-14 ) ) ;
#8624 = CARTESIAN_POINT ( 'NONE',  ( -9.139829196538601153, 206.4498403098741335, 104.0238431579207088 ) ) ;
#8625 = CARTESIAN_POINT ( 'NONE',  ( 36.19999999999999574, 142.6655632788954620, -8.961492836873480528 ) ) ;
#8626 = CARTESIAN_POINT ( 'NONE',  ( -4.903702542908436435, 200.1653181626580249, 41.04886208192144181 ) ) ;
#8627 = CONICAL_SURFACE ( 'NONE', #27671, 2.000000000000000000, 0.9599310885968733720 ) ;
#8628 = CARTESIAN_POINT ( 'NONE',  ( -0.05014649552810635652, 196.4853777576173002, 77.75113791807856956 ) ) ;
#8629 = CARTESIAN_POINT ( 'NONE',  ( 8.118202686958039038, 212.8392687619912635, 64.70113791807857240 ) ) ;
#8630 = VECTOR ( 'NONE', #26673, 1000.000000000000000 ) ;
#8631 = AXIS2_PLACEMENT_3D ( 'NONE', #26761, #11272, #875 ) ;
#8632 = CARTESIAN_POINT ( 'NONE',  ( 8.640141755188686545, 206.6086104956403915, 111.6972426105882477 ) ) ;
#8633 = CARTESIAN_POINT ( 'NONE',  ( 6.444103211791042618, 202.2591342207267644, 20.30113791807857027 ) ) ;
#8634 = CARTESIAN_POINT ( 'NONE',  ( 115.4999999999999858, 102.0000000000001990, 91.79869280115065067 ) ) ;
#8635 = FACE_OUTER_BOUND ( 'NONE', #19604, .T. ) ;
#8636 = CARTESIAN_POINT ( 'NONE',  ( 47.52499999726881441, 169.8198683612136222, -4.815267126137197984 ) ) ;
#8637 = CARTESIAN_POINT ( 'NONE',  ( 12.01549611932652972, 210.8513442034534933, 49.85113791807857808 ) ) ;
#8638 = DIRECTION ( 'NONE',  ( -1.000000000000000000, -0.000000000000000000, -0.000000000000000000 ) ) ;
#8639 = CARTESIAN_POINT ( 'NONE',  ( -10.01549611932653860, 203.7984951890123284, 96.35113791807853545 ) ) ;
#8640 = EDGE_CURVE ( 'NONE', #26498, #29684, #20855, .T. ) ;
#8641 = CARTESIAN_POINT ( 'NONE',  ( -0.05014649552810635652, 196.4853777576173002, 68.75113791807855534 ) ) ;
#8642 = AXIS2_PLACEMENT_3D ( 'NONE', #13210, #8434, #11784 ) ;
#8643 = CARTESIAN_POINT ( 'NONE',  ( 12.01549611932659367, 203.1486557965466773, 34.14886208192143613 ) ) ;
#8644 = CARTESIAN_POINT ( 'NONE',  ( 9.984503880673420539, 210.2968891136705736, 36.84886208192143187 ) ) ;
#8645 = CARTESIAN_POINT ( 'NONE',  ( 88.59999999453762598, 168.7903194862797420, 4.480746418436729606 ) ) ;
#8646 = CARTESIAN_POINT ( 'NONE',  ( 0.05014649552807549926, 219.6175466908591716, 76.25113791807856956 ) ) ;
#8647 = CARTESIAN_POINT ( 'NONE',  ( -8.000000000000008882, 207.0476921513413515, 102.5011379180785696 ) ) ;
#8648 = CARTESIAN_POINT ( 'NONE',  ( -6.139770520408224463, 198.4640165459539389, 53.04886208192142050 ) ) ;
#8649 = CARTESIAN_POINT ( 'NONE',  ( -58.50000000000002132, 185.0000000000000000, 0.000000000000000000 ) ) ;
#8650 = ORIENTED_EDGE ( 'NONE', *, *, #28490, .T. ) ;
#8651 = CARTESIAN_POINT ( 'NONE',  ( -11.98450388067341876, 203.0532714938636047, 62.34886208192143187 ) ) ;
#8652 = ORIENTED_EDGE ( 'NONE', *, *, #1394, .T. ) ;
#8653 = CARTESIAN_POINT ( 'NONE',  ( 4.903702542908435547, 213.8346818373419751, 30.54886208192144181 ) ) ;
#8654 = CIRCLE ( 'NONE', #8116, 0.2000000000000000944 ) ;
#8655 = VERTEX_POINT ( 'NONE', #24696 ) ;
#8656 = CARTESIAN_POINT ( 'NONE',  ( 75.97499999726881015, 169.8198683612136222, 4.815267126137181997 ) ) ;
#8657 = CARTESIAN_POINT ( 'NONE',  ( -9.736236675707914401, 199.9851607334237542, 72.20113791807857240 ) ) ;
#8658 = DIRECTION ( 'NONE',  ( 1.000000000000000000, 0.000000000000000000, 0.000000000000000000 ) ) ;
#8659 = CARTESIAN_POINT ( 'NONE',  ( 6.444103211791042618, 202.2591342207267644, 47.30113791807858092 ) ) ;
#8660 = LINE ( 'NONE', #8491, #12339 ) ;
#8661 = CARTESIAN_POINT ( 'NONE',  ( -6.220909254589682469, 215.4770327129946850, 35.94886208192141908 ) ) ;
#8662 = CARTESIAN_POINT ( 'NONE',  ( 71.67499999726881299, 168.2552932293087906, -9.630534252274387086 ) ) ;
#8663 = ORIENTED_EDGE ( 'NONE', *, *, #15758, .T. ) ;
#8664 = CARTESIAN_POINT ( 'NONE',  ( 67.78867513459482552, 155.0000000000000000, 15.00000000000001243 ) ) ;
#8665 = CARTESIAN_POINT ( 'NONE',  ( -60.00000000000000000, -7.347880794884118356E-15, -35.00000000000000000 ) ) ;
#8666 = CARTESIAN_POINT ( 'NONE',  ( 42.78867513459481842, 155.0000000000000000, -15.00000000000002487 ) ) ;
#8667 = CARTESIAN_POINT ( 'NONE',  ( 7.984503880673422316, 209.6470497212048372, 12.84886208192143719 ) ) ;
#8668 = CARTESIAN_POINT ( 'NONE',  ( 9.984503880673470277, 203.7031108863295401, 53.15113791807857524 ) ) ;
#8669 = DIRECTION ( 'NONE',  ( -1.000000000000000000, -0.000000000000000000, -0.000000000000000000 ) ) ;
#8670 = CARTESIAN_POINT ( 'NONE',  ( 10.00000000000000711, 206.9523078486586201, 41.00113791807856956 ) ) ;
#8671 = CARTESIAN_POINT ( 'NONE',  ( 84.37499999726881583, 155.0000000000000000, 15.58253174999999402 ) ) ;
#8672 = ITEM_DEFINED_TRANSFORMATION ( 'NONE', 'NONE', #1224,  #2404 ) ;
#8673 = CARTESIAN_POINT ( 'NONE',  ( -6.500168698208244500, 211.6636982574061676, 101.7988620819214560 ) ) ;
#8674 = CARTESIAN_POINT ( 'NONE',  ( 40.62499999726880873, 138.6155565068815463, -3.929120461958505118E-15 ) ) ;
#8675 = LINE ( 'NONE', #19067, #6750 ) ;
#8676 = CARTESIAN_POINT ( 'NONE',  ( 125.5000000000000000, 155.0000000000000000, -6.938893903907228378E-15 ) ) ;
#8677 = CARTESIAN_POINT ( 'NONE',  ( 7.375838497908181246, 196.7627149292499666, 17.45113791807856174 ) ) ;
#8678 = DIRECTION ( 'NONE',  ( 0.000000000000000000, 0.000000000000000000, 1.000000000000000000 ) ) ;
#8679 = CARTESIAN_POINT ( 'NONE',  ( 60.77499999726881441, 140.1801316387863778, 4.815267126137185549 ) ) ;
#8680 = CARTESIAN_POINT ( 'NONE',  ( 0.05014649552810505201, 217.5146222423826714, 64.25113791807856956 ) ) ;
#8681 = EDGE_CURVE ( 'NONE', #4795, #1780, #2720, .T. ) ;
#8682 = CARTESIAN_POINT ( 'NONE',  ( 0.05014649552810506589, 217.5146222423826714, 37.25113791807856956 ) ) ;
#8683 = CARTESIAN_POINT ( 'NONE',  ( -13.75000000000001243, -23.81569860407206107, -18.00000000000000000 ) ) ;
#8684 = CARTESIAN_POINT ( 'NONE',  ( 55.38867513459481984, 169.2658477444273331, 4.635254915624208216 ) ) ;
#8685 = CARTESIAN_POINT ( 'NONE',  ( 12.00000000000000711, 207.0476921513415220, 3.998862081921433997 ) ) ;
#8686 = CARTESIAN_POINT ( 'NONE',  ( 0.05014649552828275014, 196.4853777576173002, 10.74886208192143577 ) ) ;
#8687 = CARTESIAN_POINT ( 'NONE',  ( 57.99999999453763166, 155.0000000000000000, -14.50000000000000711 ) ) ;
#8688 = EDGE_LOOP ( 'NONE', ( #5957, #23120, #29181, #3800, #12859 ) ) ;
#8689 = CARTESIAN_POINT ( 'NONE',  ( -3.753561863808691168, 195.6020594897209435, 44.90113791807856813 ) ) ;
#8690 = CARTESIAN_POINT ( 'NONE',  ( 6.500168698208129925, 211.6636982574063381, 73.70113791807857240 ) ) ;
#8691 = CARTESIAN_POINT ( 'NONE',  ( 32.50000000000000000, 155.0000000000000000, -6.938893903907228378E-15 ) ) ;
#8692 = CARTESIAN_POINT ( 'NONE',  ( -8.062137200540822946, 201.0835637161416400, 23.19886208192143684 ) ) ;
#8693 = DIRECTION ( 'NONE',  ( 1.000000000000000000, 0.000000000000000000, 0.000000000000000000 ) ) ;
#8694 = EDGE_LOOP ( 'NONE', ( #9272, #24493, #28193, #7365 ) ) ;
#8695 = EDGE_CURVE ( 'NONE', #8859, #30928, #5427, .T. ) ;
#8696 = CARTESIAN_POINT ( 'NONE',  ( -6.139770520408369237, 215.5359834540460042, 84.95113791807858661 ) ) ;
#8697 = ORIENTED_EDGE ( 'NONE', *, *, #27673, .T. ) ;
#8698 = CARTESIAN_POINT ( 'NONE',  ( 50.01132485994283172, 167.7597621252805880, -9.270509831248443078 ) ) ;
#8699 = FACE_OUTER_BOUND ( 'NONE', #20171, .T. ) ;
#8700 = ORIENTED_EDGE ( 'NONE', *, *, #20818, .T. ) ;
#8701 = CARTESIAN_POINT ( 'NONE',  ( 4.903702542908601636, 200.1653181626581102, 20.45113791807856529 ) ) ;
#8702 = EDGE_CURVE ( 'NONE', #9440, #10897, #2992, .T. ) ;
#8703 =( BOUNDED_CURVE ( )  B_SPLINE_CURVE ( 2, ( #2046, #163, #12597, #8005, #30669, #33556, #33390, #5438, #12435, #10564, #20441 ),
 .UNSPECIFIED., .F., .T. ) 
 B_SPLINE_CURVE_WITH_KNOTS ( ( 3, 2, 2, 2, 2, 3 ),
 ( 0.6428571428571426827, 0.6464285714285712414, 0.6499999999999998002, 0.6535714285714284699, 0.6571428571428570287, 0.6607142857142855874 ),
 .UNSPECIFIED. ) 
 CURVE ( )  GEOMETRIC_REPRESENTATION_ITEM ( )  RATIONAL_B_SPLINE_CURVE ( ( 1.000000000000001554, 0.9510565162951518658, 1.000000000000000000, 0.9510565162951534202, 1.000000000000000000, 0.9510565162951534202, 1.000000000000000000, 0.9510565162951534202, 1.000000000000000000, 0.9510565162951534202, 1.000000000000000000 ) ) 
 REPRESENTATION_ITEM ( '' )  );
#8704 = CARTESIAN_POINT ( 'NONE',  ( -60.02503143742045921, 194.9506873066471542, -1.987662087495396301 ) ) ;
#8705 = CARTESIAN_POINT ( 'NONE',  ( -3.135527875058982783, 216.4958274776886924, 6.098862081921434530 ) ) ;
#8706 = CARTESIAN_POINT ( 'NONE',  ( 47.27499999726880731, 149.9369285172503510, -15.58253175000000823 ) ) ;
#8707 = ORIENTED_EDGE ( 'NONE', *, *, #21173, .T. ) ;
#8708 = CARTESIAN_POINT ( 'NONE',  ( 54.22499999726881015, 149.9369285172503510, 15.58253174999999580 ) ) ;
#8709 = CARTESIAN_POINT ( 'NONE',  ( -125.0000000000000000, -95.00000000000000000, -20.00000000000000000 ) ) ;
#8710 = CARTESIAN_POINT ( 'NONE',  ( 7.549006887134069643, 4.358421158401191597, -7.700127545397312367 ) ) ;
#8711 = DIRECTION ( 'NONE',  ( 0.000000000000000000, 0.000000000000000000, -1.000000000000000000 ) ) ;
#8712 = CARTESIAN_POINT ( 'NONE',  ( -6.139770520408224463, 198.4640165459539389, 86.04886208192144181 ) ) ;
#8713 = EDGE_CURVE ( 'NONE', #11826, #6436, #4894, .T. ) ;
#8714 = CARTESIAN_POINT ( 'NONE',  ( 58.07499999726880446, 168.2552932293087906, 9.630534252274372875 ) ) ;
#8715 = CARTESIAN_POINT ( 'NONE',  ( -3.135527875058821579, 197.5041725223112223, 26.90113791807856813 ) ) ;
#8716 = CARTESIAN_POINT ( 'NONE',  ( 72.78867513459482552, 155.0000000000000000, -15.00000000000002487 ) ) ;
#8717 = CARTESIAN_POINT ( 'NONE',  ( 12.00000000000000711, 207.0476921513415220, 78.99886208192144466 ) ) ;
#8718 = CARTESIAN_POINT ( 'NONE',  ( 76.59999999999999432, 159.7113355953771077, -14.50000000000000888 ) ) ;
#8719 = CARTESIAN_POINT ( 'NONE',  ( -27.50000000000000000, -15.87713240271474824, -15.54379906938135214 ) ) ;
#8720 = CARTESIAN_POINT ( 'NONE',  ( 97.30927364589244632, 155.0000000000000000, 31.00000000000000000 ) ) ;
#8721 = CARTESIAN_POINT ( 'NONE',  ( 8.118202686958039038, 212.8392687619912635, 94.70113791807857240 ) ) ;
#8722 = CARTESIAN_POINT ( 'NONE',  ( 33.38867513459482694, 169.2658477444273331, 4.635254915624208216 ) ) ;
#8723 = CARTESIAN_POINT ( 'NONE',  ( 45.37499999726880873, 155.0000000000000000, -15.58253175000000823 ) ) ;
#8724 = CARTESIAN_POINT ( 'NONE',  ( -6.139770520408369237, 215.5359834540460042, 36.95113791807857240 ) ) ;
#8725 = CARTESIAN_POINT ( 'NONE',  ( 78.82499999726881867, 141.7447067706911810, -9.630534252274385310 ) ) ;
#8726 = CIRCLE ( 'NONE', #9827, 50.00000000000000000 ) ;
#8727 = ORIENTED_EDGE ( 'NONE', *, *, #24292, .F. ) ;
#8728 = CARTESIAN_POINT ( 'NONE',  ( 39.39999999453763024, 141.2096805137202580, 4.480746418436733158 ) ) ;
#8729 = CARTESIAN_POINT ( 'NONE',  ( -12.01549611932652972, 203.1486557965464499, 15.35113791807856387 ) ) ;
#8730 = CARTESIAN_POINT ( 'NONE',  ( 40.01132485994281041, 167.7597621252805880, -9.270509831248443078 ) ) ;
#8731 = CARTESIAN_POINT ( 'NONE',  ( 0.000000000000000000, 0.000000000000000000, -18.00000000000000000 ) ) ;
#8732 = ORIENTED_EDGE ( 'NONE', *, *, #31571, .F. ) ;
#8733 = CARTESIAN_POINT ( 'NONE',  ( 0.05014649552828288198, 194.3824533091408000, 28.74886208192144110 ) ) ;
#8734 = CARTESIAN_POINT ( 'NONE',  ( 115.4999999999999858, 257.3881375866408803, -27.43481878086871717 ) ) ;
#8735 = CARTESIAN_POINT ( 'NONE',  ( 6.139770520408368348, 198.4640165459539674, 50.45113791807857240 ) ) ;
#8736 = EDGE_LOOP ( 'NONE', ( #19997, #5391 ) ) ;
#8737 = CARTESIAN_POINT ( 'NONE',  ( -6.444103211790928043, 202.2591342207265939, 14.19886208192143684 ) ) ;
#8738 = EDGE_CURVE ( 'NONE', #16522, #6050, #22468, .T. ) ;
#8739 = ADVANCED_FACE ( 'NONE', ( #16512 ), #19244, .T. ) ;
#8740 = PRODUCT_DEFINITION_CONTEXT ( 'detailed design', #14200, 'design' ) ;
#8741 = FACE_OUTER_BOUND ( 'NONE', #1415, .T. ) ;
#8742 = ORIENTED_EDGE ( 'NONE', *, *, #6007, .F. ) ;
#8743 = CARTESIAN_POINT ( 'NONE',  ( -0.05014649552828365914, 215.4116977939061144, 96.24886208192144466 ) ) ;
#8744 = EDGE_CURVE ( 'NONE', #29684, #6898, #19641, .T. ) ;
#8745 = CARTESIAN_POINT ( 'NONE',  ( -6.444103211791042618, 211.7408657792732356, 42.80113791807857382 ) ) ;
#8746 = DIRECTION ( 'NONE',  ( -0.2649168722799636333, 0.9642688156137663169, -0.002168413296789690158 ) ) ;
#8747 = ORIENTED_EDGE ( 'NONE', *, *, #6479, .F. ) ;
#8748 = CARTESIAN_POINT ( 'NONE',  ( 39.72499999726881015, 169.8198683612136222, 4.815267126137181997 ) ) ;
#8749 = CARTESIAN_POINT ( 'NONE',  ( -0.05014649552828403384, 217.5146222423826714, 60.24886208192142334 ) ) ;
#8750 = EDGE_CURVE ( 'NONE', #21724, #10366, #27186, .T. ) ;
#8751 = CARTESIAN_POINT ( 'NONE',  ( 40.27499999726881441, 160.0630714827496206, 15.58253174999999402 ) ) ;
#8752 = CARTESIAN_POINT ( 'NONE',  ( -6.500000000000002665, -2.501851166488385125, -5.848636054922036642 ) ) ;
#8753 = CARTESIAN_POINT ( 'NONE',  ( 7.984503880673485376, 204.3529502787953902, 95.15113791807856103 ) ) ;
#8754 = CARTESIAN_POINT ( 'NONE',  ( 54.20000000000000284, 142.6655632788954620, -8.961492836873480528 ) ) ;
#8755 = CARTESIAN_POINT ( 'NONE',  ( -6.500168698208244500, 211.6636982574061676, 71.79886208192142760 ) ) ;
#8756 = CARTESIAN_POINT ( 'NONE',  ( -6.500000000000000888, 0.000000000000000000, 0.000000000000000000 ) ) ;
#8757 = CARTESIAN_POINT ( 'NONE',  ( 54.92499999726881299, 145.8408176439707802, -12.60653300113719588 ) ) ;
#8759 = ORIENTED_EDGE ( 'NONE', *, *, #11483, .T. ) ;
#8758 = CARTESIAN_POINT ( 'NONE',  ( 9.984503880673473830, 203.7031108863295401, 14.15113791807856636 ) ) ;
#8760 = CARTESIAN_POINT ( 'NONE',  ( -6.815962252199548210, 1.383413844627830791, -6.173425845474762141 ) ) ;
#8761 = AXIS2_PLACEMENT_3D ( 'NONE', #14378, #10866, #8302 ) ;
#8762 = CARTESIAN_POINT ( 'NONE',  ( 67.32499999726881867, 164.1591823560292198, -12.60653300113719766 ) ) ;
#8763 = CARTESIAN_POINT ( 'NONE',  ( 75.47499999726881015, 160.0630714827496206, -15.58253175000000823 ) ) ;
#8764 = CARTESIAN_POINT ( 'NONE',  ( -9.680171189290831535, 214.0920067884431148, 75.80113791807858092 ) ) ;
#8765 = CARTESIAN_POINT ( 'NONE',  ( -6.139770520408368348, 215.5359834540460042, 96.95113791807857240 ) ) ;
#8766 = CARTESIAN_POINT ( 'NONE',  ( 53.78867513459483263, 155.0000000000000000, 15.00000000000001243 ) ) ;
#8767 = ORIENTED_EDGE ( 'NONE', *, *, #9576, .F. ) ;
#8768 = CARTESIAN_POINT ( 'NONE',  ( -8.062137200540822946, 201.0835637161416400, 2.198862081921434175 ) ) ;
#8769 = CARTESIAN_POINT ( 'NONE',  ( -7.456977232089471386, 217.1783343296987709, 65.94886208192144750 ) ) ;
#8770 = CARTESIAN_POINT ( 'NONE',  ( 10.00000000000000711, 207.0476921513415220, 66.99886208192143044 ) ) ;
#8771 = CARTESIAN_POINT ( 'NONE',  ( -7.456977232089471386, 217.1783343296987709, 5.948862081921435063 ) ) ;
#8772 = FACE_OUTER_BOUND ( 'NONE', #23582, .T. ) ;
#8773 = CARTESIAN_POINT ( 'NONE',  ( -10.01549611932653860, 203.7984951890123284, 18.35113791807856742 ) ) ;
#8774 = CARTESIAN_POINT ( 'NONE',  ( 8.118202686958138514, 201.1607312380088501, 88.29886208192142760 ) ) ;
#8775 = EDGE_CURVE ( 'NONE', #18587, #25169, #24461, .T. ) ;
#8776 = ORIENTED_EDGE ( 'NONE', *, *, #6265, .T. ) ;
#8777 = ORIENTED_EDGE ( 'NONE', *, *, #30012, .T. ) ;
#8778 = FACE_OUTER_BOUND ( 'NONE', #29996, .T. ) ;
#8779 = CARTESIAN_POINT ( 'NONE',  ( 4.984841277089891776, 200.2242689037093726, 73.44886208192143329 ) ) ;
#8780 = ORIENTED_EDGE ( 'NONE', *, *, #9157, .T. ) ;
#8781 = CARTESIAN_POINT ( 'NONE',  ( 84.42499999726881299, 141.7447067706911810, 9.630534252274376428 ) ) ;
#8782 = ORIENTED_EDGE ( 'NONE', *, *, #1292, .T. ) ;
#8783 = CARTESIAN_POINT ( 'NONE',  ( 69.38867513459481984, 169.2658477444273331, 4.635254915624208216 ) ) ;
#8784 = CONICAL_SURFACE ( 'NONE', #11516, 32.00000000000002842, 1.466076571675244411 ) ;
#8785 = CARTESIAN_POINT ( 'NONE',  ( 72.42499999726881299, 141.7447067706911810, 9.630534252274376428 ) ) ;
#8786 = CARTESIAN_POINT ( 'NONE',  ( -6.444103211791042618, 211.7408657792732356, 66.80113791807858092 ) ) ;
#8787 = DIRECTION ( 'NONE',  ( 0.000000000000000000, 0.000000000000000000, -1.000000000000000000 ) ) ;
#8788 = AXIS2_PLACEMENT_3D ( 'NONE', #22196, #25260, #14864 ) ;
#8789 = CARTESIAN_POINT ( 'NONE',  ( 32.99999999999999289, 170.2462022514548323, -7.872454543227099337E-15 ) ) ;
#8790 = CARTESIAN_POINT ( 'NONE',  ( -2.426778023690076225, 199.3768101843759553, 40.89886208192144323 ) ) ;
#8791 = CARTESIAN_POINT ( 'NONE',  ( 10.01549611932653860, 210.2015048109876716, 88.85113791807857808 ) ) ;
#8792 = CARTESIAN_POINT ( 'NONE',  ( 8.118202686958039038, 212.8392687619912635, 67.70113791807858661 ) ) ;
#8793 = DIRECTION ( 'NONE',  ( 1.000000000000000000, 0.000000000000000000, 0.000000000000000000 ) ) ;
#8794 = CARTESIAN_POINT ( 'NONE',  ( -2.517493886308901807, 199.4062855549015012, 20.90113791807856813 ) ) ;
#8795 = DIRECTION ( 'NONE',  ( -1.000000000000000000, 0.000000000000000000, 0.000000000000000000 ) ) ;
#8796 = CARTESIAN_POINT ( 'NONE',  ( 0.2813450144774485850, 7.667988119308852824, -6.122077150241853616 ) ) ;
#8797 = CARTESIAN_POINT ( 'NONE',  ( 47.42499999726880588, 168.2552932293087906, -9.630534252274387086 ) ) ;
#8798 = CARTESIAN_POINT ( 'NONE',  ( 7.375838497908181246, 196.7627149292499666, 44.45113791807857240 ) ) ;
#8799 = CARTESIAN_POINT ( 'NONE',  ( -68.50000000000000000, 215.0000000000000000, 2.500000000000000000 ) ) ;
#8800 = CARTESIAN_POINT ( 'NONE',  ( 9.984503880673470277, 203.7031108863295401, 98.15113791807858945 ) ) ;
#8801 = CARTESIAN_POINT ( 'NONE',  ( 10.00000000000000711, 206.9523078486586201, 65.00113791807856956 ) ) ;
#8802 = CARTESIAN_POINT ( 'NONE',  ( -0.05014649552828442242, 219.6175466908591716, 33.24886208192143755 ) ) ;
#8803 = CARTESIAN_POINT ( 'NONE',  ( 10.01549611932659367, 203.7984951890124421, 34.14886208192143613 ) ) ;
#8804 = CARTESIAN_POINT ( 'NONE',  ( 84.39999999453762314, 168.7903194862797420, -4.480746418436745593 ) ) ;
#8805 = CARTESIAN_POINT ( 'NONE',  ( -9.680171189290831535, 214.0920067884431148, 72.80113791807858092 ) ) ;
#8806 = CARTESIAN_POINT ( 'NONE',  ( -6.500168698208129925, 202.3363017425936050, 99.20113791807858661 ) ) ;
#8807 = CARTESIAN_POINT ( 'NONE',  ( -3.044812012439970683, 197.4746971517856196, 61.89886208192143613 ) ) ;
#8808 = VERTEX_POINT ( 'NONE', #29639 ) ;
#8809 = CARTESIAN_POINT ( 'NONE',  ( 12.01549611932659367, 203.1486557965466773, 61.14886208192143613 ) ) ;
#8810 = ORIENTED_EDGE ( 'NONE', *, *, #23076, .F. ) ;
#8811 = CARTESIAN_POINT ( 'NONE',  ( 72.57499999726880446, 145.8408176439707802, 12.60653300113718345 ) ) ;
#8812 = CARTESIAN_POINT ( 'NONE',  ( 0.05014649552828262524, 198.5883022060938572, 43.74886208192144466 ) ) ;
#8813 = ORIENTED_EDGE ( 'NONE', *, *, #13334, .F. ) ;
#8814 = CARTESIAN_POINT ( 'NONE',  ( 74.87499999726880162, 138.6155565068815747, -3.929120461958505118E-15 ) ) ;
#8815 = LINE ( 'NONE', #495, #31995 ) ;
#8816 = DIRECTION ( 'NONE',  ( -0.000000000000000000, -0.000000000000000000, -1.000000000000000000 ) ) ;
#8817 = CARTESIAN_POINT ( 'NONE',  ( -4.903702542908602524, 213.8346818373418898, 54.95113791807857240 ) ) ;
#8818 = ADVANCED_FACE ( 'NONE', ( #6468, #16851 ), #32859, .F. ) ;
#8819 = CARTESIAN_POINT ( 'NONE',  ( -8.062137200540822946, 201.0835637161416400, 29.19886208192143684 ) ) ;
#8820 = CARTESIAN_POINT ( 'NONE',  ( 68.97499999726881015, 140.1801316387863778, -4.815267126137194431 ) ) ;
#8821 = EDGE_LOOP ( 'NONE', ( #21758, #8810, #9214, #19710 ) ) ;
#8822 = CARTESIAN_POINT ( 'NONE',  ( 41.78867513459481842, 155.0000000000000000, 15.00000000000001243 ) ) ;
#8823 = AXIS2_PLACEMENT_3D ( 'NONE', #5526, #7353, #17733 ) ;
#8824 =( NAMED_UNIT ( * ) SI_UNIT ( $, .STERADIAN. ) SOLID_ANGLE_UNIT ( ) );
#8825 = DIRECTION ( 'NONE',  ( 0.000000000000000000, 0.000000000000000000, 1.000000000000000000 ) ) ;
#8826 = DIRECTION ( 'NONE',  ( 0.000000000000000000, 0.000000000000000000, 1.000000000000000000 ) ) ;
#8827 = CARTESIAN_POINT ( 'NONE',  ( -4.903702542908436435, 200.1653181626580249, 20.04886208192143471 ) ) ;
#8828 = CARTESIAN_POINT ( 'NONE',  ( 9.984503880673470277, 203.7031108863295401, 47.15113791807857524 ) ) ;
#8829 = CARTESIAN_POINT ( 'NONE',  ( 10.00000000000000711, 206.9523078486586201, 35.00113791807856956 ) ) ;
#8830 = CARTESIAN_POINT ( 'NONE',  ( 82.27499999726880731, 160.0630714827496206, 15.58253174999999402 ) ) ;
#8831 = PRODUCT_CONTEXT ( 'NONE', #15940, 'mechanical' ) ;
#8832 = CARTESIAN_POINT ( 'NONE',  ( 7.984503880673485376, 204.3529502787953902, -0.8488620819214343083 ) ) ;
#8833 = AXIS2_PLACEMENT_3D ( 'NONE', #4841, #5175, #2462 ) ;
#8834 = CARTESIAN_POINT ( 'NONE',  ( 46.52499999726881441, 140.1801316387863778, 4.815267126137185549 ) ) ;
#8835 = SURFACE_STYLE_FILL_AREA ( #8351 ) ;
#8836 = DIRECTION ( 'NONE',  ( -1.000000000000000000, -0.000000000000000000, -0.000000000000000000 ) ) ;
#8837 = CARTESIAN_POINT ( 'NONE',  ( -11.98450388067348804, 210.9467285061362247, 15.65113791807856636 ) ) ;
#8838 = DIRECTION ( 'NONE',  ( 0.000000000000000000, 0.000000000000000000, 1.000000000000000000 ) ) ;
#8839 = B_SPLINE_CURVE_WITH_KNOTS ( 'NONE', 3,
 ( #806, #5580, #14419, #6583, #6419, #14928, #1638, #24812, #22255, #30437, #1473, #11868, #32642, #32470, #32808, #9305, #27863, #1312 ),
 .UNSPECIFIED., .F., .F.,
 ( 4, 2, 2, 2, 2, 2, 2, 2, 4 ),
 ( 0.5000000000000000000, 0.5625000000000006661, 0.6250000000000012212, 0.6875000000000018874, 0.7500000000000024425, 0.8125000000000018874, 0.8750000000000013323, 0.9375000000000006661, 1.000000000000000000 ),
 .UNSPECIFIED. ) ;
#8840 = AXIS2_PLACEMENT_3D ( 'NONE', #18667, #5710, #20553 ) ;
#8841 = CARTESIAN_POINT ( 'NONE',  ( 10.00000000000000711, 206.9523078486586201, 62.00113791807856956 ) ) ;
#8842 = CARTESIAN_POINT ( 'NONE',  ( -3.044812012440131443, 216.5253028482142952, 43.10113791807857808 ) ) ;
#8843 = CARTESIAN_POINT ( 'NONE',  ( -7.500000000000000000, -2.571118828324945760, -0.3627527587569098766 ) ) ;
#8844 = DIRECTION ( 'NONE',  ( 0.000000000000000000, 0.000000000000000000, -1.000000000000000000 ) ) ;
#8845 = CARTESIAN_POINT ( 'NONE',  ( 7.375838497908012492, 217.2372850707501186, 6.548862081921433820 ) ) ;
#8846 = CARTESIAN_POINT ( 'NONE',  ( -0.05014649552828402690, 217.5146222423826714, 6.248862081921433997 ) ) ;
#8847 = CARTESIAN_POINT ( 'NONE',  ( 66.19999999453763451, 163.5228861582408797, -11.73074641843674470 ) ) ;
#8848 = ORIENTED_EDGE ( 'NONE', *, *, #8744, .T. ) ;
#8849 = CARTESIAN_POINT ( 'NONE',  ( 11.98450388067348271, 203.0532714938637753, 50.15113791807857524 ) ) ;
#8850 = CARTESIAN_POINT ( 'NONE',  ( 7.984503880673485376, 204.3529502787953902, 65.15113791807856103 ) ) ;
#8851 = CARTESIAN_POINT ( 'NONE',  ( 67.71132485994280614, 155.0000000000000000, -15.00000000000002487 ) ) ;
#8852 = CARTESIAN_POINT ( 'NONE',  ( 8.062137200540822946, 212.9164362838583315, 33.69886208192143329 ) ) ;
#8853 = CARTESIAN_POINT ( 'NONE',  ( 45.31132485994280756, 140.7341522555726669, -4.635254915624220651 ) ) ;
#8854 = ORIENTED_EDGE ( 'NONE', *, *, #22897, .T. ) ;
#8855 = CARTESIAN_POINT ( 'NONE',  ( 6.139770520408368348, 198.4640165459539674, 77.45113791807854398 ) ) ;
#8856 = ORIENTED_EDGE ( 'NONE', *, *, #8702, .F. ) ;
#8857 = DIRECTION ( 'NONE',  ( 0.000000000000000000, -1.000000000000000000, 6.454785026890489601E-15 ) ) ;
#8858 = DIRECTION ( 'NONE',  ( 1.000000000000000000, -0.000000000000000000, -0.000000000000000000 ) ) ;
#8859 = VERTEX_POINT ( 'NONE', #27244 ) ;
#8860 = AXIS2_PLACEMENT_3D ( 'NONE', #4439, #17049, #12275 ) ;
#8861 = CARTESIAN_POINT ( 'NONE',  ( -8.015496119326531499, 204.4483345814780364, 24.35113791807856742 ) ) ;
#8862 = VECTOR ( 'NONE', #5014, 1000.000000000000000 ) ;
#8863 = LINE ( 'NONE', #19263, #29208 ) ;
#8864 = EDGE_CURVE ( 'NONE', #8437, #28846, #11741, .T. ) ;
#8865 = CARTESIAN_POINT ( 'NONE',  ( 6.220909254589681581, 198.5229672870052582, 7.448862081921433287 ) ) ;
#8866 = CIRCLE ( 'NONE', #24117, 27.50000000000000355 ) ;
#8867 = CARTESIAN_POINT ( 'NONE',  ( 47.67499999726881299, 168.2552932293087906, -9.630534252274387086 ) ) ;
#8868 = VERTEX_POINT ( 'NONE', #9191 ) ;
#8869 = CARTESIAN_POINT ( 'NONE',  ( 57.72499999726881015, 169.8198683612136222, 4.815267126137181997 ) ) ;
#8870 = DIRECTION ( 'NONE',  ( 0.000000000000000000, 0.000000000000000000, -1.000000000000000000 ) ) ;
#8871 = CARTESIAN_POINT ( 'NONE',  ( -125.0000000000000000, 0.000000000000000000, 35.00000000000000000 ) ) ;
#8872 = CARTESIAN_POINT ( 'NONE',  ( 0.000000000000000000, 0.000000000000000000, 0.000000000000000000 ) ) ;
#8873 = CARTESIAN_POINT ( 'NONE',  ( -10.12668159690567649, 1.240160820363494356E-15, -9.226681596905677907 ) ) ;
#8874 = CARTESIAN_POINT ( 'NONE',  ( 6.220909254589681581, 198.5229672870052582, 88.44886208192144750 ) ) ;
#8875 = CARTESIAN_POINT ( 'NONE',  ( 61.57499999726881157, 164.1591823560292198, -12.60653300113719766 ) ) ;
#8876 = CARTESIAN_POINT ( 'NONE',  ( 6.220909254589536808, 215.4770327129947702, 22.55113791807856671 ) ) ;
#8877 = CYLINDRICAL_SURFACE ( 'NONE', #10544, 2.149999999999994138 ) ;
#8878 = CARTESIAN_POINT ( 'NONE',  ( -12.01549611932659722, 210.8513442034533227, 80.64886208192145034 ) ) ;
#8879 = ADVANCED_FACE ( 'NONE', ( #4238, #19581 ), #17018, .F. ) ;
#8880 = AXIS2_PLACEMENT_3D ( 'NONE', #12418, #10384, #11928 ) ;
#8881 = CARTESIAN_POINT ( 'NONE',  ( 75.00000000000000000, 170.2462022514548323, -7.872454543227099337E-15 ) ) ;
#8882 = DIRECTION ( 'NONE',  ( -0.5526942671207060176, -0.1536855300543007452, -0.8190908404712106128 ) ) ;
#8883 = PRESENTATION_LAYER_ASSIGNMENT (  '', '', ( #1832 ) ) ;
#8884 = CARTESIAN_POINT ( 'NONE',  ( -8.062137200540920645, 212.9164362838581894, 90.80113791807858092 ) ) ;
#8885 = DIRECTION ( 'NONE',  ( -1.000000000000000000, 0.000000000000000000, 0.000000000000000000 ) ) ;
#8886 = CARTESIAN_POINT ( 'NONE',  ( 45.07499999726880446, 141.7447067706911810, -9.630534252274385310 ) ) ;
#8887 = CARTESIAN_POINT ( 'NONE',  ( -3.044812012440131443, 216.5253028482142952, 37.10113791807857098 ) ) ;
#8888 = CARTESIAN_POINT ( 'NONE',  ( 75.82499999726881867, 168.2552932293087906, 9.630534252274372875 ) ) ;
#8889 = ORIENTED_EDGE ( 'NONE', *, *, #14591, .F. ) ;
#8890 = DIRECTION ( 'NONE',  ( 1.000000000000000000, 0.000000000000000000, 0.000000000000000000 ) ) ;
#8891 = CARTESIAN_POINT ( 'NONE',  ( 50.49999999453762456, 170.2462022514548323, -7.872454543227099337E-15 ) ) ;
#8892 = CARTESIAN_POINT ( 'NONE',  ( -3.662846001190052991, 218.4274158808045740, 22.10113791807856742 ) ) ;
#8893 = AXIS2_PLACEMENT_3D ( 'NONE', #4300, #22532, #15200 ) ;
#8894 = CARTESIAN_POINT ( 'NONE',  ( 40.61132485994281893, 159.8737954434936341, 14.99999999999998934 ) ) ;
#8895 = CIRCLE ( 'NONE', #17612, 37.00000000000000711 ) ;
#8896 = CARTESIAN_POINT ( 'NONE',  ( 4.000000000000000000, 3.518949890710768802, -4.770489558936219510E-15 ) ) ;
#8897 = ORIENTED_EDGE ( 'NONE', *, *, #29077, .T. ) ;
#8898 = CARTESIAN_POINT ( 'NONE',  ( -7.375838497908014268, 196.7627149292498530, 32.04886208192143471 ) ) ;
#8899 = CARTESIAN_POINT ( 'NONE',  ( 6.500000000000000000, -3.155218591052677990, -0.5622968210053915783 ) ) ;
#8900 = CARTESIAN_POINT ( 'NONE',  ( 8.118202686958039038, 212.8392687619912635, 55.70113791807857950 ) ) ;
#8901 = EDGE_CURVE ( 'NONE', #5683, #20901, #11916, .T. ) ;
#8902 = ORIENTED_EDGE ( 'NONE', *, *, #21604, .T. ) ;
#8903 =( BOUNDED_SURFACE ( )  B_SPLINE_SURFACE ( 3, 2, ( 
 ( #13637, #696, #24372 ),
 ( #11100, #19260, #21480 ),
 ( #26925, #32367, #27097 ),
 ( #6301, #11590, #32037 ),
 ( #8528, #9031, #1038 ),
 ( #18923, #5967, #16355 ) ),
 .UNSPECIFIED., .F., .F., .T. ) 
 B_SPLINE_SURFACE_WITH_KNOTS ( ( 4, 2, 4 ),
 ( 3, 3 ),
 ( 0.003190620565844225990, 0.007281897438794491043, 0.01137317431174475653 ),
 ( 0.000000000000000000, 1.000000000000000000 ),
 .UNSPECIFIED. ) 
 GEOMETRIC_REPRESENTATION_ITEM ( )  RATIONAL_B_SPLINE_SURFACE ( (
 ( 1.000000000000000000, 0.8047731410850402778, 1.000000000000000000),
 ( 1.000000000000000000, 0.8125552299156234559, 1.000000000000000000),
 ( 1.000000000000000000, 0.8191520442889865805, 1.000000000000000000),
 ( 1.000000000000000000, 0.8191520442889865805, 1.000000000000000000),
 ( 1.000000000000000000, 0.8125552299156227898, 1.000000000000000000),
 ( 1.000000000000000000, 0.8047731410850399447, 1.000000000000000000) ) ) 
 REPRESENTATION_ITEM ( '' )  SURFACE ( )  );
#8904 = CARTESIAN_POINT ( 'NONE',  ( 2.517493886309087436, 199.4062855549015865, 16.59886208192143897 ) ) ;
#8905 = CIRCLE ( 'NONE', #21964, 3.399999999999999911 ) ;
#8906 = LINE ( 'NONE', #13852, #12159 ) ;
#8907 = ORIENTED_EDGE ( 'NONE', *, *, #31439, .F. ) ;
#8908 = CARTESIAN_POINT ( 'NONE',  ( -8.015496119326597224, 209.5516654185217362, 98.64886208192146455 ) ) ;
#8909 = EDGE_CURVE ( 'NONE', #8086, #3377, #25032, .T. ) ;
#8910 = DIRECTION ( 'NONE',  ( -0.000000000000000000, -0.000000000000000000, 1.000000000000000000 ) ) ;
#8911 = CARTESIAN_POINT ( 'NONE',  ( -6.444103211791042618, 211.7408657792732356, 39.80113791807857382 ) ) ;
#8912 = DIRECTION ( 'NONE',  ( 0.000000000000000000, 0.000000000000000000, 1.000000000000000000 ) ) ;
#8913 = ORIENTED_EDGE ( 'NONE', *, *, #23263, .T. ) ;
#8914 = CARTESIAN_POINT ( 'NONE',  ( 37.32499999726881157, 164.1591823560292198, -12.60653300113719766 ) ) ;
#8915 = AXIS2_PLACEMENT_3D ( 'NONE', #4619, #9898, #1712 ) ;
#8916 = B_SPLINE_CURVE_WITH_KNOTS ( 'NONE', 3,
 ( #20772, #31505, #31168, #13107, #28615, #23166 ),
 .UNSPECIFIED., .F., .F.,
 ( 4, 2, 4 ),
 ( 0.004615310220740751271, 0.006918661718823357169, 0.009222013216905963068 ),
 .UNSPECIFIED. ) ;
#8917 = CARTESIAN_POINT ( 'NONE',  ( 6.139770520408223575, 215.5359834540460611, 63.54886208192144181 ) ) ;
#8918 = CIRCLE ( 'NONE', #3465, 0.9999999999999941158 ) ;
#8919 = CARTESIAN_POINT ( 'NONE',  ( 41.87499999726880162, 171.3844434931184253, -7.942151717890132712E-15 ) ) ;
#8920 = DIRECTION ( 'NONE',  ( 0.000000000000000000, 0.000000000000000000, -1.000000000000000000 ) ) ;
#8921 = CARTESIAN_POINT ( 'NONE',  ( -4.903702542908602524, 213.8346818373418898, 93.95113791807857240 ) ) ;
#8922 = CARTESIAN_POINT ( 'NONE',  ( 55.60000000000000853, 150.2886644046228639, 14.49999999999999645 ) ) ;
#8923 = LINE ( 'NONE', #1425, #33260 ) ;
#8924 = CARTESIAN_POINT ( 'NONE',  ( -4.903702542908436435, 200.1653181626580249, 71.04886208192142760 ) ) ;
#8925 = CARTESIAN_POINT ( 'NONE',  ( 16.00000000000000000, 0.000000000000000000, -18.00000000000000000 ) ) ;
#8926 = DIRECTION ( 'NONE',  ( 1.000000000000000000, 0.000000000000000000, 0.000000000000000000 ) ) ;
#8927 = EDGE_CURVE ( 'NONE', #18104, #10467, #20304, .T. ) ;
#8928 = CARTESIAN_POINT ( 'NONE',  ( 58.62499999726880162, 138.6155565068815463, -3.929120461958505118E-15 ) ) ;
#8929 = STYLED_ITEM ( 'NONE', ( #10899 ), #16530 ) ;
#8931 = EDGE_LOOP ( 'NONE', ( #31343, #8848, #29305 ) ) ;
#8930 = CARTESIAN_POINT ( 'NONE',  ( -0.05014649552810635652, 196.4853777576173002, 17.75113791807856245 ) ) ;
#8932 = LINE ( 'NONE', #10988, #21154 ) ;
#8933 = CARTESIAN_POINT ( 'NONE',  ( 80.07499999726879025, 168.2552932293087906, 9.630534252274372875 ) ) ;
#8934 = CARTESIAN_POINT ( 'NONE',  ( -12.01549611932652972, 203.1486557965464499, 81.35113791807857808 ) ) ;
#8935 = EDGE_CURVE ( 'NONE', #8276, #8169, #6521, .T. ) ;
#8936 = CARTESIAN_POINT ( 'NONE',  ( -0.05014649552810635652, 196.4853777576173002, 92.75113791807858377 ) ) ;
#8937 = DIRECTION ( 'NONE',  ( 0.000000000000000000, 0.000000000000000000, -1.000000000000000000 ) ) ;
#8938 = VERTEX_POINT ( 'NONE', #275 ) ;
#8939 = CARTESIAN_POINT ( 'NONE',  ( 10.01549611932659545, 203.7984951890123853, 1.148862081921433909 ) ) ;
#8940 = CARTESIAN_POINT ( 'NONE',  ( 0.05014649552828288198, 194.3824533091408000, 58.74886208192142334 ) ) ;
#8941 = CARTESIAN_POINT ( 'NONE',  ( 6.220909254589680693, 198.5229672870052582, 73.44886208192141908 ) ) ;
#8942 = CARTESIAN_POINT ( 'NONE',  ( 12.00000000000000711, 207.0476921513415220, 0.9988620819214339974 ) ) ;
#8943 = CARTESIAN_POINT ( 'NONE',  ( 103.4083388212532810, 155.0000000000000000, -32.00000000000002842 ) ) ;
#8944 = CARTESIAN_POINT ( 'NONE',  ( 9.984503880673470277, 203.7031108863295401, 26.15113791807856813 ) ) ;
#8945 = EDGE_CURVE ( 'NONE', #14561, #171, #25560, .T. ) ;
#8946 = CARTESIAN_POINT ( 'NONE',  ( -10.00000000000000711, 206.9523078486584495, 92.49886208192144466 ) ) ;
#8947 = ORIENTED_EDGE ( 'NONE', *, *, #12286, .T. ) ;
#8948 = DIRECTION ( 'NONE',  ( 0.000000000000000000, 0.000000000000000000, -1.000000000000000000 ) ) ;
#8949 = VERTEX_POINT ( 'NONE', #4411 ) ;
#8950 = DIRECTION ( 'NONE',  ( 0.5000000000000008882, 0.8660254037844382635, -0.000000000000000000 ) ) ;
#8951 = CARTESIAN_POINT ( 'NONE',  ( -0.05014649552828365914, 215.4116977939061144, 69.24886208192143044 ) ) ;
#8952 = VERTEX_POINT ( 'NONE', #30655 ) ;
#8953 = CARTESIAN_POINT ( 'NONE',  ( 82.12499999726881583, 155.0000000000000000, 15.58253174999999402 ) ) ;
#8954 = VERTEX_POINT ( 'NONE', #9693 ) ;
#8955 = FACE_OUTER_BOUND ( 'NONE', #26055, .T. ) ;
#8956 = CARTESIAN_POINT ( 'NONE',  ( 75.12499999726881583, 155.0000000000000000, -15.58253175000000823 ) ) ;
#8957 = CARTESIAN_POINT ( 'NONE',  ( -6.500168698208129925, 202.3363017425936050, 72.20113791807857240 ) ) ;
#8958 = CARTESIAN_POINT ( 'NONE',  ( 75.48867513459482836, 167.7597621252805880, 9.270509831248428867 ) ) ;
#8959 =( LENGTH_UNIT ( ) NAMED_UNIT ( * ) SI_UNIT ( .MILLI., .METRE. ) );
#8960 = CARTESIAN_POINT ( 'NONE',  ( 38.00000000000000711, 139.7537977485451393, -4.138211985947621020E-15 ) ) ;
#8961 = CARTESIAN_POINT ( 'NONE',  ( 4.903702542908435547, 213.8346818373419751, 39.54886208192143471 ) ) ;
#8962 = CARTESIAN_POINT ( 'NONE',  ( 6.220909254589536808, 215.4770327129947702, 85.55113791807858092 ) ) ;
#8963 = EDGE_CURVE ( 'NONE', #610, #9889, #22635, .T. ) ;
#8964 = CARTESIAN_POINT ( 'NONE',  ( -3.044812012440131443, 216.5253028482142952, 64.10113791807857808 ) ) ;
#8965 = EDGE_CURVE ( 'NONE', #30277, #31940, #3789, .T. ) ;
#8966 = FACE_OUTER_BOUND ( 'NONE', #11004, .T. ) ;
#8967 = FACE_OUTER_BOUND ( 'NONE', #11646, .T. ) ;
#8968 = CYLINDRICAL_SURFACE ( 'NONE', #15876, 15.00000000000001776 ) ;
#8969 = CARTESIAN_POINT ( 'NONE',  ( 52.12499999726881583, 155.0000000000000000, 15.58253174999999402 ) ) ;
#8970 = CARTESIAN_POINT ( 'NONE',  ( 3.662846001190051659, 195.5725841191953691, 44.60113791807857098 ) ) ;
#8971 = CARTESIAN_POINT ( 'NONE',  ( 107.9108275708642850, 155.0000000000000000, -13.00000000000001066 ) ) ;
#8972 = ADVANCED_FACE ( 'NONE', ( #15930 ), #23924, .T. ) ;
#8973 = PRODUCT_RELATED_PRODUCT_CATEGORY ( 'part', '', ( #14870 ) ) ;
#8974 = CARTESIAN_POINT ( 'NONE',  ( -8.118202686958039038, 201.1607312380087080, 96.20113791807857240 ) ) ;
#8975 = EDGE_CURVE ( 'NONE', #33178, #33078, #4882, .T. ) ;
#8977 = CARTESIAN_POINT ( 'NONE',  ( -6.139770520408368348, 215.5359834540460042, 69.95113791807858661 ) ) ;
#8976 = APPLICATION_CONTEXT ( 'automotive_design' ) ;
#8978 = CARTESIAN_POINT ( 'NONE',  ( 7.456977232089471386, 196.8216656703012006, 37.44886208192143329 ) ) ;
#8979 = CARTESIAN_POINT ( 'NONE',  ( -0.05014649552828402690, 217.5146222423826714, 42.24886208192143044 ) ) ;
#8980 = CARTESIAN_POINT ( 'NONE',  ( 86.29999999453764303, 167.3344367211045096, -8.961492836873482304 ) ) ;
#8981 = CARTESIAN_POINT ( 'NONE',  ( -9.680171189290831535, 214.0920067884431148, 75.80113791807858092 ) ) ;
#8982 = CARTESIAN_POINT ( 'NONE',  ( 0.05014649552807626948, 215.4116977939061144, 97.25113791807856956 ) ) ;
#8983 = CARTESIAN_POINT ( 'NONE',  ( -6.220909254589682469, 215.4770327129946850, 62.94886208192143329 ) ) ;
#8984 = CARTESIAN_POINT ( 'NONE',  ( 5.000000000000000000, 4.685197434473814759, -5.637851296924623057E-15 ) ) ;
#8985 = ORIENTED_EDGE ( 'NONE', *, *, #18490, .F. ) ;
#8986 = CARTESIAN_POINT ( 'NONE',  ( 7.456977232089471386, 196.8216656703012006, 58.44886208192144039 ) ) ;
#8987 = ORIENTED_EDGE ( 'NONE', *, *, #27471, .T. ) ;
#8988 = CARTESIAN_POINT ( 'NONE',  ( 74.07499999726880446, 168.2552932293087906, 9.630534252274372875 ) ) ;
#8989 = CARTESIAN_POINT ( 'NONE',  ( -6.444103211790928043, 202.2591342207265939, 44.19886208192144750 ) ) ;
#8990 = VERTEX_POINT ( 'NONE', #15140 ) ;
#8991 = CARTESIAN_POINT ( 'NONE',  ( 85.37499999726881583, 155.0000000000000000, -15.58253175000000823 ) ) ;
#8992 = CARTESIAN_POINT ( 'NONE',  ( -47.49999999999998579, 155.0000000000000000, -6.938893903907228378E-15 ) ) ;
#8993 = DIRECTION ( 'NONE',  ( -0.000000000000000000, -0.000000000000000000, 1.000000000000000000 ) ) ;
#8994 = CARTESIAN_POINT ( 'NONE',  ( -4.984841277089726574, 200.2242689037092305, 48.05113791807858092 ) ) ;
#8995 = CARTESIAN_POINT ( 'NONE',  ( 89.50000000000002842, 155.0000000000000000, -32.00000000000002842 ) ) ;
#8996 = CARTESIAN_POINT ( 'NONE',  ( -0.05014649552828403384, 217.5146222423826714, 30.24886208192142689 ) ) ;
#8997 = CARTESIAN_POINT ( 'NONE',  ( 67.27499999726879309, 149.9369285172503510, -15.58253175000000823 ) ) ;
#8998 = ORIENTED_EDGE ( 'NONE', *, *, #2109, .T. ) ;
#8999 = CARTESIAN_POINT ( 'NONE',  ( 117.5000000000000000, 246.7986928011511907, 52.99999999999882760 ) ) ;
#9000 = LINE ( 'NONE', #378, #33555 ) ;
#9001 = FACE_OUTER_BOUND ( 'NONE', #10282, .T. ) ;
#9002 = CARTESIAN_POINT ( 'NONE',  ( -2.426778023690076225, 199.3768101843759553, 19.89886208192143613 ) ) ;
#9003 = CARTESIAN_POINT ( 'NONE',  ( 10.00000000000000711, 206.9523078486586201, 59.00113791807857666 ) ) ;
#9004 = PRODUCT_DEFINITION_SHAPE ( 'NONE', 'NONE',  #33709 ) ;
#9005 = CARTESIAN_POINT ( 'NONE',  ( 9.984503880673470277, 203.7031108863295401, 38.15113791807856813 ) ) ;
#9006 = CARTESIAN_POINT ( 'NONE',  ( 38.21132485994280614, 170.7719333635740497, -7.904646289410545231E-15 ) ) ;
#9007 = ITEM_DEFINED_TRANSFORMATION ( 'NONE', 'NONE', #139,  #2404 ) ;
#9008 = CARTESIAN_POINT ( 'NONE',  ( -2.517493886308901807, 199.4062855549015012, -0.09886208192143407236 ) ) ;
#9009 = CARTESIAN_POINT ( 'NONE',  ( 47.72499999726881015, 169.8198683612136222, 4.815267126137181997 ) ) ;
#9010 = CARTESIAN_POINT ( 'NONE',  ( -6.830473686658677934E-14, -4.041451884327390331, -2.587392608830344720 ) ) ;
#9011 = CARTESIAN_POINT ( 'NONE',  ( 33.82499999726880446, 168.2552932293087906, 9.630534252274372875 ) ) ;
#9012 = CARTESIAN_POINT ( 'NONE',  ( -9.736236675707914401, 199.9851607334237542, 18.20113791807856529 ) ) ;
#9013 = CARTESIAN_POINT ( 'NONE',  ( 82.68867513459481700, 150.1262045565064795, -15.00000000000009592 ) ) ;
#9014 = CARTESIAN_POINT ( 'NONE',  ( -3.135527875058821579, 197.5041725223112223, 65.90113791807857524 ) ) ;
#9015 = CARTESIAN_POINT ( 'NONE',  ( 0.05014649552810506589, 217.5146222423826714, 40.25113791807856956 ) ) ;
#9016 = ADVANCED_FACE ( 'NONE', ( #26001 ), #20889, .F. ) ;
#9017 = CARTESIAN_POINT ( 'NONE',  ( -64.50000000000000000, 2.605762844159070557, -20.00000000000000000 ) ) ;
#9018 = CARTESIAN_POINT ( 'NONE',  ( 0.000000000000000000, 0.000000000000000000, 2.066666666666666430 ) ) ;
#9019 = CARTESIAN_POINT ( 'NONE',  ( -7.456977232089304408, 196.8216656703010301, 102.0511379180785809 ) ) ;
#9020 = CARTESIAN_POINT ( 'NONE',  ( -8.062137200540822946, 201.0835637161416400, 5.198862081921435063 ) ) ;
#9021 = CARTESIAN_POINT ( 'NONE',  ( 68.79999999453762882, 163.5228861582408797, 11.73074641843673049 ) ) ;
#9022 = EDGE_LOOP ( 'NONE', ( #26538, #12636, #11622, #20941 ) ) ;
#9023 = CARTESIAN_POINT ( 'NONE',  ( 3.662846001190051659, 195.5725841191953691, 44.60113791807857098 ) ) ;
#9024 = CARTESIAN_POINT ( 'NONE',  ( 8.015496119326531499, 209.5516654185219636, 70.85113791807857808 ) ) ;
#9025 = CARTESIAN_POINT ( 'NONE',  ( 10.00000000000000711, 207.0476921513415220, 30.99886208192143755 ) ) ;
#9026 = LINE ( 'NONE', #19415, #5801 ) ;
#9027 = VERTEX_POINT ( 'NONE', #25190 ) ;
#9028 = CARTESIAN_POINT ( 'NONE',  ( 3.135527875058820690, 216.4958274776887492, 79.40113791807857524 ) ) ;
#9029 = ORIENTED_EDGE ( 'NONE', *, *, #23556, .T. ) ;
#9030 = CARTESIAN_POINT ( 'NONE',  ( 87.49999999999995737, 164.4872682688857708, -12.40341692595884027 ) ) ;
#9031 = CARTESIAN_POINT ( 'NONE',  ( -0.9108756637647318355, -6.979659189790606177, -6.219623095965800097 ) ) ;
#9032 = VERTEX_POINT ( 'NONE', #7948 ) ;
#9033 = CARTESIAN_POINT ( 'NONE',  ( -6.444103211791042618, 211.7408657792732356, 21.80113791807856671 ) ) ;
#9034 = CARTESIAN_POINT ( 'NONE',  ( -58.82767890163440683, 194.9228235633793815, 2.483781759962022218 ) ) ;
#9035 = CARTESIAN_POINT ( 'NONE',  ( -7.375838497908014268, 196.7627149292498530, 104.0488620819214560 ) ) ;
#9036 = CARTESIAN_POINT ( 'NONE',  ( 52.47499999726881015, 149.9369285172503510, 15.58253174999999580 ) ) ;
#9037 = ORIENTED_EDGE ( 'NONE', *, *, #629, .F. ) ;
#9038 = CARTESIAN_POINT ( 'NONE',  ( 57.82499999726879736, 168.2552932293087906, 9.630534252274372875 ) ) ;
#9039 = CARTESIAN_POINT ( 'NONE',  ( 4.903702542908601636, 200.1653181626581102, 47.45113791807857950 ) ) ;
#9040 = DIRECTION ( 'NONE',  ( 1.000000000000000000, 0.000000000000000000, 0.000000000000000000 ) ) ;
#9041 = CARTESIAN_POINT ( 'NONE',  ( 117.5000000000000142, 155.0000000000000000, -6.938893903907228378E-15 ) ) ;
#9042 = CARTESIAN_POINT ( 'NONE',  ( 6.220909254589681581, 198.5229672870052582, 94.44886208192140487 ) ) ;
#9043 = CARTESIAN_POINT ( 'NONE',  ( 63.07499999726881867, 141.7447067706911810, -9.630534252274385310 ) ) ;
#9044 = CARTESIAN_POINT ( 'NONE',  ( 9.984503880673470277, 203.7031108863295401, 29.15113791807856103 ) ) ;
#9045 = CARTESIAN_POINT ( 'NONE',  ( 46.98867513459482836, 163.8167787843871110, -12.13525491562423397 ) ) ;
#9046 = CARTESIAN_POINT ( 'NONE',  ( -9.680171189290716072, 199.9079932115567146, 80.19886208192143329 ) ) ;
#9047 = AXIS2_PLACEMENT_3D ( 'NONE', #7544, #17576, #203 ) ;
#9048 = CARTESIAN_POINT ( 'NONE',  ( 82.79999999999999716, 167.3344367211045096, -8.961492836873482304 ) ) ;
#9049 = CARTESIAN_POINT ( 'NONE',  ( 39.88867513459481984, 150.1262045565064227, 15.00000000000001599 ) ) ;
#9050 = CARTESIAN_POINT ( 'NONE',  ( 98.19869130599479945, 155.0000000000000000, 0.000000000000000000 ) ) ;
#9051 = CARTESIAN_POINT ( 'NONE',  ( 9.984503880673470277, 203.7031108863295401, 98.15113791807858945 ) ) ;
#9052 = FACE_OUTER_BOUND ( 'NONE', #21969, .T. ) ;
#9053 = CARTESIAN_POINT ( 'NONE',  ( 43.67499999726881299, 168.2552932293087906, -9.630534252274385310 ) ) ;
#9054 = CARTESIAN_POINT ( 'NONE',  ( -10.01549611932653860, 203.7984951890123284, 36.35113791807857098 ) ) ;
#9055 = CARTESIAN_POINT ( 'NONE',  ( 83.32499999726880446, 164.1591823560292198, -12.60653300113719766 ) ) ;
#9056 = EDGE_LOOP ( 'NONE', ( #32117, #30050 ) ) ;
#9057 = CARTESIAN_POINT ( 'NONE',  ( 10.00000000000000178, 8.000000000000000000, 0.000000000000000000 ) ) ;
#9058 = CARTESIAN_POINT ( 'NONE',  ( -64.50000000000000000, 0.000000000000000000, -20.00000000000000000 ) ) ;
#9059 = CARTESIAN_POINT ( 'NONE',  ( 48.69999999453762030, 167.3344367211045096, 8.961492836873468093 ) ) ;
#9060 = CARTESIAN_POINT ( 'NONE',  ( -3.753561863808691168, 195.6020594897209435, 17.90113791807856458 ) ) ;
#9061 = LINE ( 'NONE', #32909, #18707 ) ;
#9062 = EDGE_CURVE ( 'NONE', #19467, #29217, #28824, .T. ) ;
#9063 = DIRECTION ( 'NONE',  ( 1.000000000000000000, 0.000000000000000000, 0.000000000000000000 ) ) ;
#9064 = ORIENTED_EDGE ( 'NONE', *, *, #12679, .F. ) ;
#9065 = CARTESIAN_POINT ( 'NONE',  ( 7.375838497908012492, 217.2372850707501186, 45.54886208192143471 ) ) ;
#9066 = CARTESIAN_POINT ( 'NONE',  ( -0.05014649552810635652, 196.4853777576173002, 5.751137918078563338 ) ) ;
#9067 = CARTESIAN_POINT ( 'NONE',  ( -9.984503880673473830, 210.2968891136704315, 51.65113791807855392 ) ) ;
#9068 = CARTESIAN_POINT ( 'NONE',  ( -2.517493886309087880, 214.5937144450984135, 12.09886208192143364 ) ) ;
#9069 = CIRCLE ( 'NONE', #28119, 15.50000000000001066 ) ;
#9070 = PRODUCT_DEFINITION_CONTEXT ( 'detailed design', #31616, 'design' ) ;
#9071 = CARTESIAN_POINT ( 'NONE',  ( -16.08713178458081572, -22.46635493911272619, -17.92845254598169547 ) ) ;
#9072 = VERTEX_POINT ( 'NONE', #15767 ) ;
#9073 = CARTESIAN_POINT ( 'NONE',  ( 6.444103211790928043, 211.7408657792734061, 96.69886208192144750 ) ) ;
#9074 = DIRECTION ( 'NONE',  ( 1.000000000000000000, 0.000000000000000000, 0.000000000000000000 ) ) ;
#9075 = CARTESIAN_POINT ( 'NONE',  ( -2.517493886308901807, 199.4062855549015012, 44.90113791807856813 ) ) ;
#9076 = DIRECTION ( 'NONE',  ( 0.000000000000000000, 0.000000000000000000, -1.000000000000000000 ) ) ;
#9078 = ORIENTED_EDGE ( 'NONE', *, *, #33526, .F. ) ;
#9077 = CIRCLE ( 'NONE', #11805, 4.400000000000001243 ) ;
#9079 = CARTESIAN_POINT ( 'NONE',  ( 39.12499999726880873, 155.0000000000000000, -15.58253175000000823 ) ) ;
#9080 = DIRECTION ( 'NONE',  ( 0.000000000000000000, 0.9988620819214357738, 0.04769215134144196705 ) ) ;
#9081 = CARTESIAN_POINT ( 'NONE',  ( -8.118202686958138514, 212.8392687619910930, 59.79886208192143471 ) ) ;
#9082 = CARTESIAN_POINT ( 'NONE',  ( 43.47499999726881015, 160.0630714827496206, -15.58253175000000823 ) ) ;
#9083 = FACE_OUTER_BOUND ( 'NONE', #24775, .T. ) ;
#9084 = CARTESIAN_POINT ( 'NONE',  ( -6.444103211791042618, 211.7408657792732356, 99.80113791807858092 ) ) ;
#9085 = CARTESIAN_POINT ( 'NONE',  ( 58.59999999999999432, 159.7113355953771077, -14.50000000000000888 ) ) ;
#9086 = DIRECTION ( 'NONE',  ( 0.000000000000000000, -0.7071067811865411334, 0.7071067811865540120 ) ) ;
#9087 = CARTESIAN_POINT ( 'NONE',  ( 8.015496119326595448, 204.4483345814782638, 85.14886208192143613 ) ) ;
#9088 = AXIS2_PLACEMENT_3D ( 'NONE', #10941, #21317, #1203 ) ;
#9089 = DIRECTION ( 'NONE',  ( 0.000000000000000000, 0.000000000000000000, -1.000000000000000000 ) ) ;
#9090 = EDGE_CURVE ( 'NONE', #23420, #20358, #22693, .T. ) ;
#9091 = CARTESIAN_POINT ( 'NONE',  ( 115.4999999999999858, 255.8678580070898363, -25.91453920131762345 ) ) ;
#9092 = CARTESIAN_POINT ( 'NONE',  ( 56.82499999726880446, 141.7447067706911810, -9.630534252274385310 ) ) ;
#9093 = VECTOR ( 'NONE', #22792, 1000.000000000000114 ) ;
#9095 = ORIENTED_EDGE ( 'NONE', *, *, #157, .F. ) ;
#9094 = CARTESIAN_POINT ( 'NONE',  ( -0.05014649552810635652, 196.4853777576173002, 20.75113791807856245 ) ) ;
#9096 = CARTESIAN_POINT ( 'NONE',  ( -13.16654248868335841, 24.15255795529145288, 2.021585300780266894E-15 ) ) ;
#9097 = CARTESIAN_POINT ( 'NONE',  ( 81.77499999726880731, 169.8198683612136222, -4.815267126137197984 ) ) ;
#9098 = CARTESIAN_POINT ( 'NONE',  ( 7.456977232089302632, 217.1783343296989131, 88.55113791807858092 ) ) ;
#9099 = CARTESIAN_POINT ( 'NONE',  ( 117.5000000000000000, 155.0000000000000000, -6.938893903907228378E-15 ) ) ;
#9100 = ADVANCED_FACE ( 'NONE', ( #31929 ), #5868, .T. ) ;
#9101 = CARTESIAN_POINT ( 'NONE',  ( 60.63708498984762940, 155.0000000000000000, 6.938893903907228378E-15 ) ) ;
#9102 = VECTOR ( 'NONE', #3639, 1000.000000000000000 ) ;
#9103 = EDGE_LOOP ( 'NONE', ( #31565, #15573, #22061, #31165, #11509, #17342 ) ) ;
#9104 = CARTESIAN_POINT ( 'NONE',  ( 7.375838497908012492, 217.2372850707501186, 72.54886208192141339 ) ) ;
#9105 = CARTESIAN_POINT ( 'NONE',  ( -8.118202686958138514, 212.8392687619910930, 80.79886208192144181 ) ) ;
#9106 = CARTESIAN_POINT ( 'NONE',  ( -9.680171189290716072, 199.9079932115567146, 11.19886208192143506 ) ) ;
#9107 = CARTESIAN_POINT ( 'NONE',  ( 2.000000000000000000, -1.773042676681340524, 1.734723475976807094E-15 ) ) ;
#9108 = CARTESIAN_POINT ( 'NONE',  ( -6.220909254589537696, 198.5229672870051161, 21.05113791807855961 ) ) ;
#9109 = CARTESIAN_POINT ( 'NONE',  ( -8.062137200540822946, 201.0835637161416400, 86.19886208192144750 ) ) ;
#9110 = VERTEX_POINT ( 'NONE', #3316 ) ;
#9111 = EDGE_CURVE ( 'NONE', #12301, #12567, #31769, .T. ) ;
#9112 = FACE_BOUND ( 'NONE', #18515, .T. ) ;
#9113 = VERTEX_POINT ( 'NONE', #14214 ) ;
#9114 = PLANE ( 'NONE',  #5309 ) ;
#9115 = CARTESIAN_POINT ( 'NONE',  ( -8.015496119326597224, 209.5516654185217362, 68.64886208192142192 ) ) ;
#9116 = CONICAL_SURFACE ( 'NONE', #21639, 27.50000000000000355, 1.047197551196595411 ) ;
#9117 = ORIENTED_EDGE ( 'NONE', *, *, #30631, .F. ) ;
#9118 = AXIS2_PLACEMENT_3D ( 'NONE', #21479, #3582, #8857 ) ;
#9119 = CARTESIAN_POINT ( 'NONE',  ( 83.42499999726882720, 168.2552932293087906, -9.630534252274387086 ) ) ;
#9120 = ORIENTED_EDGE ( 'NONE', *, *, #26148, .F. ) ;
#9121 = DIRECTION ( 'NONE',  ( 1.000000000000000000, 0.000000000000000000, 0.000000000000000000 ) ) ;
#9122 = CARTESIAN_POINT ( 'NONE',  ( 77.92499999726881299, 164.1591823560292198, 12.60653300113718167 ) ) ;
#9123 = ADVANCED_FACE ( 'NONE', ( #3650 ), #1482, .F. ) ;
#9124 = FACE_OUTER_BOUND ( 'NONE', #9056, .T. ) ;
#9125 = CARTESIAN_POINT ( 'NONE',  ( 2.426778023690261410, 199.3768101843759837, 65.60113791807857808 ) ) ;
#9126 = CARTESIAN_POINT ( 'NONE',  ( -65.24999999999998579, -6.704941225331758039E-15, 20.00000000000000000 ) ) ;
#9127 = AXIS2_PLACEMENT_3D ( 'NONE', #21290, #6282, #13617 ) ;
#9128 = CARTESIAN_POINT ( 'NONE',  ( 37.20000000000000995, 167.3344367211045096, 8.961492836873468093 ) ) ;
#9129 = CARTESIAN_POINT ( 'NONE',  ( 7.984503880673422316, 209.6470497212048372, 54.84886208192144608 ) ) ;
#9130 = EDGE_CURVE ( 'NONE', #13603, #11012, #25309, .T. ) ;
#9131 = CARTESIAN_POINT ( 'NONE',  ( -10.01549611932653860, 203.7984951890123284, 75.35113791807853545 ) ) ;
#9132 = FACE_OUTER_BOUND ( 'NONE', #1078, .T. ) ;
#9133 = LINE ( 'NONE', #27524, #15152 ) ;
#9134 = CARTESIAN_POINT ( 'NONE',  ( 97.20416941062678973, 155.0000000000000000, 32.00000000000000000 ) ) ;
#9135 = CARTESIAN_POINT ( 'NONE',  ( 53.12499999726881583, 155.0000000000000000, -15.58253175000000823 ) ) ;
#9136 =( BOUNDED_CURVE ( )  B_SPLINE_CURVE ( 3, ( #12246, #32352, #19745, #9017 ),
 .UNSPECIFIED., .F., .T. ) 
 B_SPLINE_CURVE_WITH_KNOTS ( ( 4, 4 ),
 ( 3.141592653589793116, 3.666471587091465700 ),
 .UNSPECIFIED. ) 
 CURVE ( )  GEOMETRIC_REPRESENTATION_ITEM ( )  RATIONAL_B_SPLINE_CURVE ( ( 1.000000000000000000, 0.9771733092046011038, 0.9771733092046011038, 1.000000000000000000 ) ) 
 REPRESENTATION_ITEM ( '' )  );
#9137 = CARTESIAN_POINT ( 'NONE',  ( 12.01549611932652972, 210.8513442034534933, 61.85113791807857098 ) ) ;
#9138 = DIRECTION ( 'NONE',  ( -1.000000000000000000, -0.000000000000000000, 0.000000000000000000 ) ) ;
#9139 = CONICAL_SURFACE ( 'NONE', #8607, 2.000000000000000000, 0.9599310885968733720 ) ;
#9140 = CARTESIAN_POINT ( 'NONE',  ( -12.01549611932652972, 203.1486557965464499, 3.351137918078566091 ) ) ;
#9141 = CARTESIAN_POINT ( 'NONE',  ( -3.044812012440131443, 216.5253028482142952, 67.10113791807857808 ) ) ;
#9142 = AXIS2_PLACEMENT_3D ( 'NONE', #27179, #14226, #32115 ) ;
#9143 = CARTESIAN_POINT ( 'NONE',  ( -3.662846001189865142, 195.5725841191952838, 34.89886208192143613 ) ) ;
#9144 = CARTESIAN_POINT ( 'NONE',  ( -6.139770520408224463, 198.4640165459539105, 47.04886208192143471 ) ) ;
#9145 = CARTESIAN_POINT ( 'NONE',  ( 86.09999999453764019, 159.7113355953771077, -14.50000000000000888 ) ) ;
#9146 = CARTESIAN_POINT ( 'NONE',  ( -0.05014649552807705357, 194.3824533091408000, 86.75113791807856956 ) ) ;
#9147 = CARTESIAN_POINT ( 'NONE',  ( -0.05014649552807731031, 198.5883022060938572, 101.7511379180785696 ) ) ;
#9148 = CARTESIAN_POINT ( 'NONE',  ( -3.135527875058982783, 216.4958274776886924, 60.09886208192143897 ) ) ;
#9149 = PRESENTATION_STYLE_ASSIGNMENT (( #26873 ) ) ;
#9150 = AXIS2_PLACEMENT_3D ( 'NONE', #10047, #7481, #28263 ) ;
#9151 = VERTEX_POINT ( 'NONE', #16768 ) ;
#9152 = CARTESIAN_POINT ( 'NONE',  ( -9.736236675708031640, 214.0148392665760753, 65.79886208192144181 ) ) ;
#9153 = ORIENTED_EDGE ( 'NONE', *, *, #12373, .F. ) ;
#9154 = CARTESIAN_POINT ( 'NONE',  ( 71.27499999726880731, 149.9369285172503510, -15.58253175000000823 ) ) ;
#9155 = CARTESIAN_POINT ( 'NONE',  ( 4.984841277089891776, 200.2242689037093726, 46.44886208192144039 ) ) ;
#9156 = EDGE_LOOP ( 'NONE', ( #8202, #28007, #19707, #25965 ) ) ;
#9157 = EDGE_CURVE ( 'NONE', #7334, #7505, #31945, .T. ) ;
#9158 = EDGE_CURVE ( 'NONE', #546, #10473, #8015, .T. ) ;
#9159 = CARTESIAN_POINT ( 'NONE',  ( 83.17499999726882720, 145.8408176439707802, -12.60653300113719588 ) ) ;
#9160 = CARTESIAN_POINT ( 'NONE',  ( 4.102348501002488490, 207.3577873115561943, -8.835681806194324750 ) ) ;
#9161 = CARTESIAN_POINT ( 'NONE',  ( 0.000000000000000000, 0.000000000000000000, -6.800000000000000711 ) ) ;
#9162 = CARTESIAN_POINT ( 'NONE',  ( 4.903702542908601636, 200.1653181626581102, 59.45113791807857240 ) ) ;
#9163 = CONICAL_SURFACE ( 'NONE', #30409, 4.057500000000000107, 1.047197551196593857 ) ;
#9164 = ADVANCED_FACE ( 'NONE', ( #18822 ), #11498, .F. ) ;
#9165 = CARTESIAN_POINT ( 'NONE',  ( 125.5000000000000000, 231.4735983853260279, 73.43303922622204993 ) ) ;
#9166 = AXIS2_PLACEMENT_3D ( 'NONE', #23125, #18186, #28240 ) ;
#9167 = CARTESIAN_POINT ( 'NONE',  ( -10.00000000000000711, 206.9523078486584495, 41.49886208192143044 ) ) ;
#9168 = CARTESIAN_POINT ( 'NONE',  ( 72.07499999726879025, 168.2552932293087906, 9.630534252274372875 ) ) ;
#9169 = ORIENTED_EDGE ( 'NONE', *, *, #12946, .F. ) ;
#9170 = DIRECTION ( 'NONE',  ( 0.000000000000000000, 0.000000000000000000, 1.000000000000000000 ) ) ;
#9171 = VECTOR ( 'NONE', #27945, 1000.000000000000000 ) ;
#9172 =( NAMED_UNIT ( * ) SI_UNIT ( $, .STERADIAN. ) SOLID_ANGLE_UNIT ( ) );
#9173 = DIRECTION ( 'NONE',  ( -1.000000000000000000, -0.000000000000000000, -0.000000000000000000 ) ) ;
#9174 = CARTESIAN_POINT ( 'NONE',  ( 92.60208470531341618, 155.0000000000000000, 0.000000000000000000 ) ) ;
#9175 = CARTESIAN_POINT ( 'NONE',  ( 4.903702542908435547, 213.8346818373419751, 18.54886208192143116 ) ) ;
#9176 = EDGE_CURVE ( 'NONE', #20223, #258, #27589, .T. ) ;
#9177 = CARTESIAN_POINT ( 'NONE',  ( -10.01549611932653860, 203.7984951890123284, 63.35113791807857098 ) ) ;
#9178 = CARTESIAN_POINT ( 'NONE',  ( -10.01549611932653860, 203.7984951890123284, 45.35113791807857808 ) ) ;
#9179 = DIRECTION ( 'NONE',  ( -1.000000000000000000, -0.000000000000000000, -0.000000000000000000 ) ) ;
#9180 = AXIS2_PLACEMENT_3D ( 'NONE', #15675, #12959, #30856 ) ;
#9181 = CARTESIAN_POINT ( 'NONE',  ( 3.044812012440130555, 197.4746971517856764, 17.60113791807856742 ) ) ;
#9182 = CARTESIAN_POINT ( 'NONE',  ( 6.444103211790928043, 211.7408657792734061, 102.6988620819214475 ) ) ;
#9183 = CARTESIAN_POINT ( 'NONE',  ( 46.22499999726880304, 149.9369285172503510, 15.58253174999999580 ) ) ;
#9184 = FACE_BOUND ( 'NONE', #11465, .T. ) ;
#9185 = CARTESIAN_POINT ( 'NONE',  ( 125.0000000000000000, 4.592425496802574367E-14, -20.00000000000000000 ) ) ;
#9186 = CARTESIAN_POINT ( 'NONE',  ( -7.456977232089304408, 196.8216656703010301, 15.05113791807856849 ) ) ;
#9187 = CARTESIAN_POINT ( 'NONE',  ( 115.4999999999999858, 155.0000000000000000, 49.99999999999999289 ) ) ;
#9188 = CARTESIAN_POINT ( 'NONE',  ( 3.044812012440130555, 197.4746971517856764, 77.60113791807857808 ) ) ;
#9189 = CARTESIAN_POINT ( 'NONE',  ( -10.01549611932653860, 203.7984951890123000, 42.35113791807857098 ) ) ;
#9190 = CARTESIAN_POINT ( 'NONE',  ( -31.74999999999995737, 0.000000000000000000, 4.000000000000000888 ) ) ;
#9191 = CARTESIAN_POINT ( 'NONE',  ( 46.71132485994281325, 155.0000000000000000, 15.00000000000001243 ) ) ;
#9192 = CARTESIAN_POINT ( 'NONE',  ( -12.01549611932659722, 210.8513442034533227, 8.648862081921436129 ) ) ;
#9193 = CARTESIAN_POINT ( 'NONE',  ( -8.118202686958138514, 212.8392687619910930, 20.79886208192143471 ) ) ;
#9194 = CARTESIAN_POINT ( 'NONE',  ( 66.49999999453763166, 170.2462022514548323, -7.872454543227099337E-15 ) ) ;
#9195 = EDGE_LOOP ( 'NONE', ( #31710, #14568, #11514, #12815 ) ) ;
#9196 = CARTESIAN_POINT ( 'NONE',  ( 12.00000000000000711, 206.9523078486586485, 47.00113791807856956 ) ) ;
#9197 = AXIS2_PLACEMENT_3D ( 'NONE', #17272, #9604, #27661 ) ;
#9198 = CARTESIAN_POINT ( 'NONE',  ( 4.984841277089725686, 213.7757310962907411, 73.55113791807856671 ) ) ;
#9199 = CARTESIAN_POINT ( 'NONE',  ( -6.220909254589682469, 215.4770327129946850, 32.94886208192144039 ) ) ;
#9200 = CARTESIAN_POINT ( 'NONE',  ( 75.91132485994280898, 163.8167787843871110, -12.13525491562423397 ) ) ;
#9201 = ORIENTED_EDGE ( 'NONE', *, *, #21789, .T. ) ;
#9202 = AXIS2_PLACEMENT_3D ( 'NONE', #14484, #24884, #1545 ) ;
#9203 = CARTESIAN_POINT ( 'NONE',  ( 77.59999999453762598, 141.2096805137202580, -4.480746418436742040 ) ) ;
#9204 = CARTESIAN_POINT ( 'NONE',  ( -10.00000000000000711, 207.0476921513413515, 93.50113791807858377 ) ) ;
#9205 = EDGE_LOOP ( 'NONE', ( #19411, #7032, #13803 ) ) ;
#9206 = AXIS2_PLACEMENT_3D ( 'NONE', #6536, #17428, #3809 ) ;
#9207 = CARTESIAN_POINT ( 'NONE',  ( 125.5000000000000000, 48.99999999999998579, -1.387778780781445676E-14 ) ) ;
#9208 = DIRECTION ( 'NONE',  ( 1.000000000000000000, 0.000000000000000000, 0.000000000000000000 ) ) ;
#9209 = ORIENTED_EDGE ( 'NONE', *, *, #16055, .F. ) ;
#9210 = CARTESIAN_POINT ( 'NONE',  ( 6.500168698208129925, 211.6636982574063381, 19.70113791807856884 ) ) ;
#9211 = CARTESIAN_POINT ( 'NONE',  ( 0.000000000000000000, 0.000000000000000000, 0.000000000000000000 ) ) ;
#9212 = CARTESIAN_POINT ( 'NONE',  ( 0.05014649552828275708, 196.4853777576173002, 7.748862081921435774 ) ) ;
#9213 = CARTESIAN_POINT ( 'NONE',  ( 51.27499999726880731, 149.9369285172503510, -15.58253175000000823 ) ) ;
#9214 = ORIENTED_EDGE ( 'NONE', *, *, #29256, .T. ) ;
#9215 = CARTESIAN_POINT ( 'NONE',  ( 7.984503880673485376, 204.3529502787953902, 53.15113791807857524 ) ) ;
#9216 = LINE ( 'NONE', #17385, #394 ) ;
#9217 = CARTESIAN_POINT ( 'NONE',  ( -18.40606158072672827, 21.12752019707600581, -0.2340887491524386022 ) ) ;
#9218 = AXIS2_PLACEMENT_3D ( 'NONE', #32562, #22340, #8890 ) ;
#9219 = CARTESIAN_POINT ( 'NONE',  ( 9.984503880673420539, 210.2968891136705167, 90.84886208192143897 ) ) ;
#9220 = CARTESIAN_POINT ( 'NONE',  ( 60.87499999726879452, 138.6155565068815463, -3.929120461958505118E-15 ) ) ;
#9221 = CARTESIAN_POINT ( 'NONE',  ( 10.01549611932653860, 210.2015048109876716, 28.85113791807855677 ) ) ;
#9222 = DIRECTION ( 'NONE',  ( -0.000000000000000000, -0.000000000000000000, -1.000000000000000000 ) ) ;
#9223 = CARTESIAN_POINT ( 'NONE',  ( -7.375838497908014268, 196.7627149292498530, 80.04886208192144181 ) ) ;
#9224 = CARTESIAN_POINT ( 'NONE',  ( 121.5000000000000000, 261.0000000000000000, 0.000000000000000000 ) ) ;
#9225 = CARTESIAN_POINT ( 'NONE',  ( 81.90000000000000568, 141.2096805137202580, 4.480746418436733158 ) ) ;
#9226 = CARTESIAN_POINT ( 'NONE',  ( -1.153701847711675166, -3.375361811986517857, -2.899999999999983924 ) ) ;
#9227 = CARTESIAN_POINT ( 'NONE',  ( 8.451593625408400647E-13, 7.790254909845287123, -6.526045885145519421 ) ) ;
#9228 = CARTESIAN_POINT ( 'NONE',  ( -9.984503880673473830, 210.2968891136704315, 93.65113791807857524 ) ) ;
#9229 = LINE ( 'NONE', #22510, #28184 ) ;
#9230 = CARTESIAN_POINT ( 'NONE',  ( 43.57499999726881157, 164.1591823560292198, -12.60653300113719766 ) ) ;
#9231 = CARTESIAN_POINT ( 'NONE',  ( 0.05014649552810505201, 217.5146222423826714, 34.25113791807856956 ) ) ;
#9232 = CARTESIAN_POINT ( 'NONE',  ( 81.22499999726882436, 160.0630714827496206, -15.58253175000000823 ) ) ;
#9233 = CARTESIAN_POINT ( 'NONE',  ( 99.99999999999998579, 5.109226446042757607E-16, -4.171999999999999709 ) ) ;
#9234 = DIRECTION ( 'NONE',  ( 1.000000000000000000, 0.000000000000000000, 0.000000000000000000 ) ) ;
#9235 = CARTESIAN_POINT ( 'NONE',  ( 47.39999999453763024, 141.2096805137202580, 4.480746418436733158 ) ) ;
#9236 = ORIENTED_EDGE ( 'NONE', *, *, #4558, .T. ) ;
#9237 = CARTESIAN_POINT ( 'NONE',  ( 9.736236675707914401, 214.0148392665762458, 19.70113791807856884 ) ) ;
#9238 = CARTESIAN_POINT ( 'NONE',  ( 60.91132485994280898, 146.1832212156128890, 12.13525491562421976 ) ) ;
#9239 = DIRECTION ( 'NONE',  ( -0.000000000000000000, -0.000000000000000000, -1.000000000000000000 ) ) ;
#9240 = ORIENTED_EDGE ( 'NONE', *, *, #3082, .F. ) ;
#9241 = CARTESIAN_POINT ( 'NONE',  ( 7.456977232089471386, 196.8216656703012006, 43.44886208192143329 ) ) ;
#9242 = CARTESIAN_POINT ( 'NONE',  ( -3.044812012440131443, 216.5253028482142952, 4.101137918078565647 ) ) ;
#9243 = CARTESIAN_POINT ( 'NONE',  ( 10.00000000000000711, 206.9523078486586201, 59.00113791807857666 ) ) ;
#9244 = CARTESIAN_POINT ( 'NONE',  ( 7.984503880673422316, 209.6470497212048372, 9.848862081921433642 ) ) ;
#9245 = CYLINDRICAL_SURFACE ( 'NONE', #31751, 100.0000000000000000 ) ;
#9246 = ORIENTED_EDGE ( 'NONE', *, *, #8909, .F. ) ;
#9247 = CARTESIAN_POINT ( 'NONE',  ( 0.05014649552828262524, 198.5883022060938572, 97.74886208192141623 ) ) ;
#9248 = DIRECTION ( 'NONE',  ( 0.000000000000000000, 0.8660254037844380415, -0.5000000000000012212 ) ) ;
#9249 = CARTESIAN_POINT ( 'NONE',  ( -6.500168698208129925, 202.3363017425936050, 42.20113791807857240 ) ) ;
#9250 = CARTESIAN_POINT ( 'NONE',  ( 33.87499999726880873, 171.3844434931184253, -7.942151717890134290E-15 ) ) ;
#9251 = ORIENTED_EDGE ( 'NONE', *, *, #10224, .T. ) ;
#9252 = CARTESIAN_POINT ( 'NONE',  ( 37.92499999726881299, 164.1591823560292198, 12.60653300113718167 ) ) ;
#9253 = CARTESIAN_POINT ( 'NONE',  ( 5.000000000000000000, -4.685197434473814759, 3.903127820947815962E-15 ) ) ;
#9254 = CARTESIAN_POINT ( 'NONE',  ( 53.71132485994279904, 155.0000000000000000, -15.00000000000002487 ) ) ;
#9255 = CARTESIAN_POINT ( 'NONE',  ( 10.00000000000000711, 207.0476921513415220, 60.99886208192143755 ) ) ;
#9256 = CARTESIAN_POINT ( 'NONE',  ( 38.27499999726881441, 160.0630714827496206, 15.58253174999999402 ) ) ;
#9257 = DIRECTION ( 'NONE',  ( 0.000000000000000000, 0.000000000000000000, -1.000000000000000000 ) ) ;
#9258 = CARTESIAN_POINT ( 'NONE',  ( -10.01549611932653860, 203.7984951890123284, 6.351137918078566535 ) ) ;
#9259 = ADVANCED_FACE ( 'NONE', ( #11328 ), #32270, .F. ) ;
#9260 = CARTESIAN_POINT ( 'NONE',  ( 64.10000000000000853, 141.2096805137202580, -4.480746418436742040 ) ) ;
#9261 = DIRECTION ( 'NONE',  ( 1.000000000000000000, 0.000000000000000000, 0.000000000000000000 ) ) ;
#9262 = CARTESIAN_POINT ( 'NONE',  ( -8.015496119326597224, 209.5516654185217362, 83.64886208192143613 ) ) ;
#9263 = DIRECTION ( 'NONE',  ( 1.000000000000000000, 0.000000000000000000, 0.000000000000000000 ) ) ;
#9264 = CARTESIAN_POINT ( 'NONE',  ( 3.500000000000004441, 0.3416723310689538939, -2.899999999999996803 ) ) ;
#9265 = CARTESIAN_POINT ( 'NONE',  ( 64.22499999726881015, 149.9369285172503510, 15.58253174999999580 ) ) ;
#9267 = ORIENTED_EDGE ( 'NONE', *, *, #17655, .T. ) ;
#9266 = CARTESIAN_POINT ( 'NONE',  ( -10.00000000000000711, 207.0476921513413515, 24.50113791807856600 ) ) ;
#9268 = DIRECTION ( 'NONE',  ( -0.9945218953682714025, 1.280104479605462180E-17, -0.1045284632676720116 ) ) ;
#9269 = CARTESIAN_POINT ( 'NONE',  ( 85.97499999726882436, 169.8198683612136222, 4.815267126137181997 ) ) ;
#9270 = CARTESIAN_POINT ( 'NONE',  ( -7.375838497908182134, 217.2372850707499765, 84.95113791807858661 ) ) ;
#9271 = CARTESIAN_POINT ( 'NONE',  ( 108.0159016311981759, 155.0000000000000000, 0.000000000000000000 ) ) ;
#9272 = ORIENTED_EDGE ( 'NONE', *, *, #324, .F. ) ;
#9273 = CARTESIAN_POINT ( 'NONE',  ( -9.680171189290716072, 199.9079932115567146, 71.19886208192144750 ) ) ;
#9274 = CARTESIAN_POINT ( 'NONE',  ( 6.220909254589680693, 198.5229672870052582, 79.44886208192143329 ) ) ;
#9275 = CARTESIAN_POINT ( 'NONE',  ( 7.375838497908012492, 217.2372850707501186, 15.54886208192143826 ) ) ;
#9276 = EDGE_CURVE ( 'NONE', #29718, #5152, #21539, .T. ) ;
#9277 = DIRECTION ( 'NONE',  ( 1.000000000000000000, 0.000000000000000000, 0.000000000000000000 ) ) ;
#9278 = CARTESIAN_POINT ( 'NONE',  ( -3.044812012440131443, 216.5253028482142952, 34.10113791807857808 ) ) ;
#9279 = CARTESIAN_POINT ( 'NONE',  ( -0.5735064479039797547, 3.710337782248037009, -2.761158938895385884 ) ) ;
#9280 = CARTESIAN_POINT ( 'NONE',  ( -6.220909254589682469, 215.4770327129946850, 89.94886208192140487 ) ) ;
#9281 = DIRECTION ( 'NONE',  ( -0.5000000000000034417, 1.060575238724904696E-16, -0.8660254037844367092 ) ) ;
#9282 = ORIENTED_EDGE ( 'NONE', *, *, #31597, .T. ) ;
#9283 = CARTESIAN_POINT ( 'NONE',  ( -6.500000000000000000, -3.752776749732572803, -6.064240316920399998 ) ) ;
#9284 = CARTESIAN_POINT ( 'NONE',  ( 7.984503880673422316, 209.6470497212048372, 72.84886208192143897 ) ) ;
#9285 = ORIENTED_EDGE ( 'NONE', *, *, #18558, .F. ) ;
#9286 = CARTESIAN_POINT ( 'NONE',  ( 86.62499999726881583, 138.6155565068815747, -3.929120461958505118E-15 ) ) ;
#9287 = ORIENTED_EDGE ( 'NONE', *, *, #11474, .F. ) ;
#9288 = CARTESIAN_POINT ( 'NONE',  ( 0.000000000000000000, 0.000000000000000000, -7.381345277524544279 ) ) ;
#9289 = CARTESIAN_POINT ( 'NONE',  ( 79.52499999726880731, 169.8198683612136222, -4.815267126137197984 ) ) ;
#9290 = CARTESIAN_POINT ( 'NONE',  ( 27.50000000000001066, -15.87713240271473580, -15.54379906938135214 ) ) ;
#9291 = CARTESIAN_POINT ( 'NONE',  ( -7.984503880673488041, 209.6470497212046098, 81.65113791807856103 ) ) ;
#9292 = CARTESIAN_POINT ( 'NONE',  ( -3.500000000000001332, 2.020725942163708488, -2.587392608830344720 ) ) ;
#9293 = ADVANCED_FACE ( 'NONE', ( #1273 ), #766, .F. ) ;
#9294 = CONICAL_SURFACE ( 'NONE', #6573, 10.39117206796836079, 1.221730476396047926 ) ;
#9295 = CARTESIAN_POINT ( 'NONE',  ( 43.30000000000000426, 163.5228861582408797, 11.73074641843673049 ) ) ;
#9296 = CARTESIAN_POINT ( 'NONE',  ( 6.500168698208244500, 202.3363017425938324, 49.29886208192144892 ) ) ;
#9297 = EDGE_CURVE ( 'NONE', #10467, #24797, #3979, .T. ) ;
#9298 = EDGE_CURVE ( 'NONE', #33078, #17976, #19010, .T. ) ;
#9299 = FACE_OUTER_BOUND ( 'NONE', #15931, .T. ) ;
#9300 = LINE ( 'NONE', #19692, #24955 ) ;
#9301 = CARTESIAN_POINT ( 'NONE',  ( 32.50000000000000000, 155.0000000000000000, -15.00000000000002487 ) ) ;
#9302 = CARTESIAN_POINT ( 'NONE',  ( 52.22499999726881725, 149.9369285172503510, 15.58253174999999580 ) ) ;
#9303 = CARTESIAN_POINT ( 'NONE',  ( 65.77499999726880731, 169.8198683612136222, -4.815267126137197984 ) ) ;
#9304 = CARTESIAN_POINT ( 'NONE',  ( -3.662846001190052991, 218.4274158808045740, 58.10113791807857808 ) ) ;
#9305 = CARTESIAN_POINT ( 'NONE',  ( -119.8866434474913518, -1.374176392886225617, 35.00001199999999812 ) ) ;
#9306 = CARTESIAN_POINT ( 'NONE',  ( -9.949154985843399857, 217.7087784572769067, 102.9933096652613074 ) ) ;
#9307 = CARTESIAN_POINT ( 'NONE',  ( 0.05014649552810506589, 217.5146222423826714, 79.25113791807856956 ) ) ;
#9308 = CARTESIAN_POINT ( 'NONE',  ( 9.680171189290716072, 214.0920067884432854, 39.69886208192144039 ) ) ;
#9309 = CARTESIAN_POINT ( 'NONE',  ( -3.135527875058982783, 216.4958274776886924, 48.09886208192143187 ) ) ;
#9310 = CARTESIAN_POINT ( 'NONE',  ( 87.19999999453763451, 146.4771138417591203, 11.73074641843673227 ) ) ;
#9311 = CARTESIAN_POINT ( 'NONE',  ( -3.753561863808691168, 195.6020594897209435, 83.90113791807856103 ) ) ;
#9312 = CARTESIAN_POINT ( 'NONE',  ( -2.426778023690262742, 214.6231898156240163, 100.1011379180785781 ) ) ;
#9313 = ADVANCED_FACE ( 'NONE', ( #22051 ), #32434, .T. ) ;
#9314 = CARTESIAN_POINT ( 'NONE',  ( -9.984503880673420539, 203.7031108863293980, 56.34886208192141765 ) ) ;
#9315 = FILL_AREA_STYLE_COLOUR ( '', #6912 ) ;
#9316 = EDGE_LOOP ( 'NONE', ( #18007, #24239 ) ) ;
#9317 = CARTESIAN_POINT ( 'NONE',  ( 9.736236675708031640, 199.9851607334238963, 67.29886208192144181 ) ) ;
#9318 = CIRCLE ( 'NONE', #3335, 7.500000000000001776 ) ;
#9319 = VERTEX_POINT ( 'NONE', #21816 ) ;
#9320 = CARTESIAN_POINT ( 'NONE',  ( 71.07499999726880446, 141.7447067706911810, -9.630534252274385310 ) ) ;
#9321 = CARTESIAN_POINT ( 'NONE',  ( -2.426778023690076225, 199.3768101843759553, 37.89886208192144323 ) ) ;
#9322 = ADVANCED_FACE ( 'NONE', ( #16204 ), #3592, .F. ) ;
#9323 = EDGE_LOOP ( 'NONE', ( #21481, #22685, #6723 ) ) ;
#9324 = CARTESIAN_POINT ( 'NONE',  ( 81.57499999726880446, 164.1591823560292198, -12.60653300113719766 ) ) ;
#9325 = CARTESIAN_POINT ( 'NONE',  ( -6.127431526422343306E-17, 9.147862274876549904, -8.047472243342932430 ) ) ;
#9326 = DIRECTION ( 'NONE',  ( 0.000000000000000000, -1.000000000000000000, 0.000000000000000000 ) ) ;
#9327 = CARTESIAN_POINT ( 'NONE',  ( -8.015496119326531499, 204.4483345814780364, 60.35113791807857098 ) ) ;
#9328 = FILL_AREA_STYLE_COLOUR ( '', #19995 ) ;
#9329 = CARTESIAN_POINT ( 'NONE',  ( -10.01549611932659722, 210.2015048109875011, 38.64886208192142192 ) ) ;
#9330 = ORIENTED_EDGE ( 'NONE', *, *, #8509, .T. ) ;
#9331 = FACE_OUTER_BOUND ( 'NONE', #7667, .T. ) ;
#9332 =( NAMED_UNIT ( * ) PLANE_ANGLE_UNIT ( ) SI_UNIT ( $, .RADIAN. ) );
#9333 = CARTESIAN_POINT ( 'NONE',  ( 89.50000000000001421, 155.0000000000000000, -13.00000000000002487 ) ) ;
#9334 =( BOUNDED_CURVE ( )  B_SPLINE_CURVE ( 2, ( #10668, #10993, #18659, #15928, #14345, #13541, #31447, #8115, #16892, #29855, #31604 ),
 .UNSPECIFIED., .F., .F. ) 
 B_SPLINE_CURVE_WITH_KNOTS ( ( 3, 2, 2, 2, 2, 3 ),
 ( 0.2678571428571428492, 0.2714285714285714080, 0.2750000000000000222, 0.2785714285714285809, 0.2821428571428571397, 0.2857142857142856984 ),
 .UNSPECIFIED. ) 
 CURVE ( )  GEOMETRIC_REPRESENTATION_ITEM ( )  RATIONAL_B_SPLINE_CURVE ( ( 1.000000000000000000, 0.9510565162951534202, 1.000000000000000000, 0.9510565162951534202, 1.000000000000000000, 0.9510565162951534202, 1.000000000000000000, 0.9510565162951534202, 1.000000000000000000, 0.9510565162951534202, 1.000000000000000000 ) ) 
 REPRESENTATION_ITEM ( '' )  );
#9335 = DIRECTION ( 'NONE',  ( -1.000000000000000000, -0.000000000000000000, -0.000000000000000000 ) ) ;
#9336 = CARTESIAN_POINT ( 'NONE',  ( 8.000000000000008882, 207.0476921513415220, 21.99886208192143400 ) ) ;
#9337 = CARTESIAN_POINT ( 'NONE',  ( -3.135527875058821579, 197.5041725223112223, 62.90113791807858235 ) ) ;
#9338 = CARTESIAN_POINT ( 'NONE',  ( -8.062137200540920645, 212.9164362838581894, 48.80113791807857382 ) ) ;
#9339 = DIRECTION ( 'NONE',  ( 1.000000000000000000, 0.000000000000000000, 0.000000000000000000 ) ) ;
#9340 = CARTESIAN_POINT ( 'NONE',  ( 3.135527875058820690, 216.4958274776887492, 16.40113791807856813 ) ) ;
#9341 = CARTESIAN_POINT ( 'NONE',  ( -8.015496119326597224, 209.5516654185217362, 101.6488620819214361 ) ) ;
#9342 = CARTESIAN_POINT ( 'NONE',  ( 43.42499999726881299, 168.2552932293087906, -9.630534252274385310 ) ) ;
#9343 = CARTESIAN_POINT ( 'NONE',  ( 87.50000000000001421, 147.9321341023432126, -13.35674708564858015 ) ) ;
#9344 = CARTESIAN_POINT ( 'NONE',  ( 12.01549611932652972, 210.8513442034534933, 28.85113791807856032 ) ) ;
#9345 = LINE ( 'NONE', #17183, #425 ) ;
#9346 = EDGE_CURVE ( 'NONE', #13309, #31209, #28146, .T. ) ;
#9347 = CARTESIAN_POINT ( 'NONE',  ( -6.139770520408369237, 215.5359834540460042, 78.95113791807858661 ) ) ;
#9348 = CARTESIAN_POINT ( 'NONE',  ( 8.118202686958039038, 212.8392687619912635, 52.70113791807857240 ) ) ;
#9349 = DIRECTION ( 'NONE',  ( 0.000000000000000000, 0.000000000000000000, 1.000000000000000000 ) ) ;
#9350 = CARTESIAN_POINT ( 'NONE',  ( 0.000000000000000000, 0.000000000000000000, -2.874600000000001376 ) ) ;
#9351 = CARTESIAN_POINT ( 'NONE',  ( -3.753561863808878130, 218.3979405102790281, 12.09886208192143364 ) ) ;
#9352 = CARTESIAN_POINT ( 'NONE',  ( 3.044812012439969795, 216.5253028482143520, 15.39886208192143613 ) ) ;
#9353 = CARTESIAN_POINT ( 'NONE',  ( 65.89999999453762314, 150.2886644046228639, -14.50000000000000888 ) ) ;
#9354 = VECTOR ( 'NONE', #11527, 1000.000000000000000 ) ;
#9355 = ORIENTED_EDGE ( 'NONE', *, *, #15223, .T. ) ;
#9356 = CARTESIAN_POINT ( 'NONE',  ( -12.00000000000000711, 207.0476921513413515, 54.50113791807857666 ) ) ;
#9357 = CARTESIAN_POINT ( 'NONE',  ( -6.444103211791042618, 211.7408657792732356, 72.80113791807858092 ) ) ;
#9358 = ADVANCED_FACE ( 'NONE', ( #3258 ), #11110, .F. ) ;
#9359 = CARTESIAN_POINT ( 'NONE',  ( -8.118202686958138514, 212.8392687619910930, 32.79886208192143471 ) ) ;
#9360 = B_SPLINE_CURVE_WITH_KNOTS ( 'NONE', 3,
 ( #32326, #17161, #19380, #1330 ),
 .UNSPECIFIED., .F., .F.,
 ( 4, 4 ),
 ( 2.380739282314300957E-07, 0.002044882221487520201 ),
 .UNSPECIFIED. ) ;
#9361 = CARTESIAN_POINT ( 'NONE',  ( 76.21132485994282035, 170.7719333635740497, -7.904646289410545231E-15 ) ) ;
#9362 = ORIENTED_EDGE ( 'NONE', *, *, #12805, .T. ) ;
#9363 = CARTESIAN_POINT ( 'NONE',  ( -8.062137200540920645, 212.9164362838581894, 87.80113791807856671 ) ) ;
#9364 = EDGE_CURVE ( 'NONE', #5152, #9697, #10733, .T. ) ;
#9365 = EDGE_LOOP ( 'NONE', ( #7502, #18839, #16239, #6084, #1870, #29008, #12527, #13312, #10938, #5541, #33543, #33429, #29833, #11724, #15393, #26125, #12298, #16778, #16949, #13713, #11286, #6160, #601, #25340, #3369, #2550, #22571, #32522, #27843, #17883, #21588, #8813, #27892, #14407, #26210, #8170, #16942, #661, #27002, #29566, #7122, #11047, #27758, #1571, #15872, #6739, #12639, #6849, #33474, #14907, #10443, #20362, #26381, #20308, #29860, #28330, #24613, #32742 ) ) ;
#9366 = CARTESIAN_POINT ( 'NONE',  ( 42.08867513459482979, 142.2402378747194405, 9.270509831248432420 ) ) ;
#9367 = AXIS2_PLACEMENT_3D ( 'NONE', #20875, #26314, #18156 ) ;
#9368 = DIRECTION ( 'NONE',  ( 0.000000000000000000, 0.000000000000000000, 1.000000000000000000 ) ) ;
#9369 = ORIENTED_EDGE ( 'NONE', *, *, #22678, .T. ) ;
#9370 = CARTESIAN_POINT ( 'NONE',  ( -7.984503880673488041, 209.6470497212046098, 33.65113791807856813 ) ) ;
#9371 = CARTESIAN_POINT ( 'NONE',  ( 92.60208470531341618, 155.0000000000000000, 0.000000000000000000 ) ) ;
#9372 = CARTESIAN_POINT ( 'NONE',  ( -6.139770520408224463, 198.4640165459539389, 11.04886208192143648 ) ) ;
#9373 = CARTESIAN_POINT ( 'NONE',  ( 58.57499999726881157, 145.8408176439707802, 12.60653300113718345 ) ) ;
#9374 = ORIENTED_EDGE ( 'NONE', *, *, #15586, .F. ) ;
#9375 = CARTESIAN_POINT ( 'NONE',  ( 2.426778023690261410, 199.3768101843759837, 53.60113791807856387 ) ) ;
#9376 = CARTESIAN_POINT ( 'NONE',  ( 1.083333333333332593, -6.880090707843051767, -5.848636054922041083 ) ) ;
#9377 = AXIS2_PLACEMENT_3D ( 'NONE', #3850, #17137, #12024 ) ;
#9378 = SURFACE_STYLE_FILL_AREA ( #9544 ) ;
#9379 = CARTESIAN_POINT ( 'NONE',  ( 57.11132485994280472, 140.7341522555726669, 4.635254915624211769 ) ) ;
#9380 = CARTESIAN_POINT ( 'NONE',  ( 6.139770520408223575, 215.5359834540460611, 102.5488620819214134 ) ) ;
#9381 = CARTESIAN_POINT ( 'NONE',  ( 62.07499999726881157, 168.2552932293087906, 9.630534252274372875 ) ) ;
#9382 = CARTESIAN_POINT ( 'NONE',  ( 6.139770520408368348, 198.4640165459539674, 35.45113791807857240 ) ) ;
#9383 = CARTESIAN_POINT ( 'NONE',  ( 125.5000000000000000, 80.04668119422552763, -74.95331880577366235 ) ) ;
#9384 = CARTESIAN_POINT ( 'NONE',  ( 10.00000000000000711, 206.9523078486586201, 17.00113791807856600 ) ) ;
#9385 = CARTESIAN_POINT ( 'NONE',  ( 58.50000000000000711, -88.00000000000000000, -38.00000000000000711 ) ) ;
#9386 = CARTESIAN_POINT ( 'NONE',  ( 80.10000000000000853, 141.2096805137202580, -4.480746418436742040 ) ) ;
#9387 = CARTESIAN_POINT ( 'NONE',  ( -0.5725525826505220017, -3.710888496608931497, -2.778243469714873903 ) ) ;
#9388 = CARTESIAN_POINT ( 'NONE',  ( 3.750000000000004441, -6.495190528383289141, 0.000000000000000000 ) ) ;
#9389 = CARTESIAN_POINT ( 'NONE',  ( -9.680171189290831535, 214.0920067884431148, 0.8011379180785656029 ) ) ;
#9390 = DIRECTION ( 'NONE',  ( -0.000000000000000000, -0.000000000000000000, -1.000000000000000000 ) ) ;
#9391 = CARTESIAN_POINT ( 'NONE',  ( 41.77499999726881441, 169.8198683612136222, -4.815267126137197984 ) ) ;
#9392 = CARTESIAN_POINT ( 'NONE',  ( 10.00000000000000711, 206.9523078486586201, 44.00113791807857666 ) ) ;
#9393 = ADVANCED_FACE ( 'NONE', ( #23877 ), #9625, .T. ) ;
#9394 = CARTESIAN_POINT ( 'NONE',  ( 84.62499999726880162, 138.6155565068815463, -3.929120461958505118E-15 ) ) ;
#9395 = PRODUCT_DEFINITION_FORMATION_WITH_SPECIFIED_SOURCE ( 'ANY', '', #22203, .NOT_KNOWN. ) ;
#9396 = CARTESIAN_POINT ( 'NONE',  ( 62.70000000000001705, -88.00000000000000000, -30.00000000000000000 ) ) ;
#9397 = PLANE ( 'NONE',  #7573 ) ;
#9398 = CARTESIAN_POINT ( 'NONE',  ( 48.99999999453763166, 155.0000000000000000, 14.49999999999999467 ) ) ;
#9399 = EDGE_LOOP ( 'NONE', ( #9153, #22321, #6718, #15357 ) ) ;
#9400 = CARTESIAN_POINT ( 'NONE',  ( -9.736236675707914401, 199.9851607334237542, 30.20113791807856529 ) ) ;
#9401 = EDGE_CURVE ( 'NONE', #18094, #9027, #22488, .T. ) ;
#9402 = EDGE_CURVE ( 'NONE', #27639, #28972, #27107, .T. ) ;
#9403 = CARTESIAN_POINT ( 'NONE',  ( 61.21132485994281325, 139.2280666364260071, -4.041636747397287284E-15 ) ) ;
#9404 = CARTESIAN_POINT ( 'NONE',  ( -10.00000000000000178, 208.0352956435529563, 102.7846294209004441 ) ) ;
#9405 = ORIENTED_EDGE ( 'NONE', *, *, #7998, .F. ) ;
#9406 = TOROIDAL_SURFACE ( 'NONE', #32791, 4.999999999999990230, 2.500000000000000000 ) ;
#9407 = CARTESIAN_POINT ( 'NONE',  ( 9.680171189290716072, 214.0920067884432854, 42.69886208192142618 ) ) ;
#9408 = FACE_OUTER_BOUND ( 'NONE', #14054, .T. ) ;
#9409 = CARTESIAN_POINT ( 'NONE',  ( 10.01549611932653860, 210.2015048109876716, 61.85113791807857098 ) ) ;
#9410 = VECTOR ( 'NONE', #20356, 1000.000000000000000 ) ;
#9411 = CARTESIAN_POINT ( 'NONE',  ( -4.984841277089891776, 213.7757310962905990, 20.94886208192143684 ) ) ;
#9412 = CARTESIAN_POINT ( 'NONE',  ( 5.441945782601302462, 4.363644636964922441, -0.3576316571898402463 ) ) ;
#9413 = ORIENTED_EDGE ( 'NONE', *, *, #2302, .F. ) ;
#9414 = CARTESIAN_POINT ( 'NONE',  ( 6.444103211791042618, 202.2591342207267644, 2.301137918078565825 ) ) ;
#9415 = CARTESIAN_POINT ( 'NONE',  ( 117.5000000000000000, 180.9145392013172682, 100.8678580070898931 ) ) ;
#9416 = CARTESIAN_POINT ( 'NONE',  ( 12.00000000000000711, 207.0476921513415220, 90.99886208192144466 ) ) ;
#9417 = CYLINDRICAL_SURFACE ( 'NONE', #29847, 15.00000000000001776 ) ;
#9418 = ORIENTED_EDGE ( 'NONE', *, *, #26864, .T. ) ;
#9419 = CARTESIAN_POINT ( 'NONE',  ( 35.32499999726881157, 164.1591823560292198, -12.60653300113719766 ) ) ;
#9420 = CARTESIAN_POINT ( 'NONE',  ( 117.5000000000000142, 155.0000000000000000, -6.938893903907228378E-15 ) ) ;
#9421 = CARTESIAN_POINT ( 'NONE',  ( -3.755786496842903988E-16, -7.505553499465146494, -6.064240316920404439 ) ) ;
#9422 = CONICAL_SURFACE ( 'NONE', #5071, 32.10452846326769816, 1.466076571675243523 ) ;
#9423 = CARTESIAN_POINT ( 'NONE',  ( 9.984503880673420539, 210.2968891136705167, 60.84886208192142476 ) ) ;
#9424 = CARTESIAN_POINT ( 'NONE',  ( 40.67499999726880588, 141.7447067706911810, 9.630534252274376428 ) ) ;
#9425 = FACE_OUTER_BOUND ( 'NONE', #22030, .T. ) ;
#9426 = CARTESIAN_POINT ( 'NONE',  ( 6.139770520408368348, 198.4640165459539674, 2.451137918078566180 ) ) ;
#9427 = CARTESIAN_POINT ( 'NONE',  ( 0.000000000000000000, 0.000000000000000000, -18.00000000000000000 ) ) ;
#9428 =( REPRESENTATION_RELATIONSHIP ('NONE','NONE', #25663, #32622 ) REPRESENTATION_RELATIONSHIP_WITH_TRANSFORMATION ( #2530 )SHAPE_REPRESENTATION_RELATIONSHIP( ) );
#9429 = AXIS2_PLACEMENT_3D ( 'NONE', #19437, #3263, #16711 ) ;
#9430 = CARTESIAN_POINT ( 'NONE',  ( 61.19999999999999574, 167.3344367211045096, 8.961492836873468093 ) ) ;
#9431 = DIRECTION ( 'NONE',  ( 1.000000000000000000, 0.000000000000000000, 0.000000000000000000 ) ) ;
#9432 = CARTESIAN_POINT ( 'NONE',  ( -6.444103211790928043, 202.2591342207265939, 86.19886208192144750 ) ) ;
#9433 = CARTESIAN_POINT ( 'NONE',  ( -7.779103221381273414, 4.168986698926021361, -7.929128246061903695 ) ) ;
#9434 = VECTOR ( 'NONE', #3411, 1000.000000000000000 ) ;
#9435 = LINE ( 'NONE', #4322, #18895 ) ;
#9436 = CARTESIAN_POINT ( 'NONE',  ( 0.05014649552828288198, 194.3824533091408000, 85.74886208192143044 ) ) ;
#9437 = AXIS2_PLACEMENT_3D ( 'NONE', #7797, #290, #18016 ) ;
#9438 = CARTESIAN_POINT ( 'NONE',  ( 63.62499999726879452, 171.3844434931184253, -7.942151717890132712E-15 ) ) ;
#9440 = VERTEX_POINT ( 'NONE', #24211 ) ;
#9439 = CARTESIAN_POINT ( 'NONE',  ( 9.984503880673473830, 203.7031108863295401, 17.15113791807856458 ) ) ;
#9441 = DIRECTION ( 'NONE',  ( 0.000000000000000000, -1.000000000000000000, 0.000000000000000000 ) ) ;
#9442 = CARTESIAN_POINT ( 'NONE',  ( 85.87499999726881583, 171.3844434931184253, -7.942151717890132712E-15 ) ) ;
#9443 = CARTESIAN_POINT ( 'NONE',  ( 3.662846001190051659, 195.5725841191953691, 89.60113791807857808 ) ) ;
#9444 = CARTESIAN_POINT ( 'NONE',  ( -8.118202686958039038, 201.1607312380087080, 102.2011379180785866 ) ) ;
#9445 = ORIENTED_EDGE ( 'NONE', *, *, #15182, .T. ) ;
#9446 = CARTESIAN_POINT ( 'NONE',  ( 9.736236675708031640, 199.9851607334238963, 73.29886208192142760 ) ) ;
#9447 = CARTESIAN_POINT ( 'NONE',  ( -8.118202686958138514, 212.8392687619910930, 74.79886208192144181 ) ) ;
#9448 = CARTESIAN_POINT ( 'NONE',  ( -12.01549611932659722, 210.8513442034533227, 14.64886208192143258 ) ) ;
#9449 = MECHANICAL_DESIGN_GEOMETRIC_PRESENTATION_REPRESENTATION (  '', ( #3457 ), #23587 ) ;
#9450 = CARTESIAN_POINT ( 'NONE',  ( 89.50000000000002842, 155.0000000000000000, 0.000000000000000000 ) ) ;
#9451 = CARTESIAN_POINT ( 'NONE',  ( 3.044812012440130555, 197.4746971517856764, 29.60113791807856742 ) ) ;
#9452 = CARTESIAN_POINT ( 'NONE',  ( -1.156317065392243659, 3.373851915354613151, -2.870065989602862633 ) ) ;
#9453 = CARTESIAN_POINT ( 'NONE',  ( 10.00000000000000711, 207.0476921513415220, 102.9988620819214447 ) ) ;
#9454 = CARTESIAN_POINT ( 'NONE',  ( 2.000000000000000000, -0.8865213383406685965, 1.535500000000000531 ) ) ;
#9455 = ORIENTED_EDGE ( 'NONE', *, *, #13283, .T. ) ;
#9456 = FACE_OUTER_BOUND ( 'NONE', #17082, .T. ) ;
#9457 =( BOUNDED_CURVE ( )  B_SPLINE_CURVE ( 2, ( #11759, #25380, #27432, #2051, #33221, #20269, #1538, #33043, #9713, #30675, #1370 ),
 .UNSPECIFIED., .F., .F. ) 
 B_SPLINE_CURVE_WITH_KNOTS ( ( 3, 2, 2, 2, 2, 3 ),
 ( 0.3749999999999998890, 0.3785714285714284477, 0.3821428571428570620, 0.3857142857142856762, 0.3892857142857142905, 0.3928571428571428492 ),
 .UNSPECIFIED. ) 
 CURVE ( )  GEOMETRIC_REPRESENTATION_ITEM ( )  RATIONAL_B_SPLINE_CURVE ( ( 1.000000000000001554, 0.9510565162951518658, 1.000000000000000000, 0.9510565162951534202, 1.000000000000000000, 0.9510565162951534202, 1.000000000000000000, 0.9510565162951534202, 1.000000000000000000, 0.9510565162951534202, 1.000000000000000000 ) ) 
 REPRESENTATION_ITEM ( '' )  );
#9458 = CARTESIAN_POINT ( 'NONE',  ( 4.903702542908435547, 213.8346818373419751, 66.54886208192144181 ) ) ;
#9459 = AXIS2_PLACEMENT_3D ( 'NONE', #22485, #17542, #14474 ) ;
#9460 = EDGE_LOOP ( 'NONE', ( #25847, #10234, #32942, #19813 ) ) ;
#9461 = CARTESIAN_POINT ( 'NONE',  ( 83.02499999726879309, 149.9369285172503510, -15.58253175000000823 ) ) ;
#9462 = ORIENTED_EDGE ( 'NONE', *, *, #22802, .F. ) ;
#9463 = FACE_OUTER_BOUND ( 'NONE', #27830, .T. ) ;
#9464 = CARTESIAN_POINT ( 'NONE',  ( 75.32499999726881867, 164.1591823560292198, -12.60653300113719766 ) ) ;
#9465 = CARTESIAN_POINT ( 'NONE',  ( 0.05014649552807626948, 215.4116977939061144, 76.25113791807856956 ) ) ;
#9466 = CARTESIAN_POINT ( 'NONE',  ( 0.000000000000000000, 0.000000000000000000, 0.000000000000000000 ) ) ;
#9467 = CARTESIAN_POINT ( 'NONE',  ( 38.79999999999999716, 167.3344367211045096, -8.961492836873482304 ) ) ;
#9468 = CARTESIAN_POINT ( 'NONE',  ( -4.984841277089891776, 213.7757310962905990, 53.94886208192144039 ) ) ;
#9469 = DIRECTION ( 'NONE',  ( 0.000000000000000000, 0.000000000000000000, -1.000000000000000000 ) ) ;
#9470 = CARTESIAN_POINT ( 'NONE',  ( 78.28867513459482552, 139.2280666364260071, -4.041636747397287284E-15 ) ) ;
#9471 = CARTESIAN_POINT ( 'NONE',  ( -10.00000000000000178, 208.0352956435529563, 102.7846294209004441 ) ) ;
#9472 = CARTESIAN_POINT ( 'NONE',  ( 50.52499999726880731, 140.1801316387863778, 4.815267126137185549 ) ) ;
#9473 = CARTESIAN_POINT ( 'NONE',  ( 65.17499999726881299, 145.8408176439707802, -12.60653300113719588 ) ) ;
#9474 = CARTESIAN_POINT ( 'NONE',  ( -0.05014649552807705357, 194.3824533091408000, 53.75113791807857666 ) ) ;
#9475 = AXIS2_PLACEMENT_3D ( 'NONE', #9845, #25164, #24669 ) ;
#9476 = CARTESIAN_POINT ( 'NONE',  ( -8.062137200540920645, 212.9164362838581894, 99.80113791807858092 ) ) ;
#9477 = CARTESIAN_POINT ( 'NONE',  ( -10.00000000000000711, 207.0476921513413515, 81.50113791807856956 ) ) ;
#9478 = CARTESIAN_POINT ( 'NONE',  ( 9.680171189290716072, 214.0920067884432854, 42.69886208192142618 ) ) ;
#9479 = CARTESIAN_POINT ( 'NONE',  ( 8.118202686958138514, 201.1607312380088501, 49.29886208192143471 ) ) ;
#9480 = DIRECTION ( 'NONE',  ( 0.000000000000000000, 0.000000000000000000, -1.000000000000000000 ) ) ;
#9481 = CARTESIAN_POINT ( 'NONE',  ( 3.662846001190051659, 195.5725841191953691, 83.60113791807857808 ) ) ;
#9482 = DIRECTION ( 'NONE',  ( 0.000000000000000000, 0.000000000000000000, -1.000000000000000000 ) ) ;
#9483 = CARTESIAN_POINT ( 'NONE',  ( 0.05014649552810505201, 217.5146222423826714, 4.251137918078566003 ) ) ;
#9484 = CARTESIAN_POINT ( 'NONE',  ( 9.984503880673420539, 210.2968891136705167, 63.84886208192142476 ) ) ;
#9485 = EDGE_CURVE ( 'NONE', #7668, #27493, #24874, .T. ) ;
#9486 = DIRECTION ( 'NONE',  ( 1.000000000000000000, 0.000000000000000000, 0.000000000000000000 ) ) ;
#9487 = ORIENTED_EDGE ( 'NONE', *, *, #20414, .F. ) ;
#9488 = CARTESIAN_POINT ( 'NONE',  ( 0.05014649552828288198, 194.3824533091408000, 70.74886208192144466 ) ) ;
#9489 = MECHANICAL_DESIGN_GEOMETRIC_PRESENTATION_REPRESENTATION (  '', ( #26347 ), #21455 ) ;
#9490 = EDGE_LOOP ( 'NONE', ( #23028, #18342, #11789, #2259 ) ) ;
#9491 = CARTESIAN_POINT ( 'NONE',  ( 68.77499999726880731, 140.1801316387863778, 4.815267126137185549 ) ) ;
#9492 = CARTESIAN_POINT ( 'NONE',  ( 7.984503880673422316, 209.6470497212048372, 45.84886208192143897 ) ) ;
#9493 = ADVANCED_FACE ( 'NONE', ( #32376 ), #6144, .T. ) ;
#9494 = ORIENTED_EDGE ( 'NONE', *, *, #22652, .T. ) ;
#9495 = CARTESIAN_POINT ( 'NONE',  ( 81.17499999726882720, 145.8408176439707802, -12.60653300113719588 ) ) ;
#9496 = FACE_OUTER_BOUND ( 'NONE', #14711, .T. ) ;
#9497 = CYLINDRICAL_SURFACE ( 'NONE', #9475, 2.149999999999985256 ) ;
#9498 = CARTESIAN_POINT ( 'NONE',  ( -6.444103211791042618, 211.7408657792732356, 63.80113791807858092 ) ) ;
#9499 = DIRECTION ( 'NONE',  ( -1.000000000000000000, -0.000000000000000000, -0.000000000000000000 ) ) ;
#9500 = CARTESIAN_POINT ( 'NONE',  ( -3.044812012439970683, 197.4746971517856196, 37.89886208192143613 ) ) ;
#9501 = ORIENTED_EDGE ( 'NONE', *, *, #20637, .T. ) ;
#9502 = DIRECTION ( 'NONE',  ( -1.000000000000000000, 0.000000000000000000, 0.000000000000000000 ) ) ;
#9503 = CARTESIAN_POINT ( 'NONE',  ( 4.444974277458119793, -4.939246403833736032, -5.720331885005374595 ) ) ;
#9504 = DIRECTION ( 'NONE',  ( -1.000000000000000000, 0.000000000000000000, 0.000000000000000000 ) ) ;
#9505 = CARTESIAN_POINT ( 'NONE',  ( 6.500168698208244500, 202.3363017425938324, 25.29886208192143826 ) ) ;
#9506 = CARTESIAN_POINT ( 'NONE',  ( -0.05014649552810635652, 196.4853777576173002, 65.75113791807856956 ) ) ;
#9507 = CARTESIAN_POINT ( 'NONE',  ( -3.135527875058821579, 197.5041725223112223, 44.90113791807857524 ) ) ;
#9508 = CARTESIAN_POINT ( 'NONE',  ( 67.78867513459482552, 155.0000000000000000, 15.00000000000001243 ) ) ;
#9509 = ITEM_DEFINED_TRANSFORMATION ( 'NONE', 'NONE', #20808,  #2404 ) ;
#9510 = CARTESIAN_POINT ( 'NONE',  ( -3.044812012440131443, 216.5253028482142952, 16.10113791807856742 ) ) ;
#9511 = CARTESIAN_POINT ( 'NONE',  ( 4.903702542908601636, 200.1653181626581102, 2.451137918078566180 ) ) ;
#9512 = CARTESIAN_POINT ( 'NONE',  ( 47.22499999726881015, 160.0630714827496206, -15.58253175000000823 ) ) ;
#9513 = CARTESIAN_POINT ( 'NONE',  ( -3.528928113779633335, 5.468125903023623557, 1.037615360386517718E-15 ) ) ;
#9514 = CARTESIAN_POINT ( 'NONE',  ( 33.22499999726881725, 160.0630714827496206, -15.58253175000000823 ) ) ;
#9515 = CARTESIAN_POINT ( 'NONE',  ( -7.375838497908182134, 217.2372850707499765, 30.95113791807857595 ) ) ;
#9516 = CARTESIAN_POINT ( 'NONE',  ( 6.500000000000005329, -3.752776749732570583, -6.177805531628536961 ) ) ;
#9517 = EDGE_CURVE ( 'NONE', #20358, #22384, #3423, .T. ) ;
#9518 = CARTESIAN_POINT ( 'NONE',  ( -3.044812012440131443, 216.5253028482142952, 79.10113791807857808 ) ) ;
#9519 = CARTESIAN_POINT ( 'NONE',  ( 0.05014649552810506589, 217.5146222423826714, 46.25113791807857666 ) ) ;
#9520 = DIRECTION ( 'NONE',  ( 0.000000000000000000, 0.000000000000000000, -1.000000000000000000 ) ) ;
#9521 = DIRECTION ( 'NONE',  ( -1.000000000000000000, 0.000000000000000000, 0.000000000000000000 ) ) ;
#9522 = CARTESIAN_POINT ( 'NONE',  ( -0.05014649552828442242, 219.6175466908591716, 9.248862081921435774 ) ) ;
#9523 = CARTESIAN_POINT ( 'NONE',  ( 6.220909254589680693, 198.5229672870052582, 16.44886208192142973 ) ) ;
#9524 = CARTESIAN_POINT ( 'NONE',  ( 70.49999999453763166, 170.2462022514548323, -7.872454543227099337E-15 ) ) ;
#9525 = ORIENTED_EDGE ( 'NONE', *, *, #10237, .T. ) ;
#9526 = CARTESIAN_POINT ( 'NONE',  ( 12.01549611932652972, 210.8513442034534933, 58.85113791807857098 ) ) ;
#9527 = CARTESIAN_POINT ( 'NONE',  ( -2.426778023690262742, 214.6231898156240163, 82.10113791807857808 ) ) ;
#9528 = CARTESIAN_POINT ( 'NONE',  ( 8.118202686958138514, 201.1607312380088501, 31.29886208192143826 ) ) ;
#9529 = EDGE_CURVE ( 'NONE', #29025, #1337, #17264, .T. ) ;
#9530 = DIRECTION ( 'NONE',  ( 0.000000000000000000, 0.000000000000000000, -1.000000000000000000 ) ) ;
#9531 = ORIENTED_EDGE ( 'NONE', *, *, #19129, .T. ) ;
#9532 = ORIENTED_EDGE ( 'NONE', *, *, #19724, .F. ) ;
#9533 = EDGE_LOOP ( 'NONE', ( #7888, #9952, #13263, #31460 ) ) ;
#9534 = EDGE_CURVE ( 'NONE', #7575, #613, #3336, .T. ) ;
#9535 = CARTESIAN_POINT ( 'NONE',  ( 0.000000000000000000, 0.8865213383406723713, 1.535499999999998755 ) ) ;
#9536 = ORIENTED_EDGE ( 'NONE', *, *, #29925, .F. ) ;
#9537 = CARTESIAN_POINT ( 'NONE',  ( 6.444103211791042618, 202.2591342207267644, 29.30113791807857027 ) ) ;
#9538 = DIRECTION ( 'NONE',  ( 0.000000000000000000, 0.000000000000000000, -1.000000000000000000 ) ) ;
#9539 = CARTESIAN_POINT ( 'NONE',  ( 8.118202686958138514, 201.1607312380088501, 16.29886208192143471 ) ) ;
#9540 = CARTESIAN_POINT ( 'NONE',  ( 58.37499999726881583, 155.0000000000000000, 15.58253174999999402 ) ) ;
#9541 = VERTEX_POINT ( 'NONE', #24382 ) ;
#9542 = CARTESIAN_POINT ( 'NONE',  ( -4.903702542908602524, 213.8346818373418898, 45.95113791807857950 ) ) ;
#9543 = DIRECTION ( 'NONE',  ( 1.000000000000000000, 0.000000000000000000, 0.000000000000000000 ) ) ;
#9544 = FILL_AREA_STYLE ('',( #22662 ) ) ;
#9545 = DIRECTION ( 'NONE',  ( 1.000000000000000000, 0.000000000000000000, 0.000000000000000000 ) ) ;
#9546 = CARTESIAN_POINT ( 'NONE',  ( -9.984503880673420539, 203.7031108863293980, 98.34886208192143897 ) ) ;
#9547 = CARTESIAN_POINT ( 'NONE',  ( 68.27499999726879309, 160.0630714827496206, 15.58253174999999402 ) ) ;
#9548 = CARTESIAN_POINT ( 'NONE',  ( -0.05014649552810635652, 196.4853777576173002, 35.75113791807857666 ) ) ;
#9549 = PLANE ( 'NONE',  #11625 ) ;
#9550 = ADVANCED_FACE ( 'NONE', ( #1047 ), #3768, .F. ) ;
#9551 = CARTESIAN_POINT ( 'NONE',  ( 3.135527875058820690, 216.4958274776887492, 16.40113791807856813 ) ) ;
#9552 = DIRECTION ( 'NONE',  ( 1.000000000000000000, 0.000000000000000000, 0.000000000000000000 ) ) ;
#9553 = CARTESIAN_POINT ( 'NONE',  ( 78.30000000000001137, 146.4771138417591203, -11.73074641843674470 ) ) ;
#9554 = CARTESIAN_POINT ( 'NONE',  ( -11.40740920524442004, -25.16819403002536859, -1.393199791643873198E-14 ) ) ;
#9555 = FACE_OUTER_BOUND ( 'NONE', #24823, .T. ) ;
#9556 = CARTESIAN_POINT ( 'NONE',  ( -10.00000000000000711, 207.0476921513413515, 102.5011379180785838 ) ) ;
#9557 = DIRECTION ( 'NONE',  ( 0.000000000000000000, 0.000000000000000000, -1.000000000000000000 ) ) ;
#9558 = CARTESIAN_POINT ( 'NONE',  ( 50.97499999726881725, 140.1801316387863778, -4.815267126137194431 ) ) ;
#9559 = CARTESIAN_POINT ( 'NONE',  ( 6.139770520408368348, 198.4640165459539674, 47.45113791807857950 ) ) ;
#9560 = CARTESIAN_POINT ( 'NONE',  ( 81.32499999726880446, 164.1591823560292198, -12.60653300113719766 ) ) ;
#9561 = DIRECTION ( 'NONE',  ( 1.000000000000000000, 0.000000000000000000, 0.000000000000000000 ) ) ;
#9562 = DIRECTION ( 'NONE',  ( -1.000000000000000000, -0.000000000000000000, -0.000000000000000000 ) ) ;
#9563 = CARTESIAN_POINT ( 'NONE',  ( 49.29999999453762172, 142.6655632788954620, 8.961492836873471646 ) ) ;
#9564 = ORIENTED_EDGE ( 'NONE', *, *, #31812, .T. ) ;
#9565 = CARTESIAN_POINT ( 'NONE',  ( -3.753561863808691168, 195.6020594897209435, 29.90113791807857169 ) ) ;
#9566 = CARTESIAN_POINT ( 'NONE',  ( -10.47863426674271814, 207.9189531262114770, 102.6635298682156758 ) ) ;
#9567 = CARTESIAN_POINT ( 'NONE',  ( -3.044812012439970683, 197.4746971517856196, 4.898862081921434353 ) ) ;
#9568 = DIRECTION ( 'NONE',  ( 0.000000000000000000, 0.000000000000000000, 1.000000000000000000 ) ) ;
#9569 = ORIENTED_EDGE ( 'NONE', *, *, #12085, .F. ) ;
#9570 = CARTESIAN_POINT ( 'NONE',  ( -3.044812012440131443, 216.5253028482142952, 1.101137918078565869 ) ) ;
#9571 = CARTESIAN_POINT ( 'NONE',  ( 10.01549611932653860, 210.2015048109876716, 64.85113791807857808 ) ) ;
#9572 = CARTESIAN_POINT ( 'NONE',  ( 4.984841277089891776, 200.2242689037093726, 19.44886208192143329 ) ) ;
#9573 = CARTESIAN_POINT ( 'NONE',  ( 1.500000000000001332, 7.960204194457796463E-16, -6.500000000000000888 ) ) ;
#9574 = VERTEX_POINT ( 'NONE', #6495 ) ;
#9575 = CARTESIAN_POINT ( 'NONE',  ( -6.444103211791042618, 211.7408657792732356, 6.801137918078567601 ) ) ;
#9576 = EDGE_CURVE ( 'NONE', #19849, #1328, #32730, .T. ) ;
#9577 = EDGE_CURVE ( 'NONE', #12511, #17462, #9216, .T. ) ;
#9578 = DIRECTION ( 'NONE',  ( -0.000000000000000000, -0.000000000000000000, 1.000000000000000000 ) ) ;
#9579 = AXIS2_PLACEMENT_3D ( 'NONE', #10302, #10463, #13009 ) ;
#9580 = CARTESIAN_POINT ( 'NONE',  ( -0.05014649552828442242, 219.6175466908591716, 90.24886208192144466 ) ) ;
#9581 = CARTESIAN_POINT ( 'NONE',  ( 35.37499999726881583, 155.0000000000000000, -15.58253175000000823 ) ) ;
#9582 = ORIENTED_EDGE ( 'NONE', *, *, #15203, .F. ) ;
#9583 = CARTESIAN_POINT ( 'NONE',  ( 46.42499999726880588, 141.7447067706911810, 9.630534252274376428 ) ) ;
#9584 = DIRECTION ( 'NONE',  ( -0.9998603841633338929, 0.01669062914075312987, 0.0007969188393214247284 ) ) ;
#9585 = DIRECTION ( 'NONE',  ( 0.000000000000000000, 0.000000000000000000, -1.000000000000000000 ) ) ;
#9586 = CARTESIAN_POINT ( 'NONE',  ( 10.00000000000000711, 207.0476921513415220, 66.99886208192143044 ) ) ;
#9587 = CARTESIAN_POINT ( 'NONE',  ( 49.57499999726881157, 164.1591823560292198, -12.60653300113719766 ) ) ;
#9588 = CARTESIAN_POINT ( 'NONE',  ( -10.00000000000000178, 207.9988620819213168, 103.5476921513414794 ) ) ;
#9589 = CARTESIAN_POINT ( 'NONE',  ( 10.01549611932653860, 210.2015048109876716, 4.851137918078563871 ) ) ;
#9590 = CARTESIAN_POINT ( 'NONE',  ( -14.33345751131668777, -23.47883925285269413, -1.404041813368736288E-14 ) ) ;
#9591 = EDGE_CURVE ( 'NONE', #2588, #24969, #19424, .T. ) ;
#9592 = CARTESIAN_POINT ( 'NONE',  ( 59.50000000000000000, 155.0000000000000000, 14.49999999999999467 ) ) ;
#9593 = CARTESIAN_POINT ( 'NONE',  ( -8.118202686958039038, 201.1607312380087080, 87.20113791807858661 ) ) ;
#9594 = LINE ( 'NONE', #28169, #16391 ) ;
#9595 = ADVANCED_BREP_SHAPE_REPRESENTATION ( '', ( #11828, #2404 ), #30714 ) ;
#9596 = CARTESIAN_POINT ( 'NONE',  ( -0.05014649552828365914, 215.4116977939061144, 87.24886208192144466 ) ) ;
#9597 = LINE ( 'NONE', #20160, #24890 ) ;
#9598 = LINE ( 'NONE', #11987, #32969 ) ;
#9599 = ADVANCED_FACE ( 'NONE', ( #16874 ), #14323, .T. ) ;
#9600 = CARTESIAN_POINT ( 'NONE',  ( -9.680171189290716072, 199.9079932115567146, 86.19886208192144750 ) ) ;
#9601 = CARTESIAN_POINT ( 'NONE',  ( 61.22499999726880304, 160.0630714827496206, -15.58253175000000823 ) ) ;
#9603 = EDGE_LOOP ( 'NONE', ( #16588, #18916, #30495, #25047 ) ) ;
#9602 = CARTESIAN_POINT ( 'NONE',  ( -3.044812012440131443, 216.5253028482142952, 16.10113791807856742 ) ) ;
#9604 = DIRECTION ( 'NONE',  ( -1.000000000000000000, 0.000000000000000000, 0.000000000000000000 ) ) ;
#9605 = CARTESIAN_POINT ( 'NONE',  ( 84.17499999726882720, 164.1591823560292198, 12.60653300113718167 ) ) ;
#9606 = CARTESIAN_POINT ( 'NONE',  ( -0.05014649552807705357, 194.3824533091408000, 86.75113791807856956 ) ) ;
#9607 = AXIS2_PLACEMENT_3D ( 'NONE', #33592, #10274, #6125 ) ;
#9608 = EDGE_LOOP ( 'NONE', ( #8747, #21027, #18765, #7455, #18355 ) ) ;
#9609 = CARTESIAN_POINT ( 'NONE',  ( 0.05014649552828288198, 194.3824533091408000, 70.74886208192144466 ) ) ;
#9610 = CARTESIAN_POINT ( 'NONE',  ( 3.044812012439969795, 216.5253028482143520, 72.39886208192143613 ) ) ;
#9611 = CARTESIAN_POINT ( 'NONE',  ( 0.05014649552828288198, 194.3824533091408000, 16.74886208192143755 ) ) ;
#9612 = CARTESIAN_POINT ( 'NONE',  ( 32.50000000000000000, 155.0000000000000000, -6.938893903907228378E-15 ) ) ;
#9613 = CARTESIAN_POINT ( 'NONE',  ( -10.01549611932653860, 203.7984951890123284, 33.35113791807855677 ) ) ;
#9614 = CARTESIAN_POINT ( 'NONE',  ( -27.50000000000000000, -15.87713240271473225, -18.00000000000000000 ) ) ;
#9615 = CARTESIAN_POINT ( 'NONE',  ( 6.139770520408223575, 215.5359834540460611, 96.54886208192141339 ) ) ;
#9616 = CONICAL_SURFACE ( 'NONE', #30286, 37.00000000000000711, 0.7853981633974482790 ) ;
#9617 = DIRECTION ( 'NONE',  ( 1.000000000000000000, -0.000000000000000000, -0.000000000000000000 ) ) ;
#9618 = ORIENTED_EDGE ( 'NONE', *, *, #7029, .F. ) ;
#9619 = FACE_OUTER_BOUND ( 'NONE', #3328, .T. ) ;
#9620 = CARTESIAN_POINT ( 'NONE',  ( 6.500168698208244500, 202.3363017425938324, 76.29886208192142760 ) ) ;
#9621 = ORIENTED_EDGE ( 'NONE', *, *, #3053, .F. ) ;
#9622 = DIRECTION ( 'NONE',  ( -1.000000000000000000, -0.000000000000000000, -0.000000000000000000 ) ) ;
#9623 = VERTEX_POINT ( 'NONE', #27943 ) ;
#9624 = LINE ( 'NONE', #17979, #17251 ) ;
#9625 = CONICAL_SURFACE ( 'NONE', #13440, 1.610000000000000098, 0.7853981633974652654 ) ;
#9626 = CARTESIAN_POINT ( 'NONE',  ( 77.22499999726881015, 160.0630714827496206, -15.58253175000000823 ) ) ;
#9627 = DIRECTION ( 'NONE',  ( 0.000000000000000000, 0.9988620819214357738, 0.04769215134144196705 ) ) ;
#9628 = CARTESIAN_POINT ( 'NONE',  ( 0.05014649552807626948, 215.4116977939061144, 82.25113791807856956 ) ) ;
#9629 = CARTESIAN_POINT ( 'NONE',  ( 87.50000000000005684, 169.6253155642411343, -5.351338237494227101 ) ) ;
#9630 = AXIS2_PLACEMENT_3D ( 'NONE', #5431, #18382, #21097 ) ;
#9631 = VECTOR ( 'NONE', #16358, 1000.000000000000000 ) ;
#9632 =( LENGTH_UNIT ( ) NAMED_UNIT ( * ) SI_UNIT ( .MILLI., .METRE. ) );
#9633 = CARTESIAN_POINT ( 'NONE',  ( 39.50000000000000000, 155.0000000000000000, 14.49999999999999467 ) ) ;
#9634 = CARTESIAN_POINT ( 'NONE',  ( 8.000000000000008882, 207.0476921513415220, 57.99886208192144466 ) ) ;
#9635 = VECTOR ( 'NONE', #33144, 1000.000000000000000 ) ;
#9636 = CYLINDRICAL_SURFACE ( 'NONE', #19709, 13.50000000000001066 ) ;
#9637 = CARTESIAN_POINT ( 'NONE',  ( 1.500000000000001332, 0.000000000000000000, 0.000000000000000000 ) ) ;
#9638 = CARTESIAN_POINT ( 'NONE',  ( -54.50000000000002132, 155.0000000000000000, 6.938893903907228378E-15 ) ) ;
#9639 = CARTESIAN_POINT ( 'NONE',  ( 49.72499999726881725, 169.8198683612136222, 4.815267126137181997 ) ) ;
#9640 = CARTESIAN_POINT ( 'NONE',  ( 61.07499999726881867, 141.7447067706911810, -9.630534252274385310 ) ) ;
#9641 = CARTESIAN_POINT ( 'NONE',  ( -3.753561863808691168, 195.6020594897209435, 56.90113791807858235 ) ) ;
#9642 = CARTESIAN_POINT ( 'NONE',  ( 92.59660660068168170, 155.0000000000000000, 0.000000000000000000 ) ) ;
#9643 = CARTESIAN_POINT ( 'NONE',  ( 6.220909254589536808, 215.4770327129947702, 100.5511379180785809 ) ) ;
#9644 = CARTESIAN_POINT ( 'NONE',  ( -3.135527875058821579, 197.5041725223112223, 77.90113791807857524 ) ) ;
#9645 = CARTESIAN_POINT ( 'NONE',  ( -9.736236675708031640, 214.0148392665760753, 38.79886208192142050 ) ) ;
#9646 = CARTESIAN_POINT ( 'NONE',  ( 8.062137200540822946, 212.9164362838583315, 48.69886208192144039 ) ) ;
#9647 = DIRECTION ( 'NONE',  ( 0.9396926207859143121, 1.150791560227857665E-16, -0.3420201433256525592 ) ) ;
#9648 =( BOUNDED_CURVE ( )  B_SPLINE_CURVE ( 2, ( #29871, #3460, #16910, #6184, #27306, #9250, #16575, #19644, #30033, #14693, #23211, #4472, #33606, #2437, #9932, #20145, #25257, #4812, #25424, #17250, #9581, #12142, #12485, #30719, #30541, #10285, #27638, #27805, #20315, #12818, #1923, #25597, #20664, #25085, #17590, #25766, #22874, #22704, #9762, #23040, #14861, #1743, #10108, #19974, #33436, #20486, #30889, #17420, #2263, #31058, #33265, #33093, #7204, #7554, #12309, #15374, #7379, #4307, #28155, #27981, #17758, #4648, #12645, #15032, #2098, #17941, #22537, #15206, #28329, #4987, #32922, #30376, #7038, #21149, #3254, #13154, #10773, #28498, #18268, #15871, #8053, #13317, #24036, #2775, #12992, #20820, #7887, #23386, #13642, #13480, #5482, #50, #31709, #25931, #5316, #28990, #28657, #10446, #23546, #26589, #15705, #21485, #5151, #5803, #26107, #15539, #215, #31223, #18769, #10612, #5649, #23873, #20987, #704, #31383, #18437, #28826, #545, #26266, #7717, #2605, #370, #11106, #2934, #23709, #31547, #8215, #21313, #8381, #18603, #16037, #26428, #10937, #3091, #29152, #18103, #16199, #13981, #18929, #8706, #32537, #27102, #29325, #8867, #6140, #3419, #22149, #16533, #5973, #4090, #19096, #14480, #17040, #24545, #1043, #26930, #19428, #6307, #31869, #24207, #3764, #14149, #11598, #11435, #24877, #8534, #29484, #1199, #27434, #3588, #6492, #1540, #16361, #32204, #11937, #1373, #24377, #26755, #21812, #9213, #13814, #870, #19265, #29658, #11266, #19603, #16702, #21648, #32043, #21986, #32372, #9036, #29831, #16871, #27264, #3921, #14320, #24717, #11761, #29995, #6652, #2053, #1881, #4942, #22320, #32880, #14993, #17894, #6996, #30678, #25722, #30164, #22658, #30846, #17546, #27766, #14818, #28108, #19931, #20447, #4610, #25051, #4769, #15163, #25556, #22494, #7342, #30329, #12266, #2220, #32706, #30499, #12604, #9888, #25382, #17382, #17721, #12441, #28288, #4430, #22832, #17207, #22999, #2395, #25216, #27940, #15328, #33046, #27594, #1704, #9540, #4261, #9373, #33399, #20106, #14655, #10070, #6822, #9715, #20271, #7162, #33224, #7510, #19769, #12101, #26545, #33563, #10896, #31174, #20620, #5272, #2562, #23831, #25893, #10728, #28947, #9, #5761, #23345, #18058, #18230, #10404, #12781, #31019, #20777, #8010, #26068, #26220, #5604, #15503, #23172, #12950, #16154, #7845, #13112, #18562, #170, #15666, #23667, #502, #28788, #28620, #327, #2738, #28453, #23503, #31669, #10570, #20948, #31342, #5112, #21110, #18395, #5445, #15830, #18728, #31509, #29112, #10242, #2888, #13275, #8177, #15997, #26389, #3048, #13433, #7676, #21273, #8337, #32160, #16489, #16658, #29784, #5931, #3216, #3376, #29953, #31997, #3546, #8997, #24326, #27055, #6609, #6449, #19053, #23998, #13770, #3879, #660, #3718, #26888, #21445, #24167, #14106, #24501, #19222, #8820, #13938, #18885, #29619, #16830, #6091, #11219, #1160, #11394, #13602, #29280, #6267, #16993, #27224, #21601, #16323, #11553, #14272, #997, #21771, #829, #21941, #32331, #1336, #19386, #11723, #24672, #8662, #29443, #22109, #32496, #9168, #19561, #11063, #31827, #8493, #26714, #27847, #20188, #25301, #4520, #14910, #12356, #1965, #22752, #33145, #9808, #30587, #7252, #5923, #21764, #31662, #29272, #12814, #3043, #654, #26539, #26382, #10281, #8814, #8329, #11055, #11387, #16317, #26708, #31988, #23991, #823, #23823, #16148, #8656, #25761, #21436, #19047, #13763, #8487, #21267, #11214, #3370, #32154, #18722, #24158, #23206, #13428, #31821, #494, #18878, #19214, #29107, #31054, #5598, #10891, #8171, #29613, #29436, #21596, #18554, #16482, #20659, #5754, #6085, #3209, #28939, #13597, #6261, #26880, #2433, #33602, #24320, #3538, #15991, #13931, #989, #27725, #29776, #14608, #32829, #3873, #9664, #27218, #21932, #22103, #9495, #14266, #16650, #6945, #9324, #32996, #29947, #27380, #24666, #14437, #30279, #17334, #11717, #1329, #30111, #19882, #32490, #6775, #20056, #4384, #9159, #3711, #19554, #14770, #11888, #14100, #4046, #6603, #32325, #25162, #16986, #24494, #22609, #24830, #30456, #1828, #19716, #1494, #22275, #4210, #32659, #27049, #8991, #11547, #17160, #27546, #25004, #1155, #19379, #1656, #12050, #12221, #22438, #6441, #16823, #15476, #30813, #10205, #18534, #12916, #2708, #28259, #28916, #13086, #26363 ),
 .UNSPECIFIED., .F., .T. ) 
 B_SPLINE_CURVE_WITH_KNOTS ( ( 3, 2, 2, 2, 2, 2, 2, 2, 2, 2, 2, 2, 2, 2, 2, 2, 2, 2, 2, 2, 2, 2, 2, 2, 2, 2, 2, 2, 2, 2, 2, 2, 2, 2, 2, 2, 2, 2, 2, 2, 2, 2, 2, 2, 2, 2, 2, 2, 2, 2, 2, 2, 2, 2, 2, 2, 2, 2, 2, 2, 2, 2, 2, 2, 2, 2, 2, 2, 2, 2, 2, 2, 2, 2, 2, 2, 2, 2, 2, 2, 2, 2, 2, 2, 2, 2, 2, 2, 2, 2, 2, 2, 2, 2, 2, 2, 2, 2, 2, 2, 2, 2, 2, 2, 2, 2, 2, 2, 2, 2, 2, 2, 2, 2, 2, 2, 2, 2, 2, 2, 2, 2, 2, 2, 2, 2, 2, 2, 2, 2, 2, 2, 2, 2, 2, 2, 2, 2, 2, 2, 2, 2, 2, 2, 2, 2, 2, 2, 2, 2, 2, 2, 2, 2, 2, 2, 2, 2, 2, 2, 2, 2, 2, 2, 2, 2, 2, 2, 2, 2, 2, 2, 2, 2, 2, 2, 2, 2, 2, 2, 2, 2, 2, 2, 2, 2, 2, 2, 2, 2, 2, 2, 2, 2, 2, 2, 2, 2, 2, 2, 2, 2, 2, 2, 2, 2, 2, 2, 2, 2, 2, 2, 2, 2, 2, 2, 2, 2, 2, 2, 2, 2, 2, 2, 2, 2, 2, 2, 2, 2, 2, 2, 2, 2, 2, 2, 2, 2, 2, 2, 2, 2, 2, 2, 2, 2, 2, 2, 2, 2, 2, 2, 2, 2, 2, 2, 2, 2, 2, 2, 2, 2, 2, 2, 2, 2, 2, 2, 2, 2, 2, 3 ),
 ( 0.000000000000000000, 0.003571428571428571317, 0.007142857142857142634, 0.01071428571428571438, 0.01428571428571428527, 0.01785714285714285615, 0.02142857142857142877, 0.02500000000000000139, 0.02857142857142857054, 0.03214285714285713969, 0.03571428571428571230, 0.03928571428571428492, 0.04285714285714285754, 0.04642857142857143016, 0.05000000000000000278, 0.05357142857142856845, 0.05714285714285714107, 0.06071428571428571369, 0.06428571428571427937, 0.06785714285714285199, 0.07142857142857142461, 0.07499999999999999722, 0.07857142857142856984, 0.08214285714285714246, 0.08571428571428571508, 0.08928571428571428770, 0.09285714285714286031, 0.09642857142857143293, 0.1000000000000000056, 0.1035714285714285782, 0.1071428571428571369, 0.1107142857142857095, 0.1142857142857142821, 0.1178571428571428548, 0.1214285714285714274, 0.1250000000000000000, 0.1285714285714285587, 0.1321428571428571452, 0.1357142857142857040, 0.1392857142857142905, 0.1428571428571428492, 0.1464285714285714357, 0.1499999999999999944, 0.1535714285714285809, 0.1571428571428571397, 0.1607142857142857262, 0.1642857142857142849, 0.1678571428571428437, 0.1714285714285714302, 0.1749999999999999889, 0.1785714285714285754, 0.1821428571428571341, 0.1857142857142857206, 0.1892857142857142794, 0.1928571428571428659, 0.1964285714285714246, 0.2000000000000000111, 0.2035714285714285698, 0.2071428571428571563, 0.2107142857142857151, 0.2142857142857142738, 0.2178571428571428603, 0.2214285714285714191, 0.2250000000000000056, 0.2285714285714285643, 0.2321428571428571508, 0.2357142857142857095, 0.2392857142857142960, 0.2428571428571428548, 0.2464285714285714413, 0.2500000000000000000, 0.2535714285714285587, 0.2571428571428571175, 0.2607142857142857317, 0.2642857142857142905, 0.2678571428571428492, 0.2714285714285714080, 0.2749999999999999667, 0.2785714285714285809, 0.2821428571428571397, 0.2857142857142856984, 0.2892857142857143127, 0.2928571428571428714, 0.2964285714285714302, 0.2999999999999999889, 0.3035714285714285476, 0.3071428571428571619, 0.3107142857142857206, 0.3142857142857142794, 0.3178571428571428381, 0.3214285714285714524, 0.3249999999999999556, 0.3285714285714285698, 0.3321428571428571286, 0.3357142857142856873, 0.3392857142857143016, 0.3428571428571428603, 0.3464285714285714191, 0.3499999999999999778, 0.3535714285714285920, 0.3571428571428571508, 0.3607142857142857095, 0.3642857142857142683, 0.3678571428571428825, 0.3714285714285714413, 0.3750000000000000555, 0.3785714285714285587, 0.3821428571428571175, 0.3857142857142857317, 0.3892857142857142905, 0.3928571428571428492, 0.3964285714285714080, 0.4000000000000000222, 0.4035714285714285809, 0.4071428571428571397, 0.4107142857142856984, 0.4142857142857143127, 0.4178571428571428714, 0.4214285714285714302, 0.4250000000000000444, 0.4285714285714285476, 0.4321428571428571619, 0.4357142857142857206, 0.4392857142857142794, 0.4428571428571428381, 0.4464285714285714524, 0.4500000000000000111, 0.4535714285714285698, 0.4571428571428571286, 0.4607142857142856873, 0.4642857142857143016, 0.4678571428571428603, 0.4714285714285714191, 0.4750000000000000333, 0.4785714285714285920, 0.4821428571428571508, 0.4857142857142857095, 0.4892857142857142683, 0.4928571428571428825, 0.4964285714285714413, 0.5000000000000000000, 0.5035714285714285587, 0.5071428571428571175, 0.5107142857142856762, 0.5142857142857142350, 0.5178571428571429047, 0.5214285714285714635, 0.5250000000000000222, 0.5285714285714285809, 0.5321428571428571397, 0.5357142857142856984, 0.5392857142857142572, 0.5428571428571428159, 0.5464285714285713746, 0.5499999999999999334, 0.5535714285714286031, 0.5571428571428571619, 0.5607142857142857206, 0.5642857142857142794, 0.5678571428571428381, 0.5714285714285713969, 0.5749999999999999556, 0.5785714285714286254, 0.5821428571428571841, 0.5857142857142857428, 0.5892857142857143016, 0.5928571428571428603, 0.5964285714285714191, 0.5999999999999999778, 0.6035714285714285365, 0.6071428571428570953, 0.6107142857142857650, 0.6142857142857143238, 0.6178571428571428825, 0.6214285714285714413, 0.6250000000000000000, 0.6285714285714285587, 0.6321428571428571175, 0.6357142857142856762, 0.6392857142857142350, 0.6428571428571429047, 0.6464285714285714635, 0.6499999999999999112, 0.6535714285714285809, 0.6571428571428571397, 0.6607142857142856984, 0.6642857142857142572, 0.6678571428571428159, 0.6714285714285713746, 0.6750000000000000444, 0.6785714285714286031, 0.6821428571428571619, 0.6857142857142857206, 0.6892857142857142794, 0.6928571428571428381, 0.6964285714285713969, 0.6999999999999999556, 0.7035714285714286254, 0.7071428571428571841, 0.7107142857142857428, 0.7142857142857143016, 0.7178571428571428603, 0.7214285714285714191, 0.7249999999999999778, 0.7285714285714285365, 0.7321428571428570953, 0.7357142857142857650, 0.7392857142857143238, 0.7428571428571428825, 0.7464285714285714413, 0.7500000000000001110, 0.7535714285714285587, 0.7571428571428571175, 0.7607142857142856762, 0.7642857142857142350, 0.7678571428571429047, 0.7714285714285714635, 0.7750000000000000222, 0.7785714285714285809, 0.7821428571428571397, 0.7857142857142856984, 0.7892857142857142572, 0.7928571428571428159, 0.7964285714285713746, 0.8000000000000000444, 0.8035714285714286031, 0.8071428571428571619, 0.8107142857142857206, 0.8142857142857142794, 0.8178571428571428381, 0.8214285714285713969, 0.8249999999999999556, 0.8285714285714286254, 0.8321428571428571841, 0.8357142857142857428, 0.8392857142857143016, 0.8428571428571428603, 0.8464285714285714191, 0.8500000000000000888, 0.8535714285714285365, 0.8571428571428570953, 0.8607142857142857650, 0.8642857142857143238, 0.8678571428571428825, 0.8714285714285714413, 0.8750000000000000000, 0.8785714285714285587, 0.8821428571428571175, 0.8857142857142856762, 0.8892857142857142350, 0.8928571428571429047, 0.8964285714285714635, 0.9000000000000000222, 0.9035714285714285809, 0.9071428571428571397, 0.9107142857142856984, 0.9142857142857142572, 0.9178571428571428159, 0.9214285714285713746, 0.9250000000000000444, 0.9285714285714286031, 0.9321428571428571619, 0.9357142857142857206, 0.9392857142857142794, 0.9428571428571428381, 0.9464285714285713969, 0.9500000000000000666, 0.9535714285714286254, 0.9571428571428571841, 0.9607142857142857428, 0.9642857142857143016, 0.9665075840475536584 ),
 .UNSPECIFIED. ) 
 CURVE ( )  GEOMETRIC_REPRESENTATION_ITEM ( )  RATIONAL_B_SPLINE_CURVE ( ( 1.000000000000000000, 0.9510565162951535312, 1.000000000000000000, 0.9510565162951535312, 1.000000000000000000, 0.9510565162951535312, 1.000000000000000000, 0.9510565162951535312, 1.000000000000000000, 0.9510565162951535312, 1.000000000000000000, 0.9510565162951535312, 1.000000000000000000, 0.9510565162951535312, 1.000000000000000000, 0.9510565162951535312, 1.000000000000000000, 0.9510565162951535312, 1.000000000000000000, 0.9510565162951535312, 1.000000000000000000, 0.9510565162951535312, 1.000000000000000000, 0.9510565162951535312, 1.000000000000000000, 0.9510565162951535312, 1.000000000000000000, 0.9510565162951535312, 1.000000000000000000, 0.9510565162951535312, 1.000000000000000000, 0.9510565162951535312, 1.000000000000000000, 0.9510565162951535312, 1.000000000000000000, 0.9510565162951535312, 1.000000000000000000, 0.9510565162951535312, 1.000000000000000000, 0.9510565162951535312, 1.000000000000000000, 0.9510565162951535312, 1.000000000000000000, 0.9510565162951535312, 1.000000000000000000, 0.9510565162951535312, 1.000000000000000000, 0.9510565162951535312, 1.000000000000000000, 0.9510565162951535312, 1.000000000000000000, 0.9510565162951535312, 1.000000000000000000, 0.9510565162951535312, 1.000000000000000000, 0.9510565162951535312, 1.000000000000000000, 0.9510565162951535312, 1.000000000000000000, 0.9510565162951535312, 1.000000000000000000, 0.9510565162951535312, 1.000000000000000000, 0.9510565162951535312, 1.000000000000000000, 0.9510565162951535312, 1.000000000000000000, 0.9510565162951535312, 1.000000000000000000, 0.9510565162951535312, 1.000000000000000000, 0.9510565162951535312, 1.000000000000000000, 0.9510565162951535312, 1.000000000000000000, 0.9510565162951535312, 1.000000000000000000, 0.9510565162951535312, 1.000000000000000000, 0.9510565162951535312, 1.000000000000000000, 0.9510565162951535312, 1.000000000000000000, 0.9510565162951535312, 1.000000000000000000, 0.9510565162951535312, 1.000000000000000000, 0.9510565162951535312, 1.000000000000000000, 0.9510565162951535312, 1.000000000000000000, 0.9510565162951535312, 1.000000000000000000, 0.9510565162951535312, 1.000000000000000000, 0.9510565162951535312, 1.000000000000000000, 0.9510565162951535312, 1.000000000000000000, 0.9510565162951535312, 1.000000000000000000, 0.9510565162951535312, 1.000000000000000000, 0.9510565162951535312, 1.000000000000000000, 0.9510565162951535312, 1.000000000000000000, 0.9510565162951535312, 1.000000000000000000, 0.9510565162951535312, 1.000000000000000000, 0.9510565162951535312, 1.000000000000000000, 0.9510565162951535312, 1.000000000000000000, 0.9510565162951535312, 1.000000000000000000, 0.9510565162951535312, 1.000000000000000000, 0.9510565162951535312, 1.000000000000000000, 0.9510565162951535312, 1.000000000000000000, 0.9510565162951535312, 1.000000000000000000, 0.9510565162951535312, 1.000000000000000000, 0.9510565162951535312, 1.000000000000000000, 0.9510565162951535312, 1.000000000000000000, 0.9510565162951535312, 1.000000000000000000, 0.9510565162951535312, 1.000000000000000000, 0.9510565162951535312, 1.000000000000000000, 0.9510565162951535312, 1.000000000000000000, 0.9510565162951535312, 1.000000000000000000, 0.9510565162951535312, 1.000000000000000000, 0.9510565162951535312, 1.000000000000000000, 0.9510565162951535312, 1.000000000000000000, 0.9510565162951535312, 1.000000000000000000, 0.9510565162951535312, 1.000000000000000000, 0.9510565162951535312, 1.000000000000000000, 0.9510565162951535312, 1.000000000000000000, 0.9510565162951535312, 1.000000000000000000, 0.9510565162951535312, 1.000000000000000000, 0.9510565162951535312, 1.000000000000000000, 0.9510565162951535312, 1.000000000000000000, 0.9510565162951535312, 1.000000000000000000, 0.9510565162951535312, 1.000000000000000000, 0.9510565162951535312, 1.000000000000000000, 0.9510565162951535312, 1.000000000000000000, 0.9510565162951535312, 1.000000000000000000, 0.9510565162951535312, 1.000000000000000000, 0.9510565162951535312, 1.000000000000000000, 0.9510565162951535312, 1.000000000000000000, 0.9510565162951535312, 1.000000000000000000, 0.9510565162951535312, 1.000000000000000000, 0.9510565162951535312, 1.000000000000000000, 0.9510565162951535312, 1.000000000000000000, 0.9510565162951535312, 1.000000000000000000, 0.9510565162951535312, 1.000000000000000000, 0.9510565162951535312, 1.000000000000000000, 0.9510565162951535312, 1.000000000000000000, 0.9510565162951535312, 1.000000000000000000, 0.9510565162951535312, 1.000000000000000000, 0.9510565162951535312, 1.000000000000000000, 0.9510565162951535312, 1.000000000000000000, 0.9510565162951535312, 1.000000000000000000, 0.9510565162951535312, 1.000000000000000000, 0.9510565162951535312, 1.000000000000000000, 0.9510565162951535312, 1.000000000000000000, 0.9510565162951535312, 1.000000000000000000, 0.9510565162951535312, 1.000000000000000000, 0.9510565162951535312, 1.000000000000000000, 0.9510565162951535312, 1.000000000000000000, 0.9510565162951535312, 1.000000000000000000, 0.9510565162951535312, 1.000000000000000000, 0.9510565162951535312, 1.000000000000000000, 0.9510565162951535312, 1.000000000000000000, 0.9510565162951535312, 1.000000000000000000, 0.9510565162951535312, 1.000000000000000000, 0.9510565162951535312, 1.000000000000000000, 0.9510565162951535312, 1.000000000000000000, 0.9510565162951535312, 1.000000000000000000, 0.9510565162951535312, 1.000000000000000000, 0.9510565162951535312, 1.000000000000000000, 0.9510565162951535312, 1.000000000000000000, 0.9510565162951535312, 1.000000000000000000, 0.9510565162951535312, 1.000000000000000000, 0.9510565162951535312, 1.000000000000000000, 0.9510565162951535312, 1.000000000000000000, 0.9510565162951535312, 1.000000000000000000, 0.9510565162951535312, 1.000000000000000000, 0.9510565162951535312, 1.000000000000000000, 0.9510565162951535312, 1.000000000000000000, 0.9510565162951535312, 1.000000000000000000, 0.9510565162951535312, 1.000000000000000000, 0.9510565162951535312, 1.000000000000000000, 0.9510565162951535312, 1.000000000000000000, 0.9510565162951535312, 1.000000000000000000, 0.9510565162951535312, 1.000000000000000000, 0.9510565162951535312, 1.000000000000000000, 0.9510565162951535312, 1.000000000000000000, 0.9510565162951535312, 1.000000000000000000, 0.9510565162951535312, 1.000000000000000000, 0.9510565162951535312, 1.000000000000000000, 0.9510565162951535312, 1.000000000000000000, 0.9510565162951535312, 1.000000000000000000, 0.9510565162951535312, 1.000000000000000000, 0.9510565162951535312, 1.000000000000000000, 0.9510565162951535312, 1.000000000000000000, 0.9510565162951535312, 1.000000000000000000, 0.9510565162951535312, 1.000000000000000000, 0.9510565162951535312, 1.000000000000000000, 0.9510565162951535312, 1.000000000000000000, 0.9510565162951535312, 1.000000000000000000, 0.9510565162951535312, 1.000000000000000000, 0.9510565162951535312, 1.000000000000000000, 0.9510565162951535312, 1.000000000000000000, 0.9510565162951535312, 1.000000000000000000, 0.9510565162951535312, 1.000000000000000000, 0.9510565162951535312, 1.000000000000000000, 0.9510565162951535312, 1.000000000000000000, 0.9510565162951535312, 1.000000000000000000, 0.9510565162951535312, 1.000000000000000000, 0.9510565162951535312, 1.000000000000000000, 0.9510565162951535312, 1.000000000000000000, 0.9510565162951535312, 1.000000000000000000, 0.9510565162951535312, 1.000000000000000000, 0.9510565162951535312, 1.000000000000000000, 0.9510565162951535312, 1.000000000000000000, 0.9510565162951535312, 1.000000000000000000, 0.9510565162951535312, 1.000000000000000000, 0.9510565162951535312, 1.000000000000000000, 0.9510565162951535312, 1.000000000000000000, 0.9510565162951535312, 1.000000000000000000, 0.9510565162951535312, 1.000000000000000000, 0.9510565162951535312, 1.000000000000000000, 0.9510565162951535312, 1.000000000000000000, 0.9510565162951535312, 1.000000000000000000, 0.9510565162951535312, 1.000000000000000000, 0.9510565162951535312, 1.000000000000000000, 0.9510565162951535312, 1.000000000000000000, 0.9510565162951535312, 1.000000000000000000, 0.9510565162951535312, 1.000000000000000000, 0.9510565162951535312, 1.000000000000000000, 0.9510565162951535312, 1.000000000000000000, 0.9510565162951535312, 1.000000000000000000, 0.9510565162951535312, 1.000000000000000000, 0.9510565162951535312, 1.000000000000000000, 0.9510565162951535312, 1.000000000000000000, 0.9510565162951535312, 1.000000000000000000, 0.9510565162951535312, 1.000000000000000000, 0.9510565162951535312, 1.000000000000000000, 0.9510565162951535312, 1.000000000000000000, 0.9510565162951535312, 1.000000000000000000, 0.9510565162951535312, 1.000000000000000000, 0.9510565162951535312, 1.000000000000000000, 0.9510565162951535312, 1.000000000000000000, 0.9510565162951535312, 1.000000000000000000, 0.9510565162951535312, 1.000000000000000000, 0.9510565162951535312, 1.000000000000000000, 0.9510565162951535312, 1.000000000000000000, 0.9510565162951535312, 1.000000000000000000, 0.9510565162951535312, 1.000000000000000000, 0.9510565162951535312, 1.000000000000000000, 0.9510565162951535312, 1.000000000000000000, 0.9510565162951535312, 1.000000000000000000, 0.9510565162951535312, 1.000000000000000000, 0.9510565162951535312, 1.000000000000000000, 0.9510565162951535312, 1.000000000000000000, 0.9510565162951535312, 1.000000000000000000, 0.9510565162951535312, 1.000000000000000000, 0.9510565162951535312, 1.000000000000000000, 0.9510565162951535312, 1.000000000000000000, 0.9510565162951535312, 1.000000000000000000, 0.9510565162951535312, 1.000000000000000000, 0.9510565162951535312, 1.000000000000000000, 0.9510565162951535312, 1.000000000000000000, 0.9510565162951535312, 1.000000000000000000, 0.9510565162951535312, 1.000000000000000000, 0.9510565162951535312, 1.000000000000000000, 0.9510565162951535312, 1.000000000000000000, 0.9510565162951535312, 1.000000000000000000, 0.9510565162951535312, 1.000000000000000000, 0.9510565162951535312, 1.000000000000000000, 0.9510565162951535312, 1.000000000000000000, 0.9510565162951535312, 1.000000000000000000, 0.9510565162951535312, 1.000000000000000000, 0.9510565162951535312, 1.000000000000000000, 0.9510565162951535312, 1.000000000000000000, 0.9510565162951535312, 1.000000000000000000, 0.9510565162951535312, 1.000000000000000000, 0.9510565162951535312, 1.000000000000000000, 0.9510565162951535312, 1.000000000000000000, 0.9510565162951535312, 1.000000000000000000, 0.9510565162951535312, 1.000000000000000000, 0.9510565162951535312, 1.000000000000000000, 0.9510565162951535312, 1.000000000000000000, 0.9510565162951535312, 1.000000000000000000, 0.9510565162951535312, 1.000000000000000000, 0.9510565162951535312, 1.000000000000000000, 0.9510565162951535312, 1.000000000000000000, 0.9510565162951535312, 1.000000000000000000, 0.9510565162951535312, 1.000000000000000000, 0.9510565162951535312, 1.000000000000000000, 0.9510565162951535312, 1.000000000000000000, 0.9510565162951535312, 1.000000000000000000, 0.9510565162951535312, 1.000000000000000000, 0.9510565162951535312, 1.000000000000000000, 0.9510565162951535312, 1.000000000000000000, 0.9510565162951535312, 1.000000000000000000, 0.9510565162951535312, 1.000000000000000000, 0.9510565162951535312, 1.000000000000000000, 0.9510565162951535312, 1.000000000000000000, 0.9510565162951535312, 1.000000000000000000, 0.9510565162951535312, 1.000000000000000000, 0.9510565162951535312, 1.000000000000000000, 0.9510565162951535312, 1.000000000000000000, 0.9510565162951535312, 1.000000000000000000, 0.9510565162951535312, 1.000000000000000000, 0.9510565162951535312, 1.000000000000000000, 0.9510565162951535312, 1.000000000000000000, 0.9510565162951535312, 1.000000000000000000, 0.9510565162951535312, 1.000000000000000000, 0.9510565162951535312, 1.000000000000000000, 0.9510565162951535312, 1.000000000000000000, 0.9510565162951535312, 1.000000000000000000, 0.9510565162951535312, 1.000000000000000000, 0.9510565162951535312, 1.000000000000000000, 0.9510565162951535312, 1.000000000000000000, 0.9510565162951535312, 1.000000000000000000, 0.9510565162951535312, 1.000000000000000000, 0.9510565162951535312, 1.000000000000000000, 0.9510565162951535312, 1.000000000000000000, 0.9510565162951535312, 1.000000000000000000, 0.9695511069847947416, 0.9769881597858905975 ) ) 
 REPRESENTATION_ITEM ( '' )  );
#9649 = CARTESIAN_POINT ( 'NONE',  ( 11.98450388067348271, 203.0532714938637753, 86.15113791807856103 ) ) ;
#9650 = CARTESIAN_POINT ( 'NONE',  ( 82.71132485994282035, 155.0000000000000000, 15.00000000000001243 ) ) ;
#9651 = AXIS2_PLACEMENT_3D ( 'NONE', #16661, #831, #11221 ) ;
#9652 = CARTESIAN_POINT ( 'NONE',  ( 8.062137200540920645, 201.0835637161417822, 5.301137918078566713 ) ) ;
#9653 = CARTESIAN_POINT ( 'NONE',  ( 10.00000000000000711, 207.0476921513415220, 69.99886208192143044 ) ) ;
#9654 = B_SPLINE_CURVE_WITH_KNOTS ( 'NONE', 3,
 ( #28429, #13090, #7817, #28598, #15480, #31150, #26198, #146, #12757, #18207 ),
 .UNSPECIFIED., .F., .F.,
 ( 4, 2, 2, 2, 4 ),
 ( 0.000000000000000000, 0.001989602278884365291, 0.003979204557768730582, 0.005968806836653095874, 0.007958409115537461165 ),
 .UNSPECIFIED. ) ;
#9655 = STYLED_ITEM ( 'NONE', ( #26499 ), #23982 ) ;
#9656 = FACE_BOUND ( 'NONE', #8736, .T. ) ;
#9657 = VERTEX_POINT ( 'NONE', #25385 ) ;
#9658 = CARTESIAN_POINT ( 'NONE',  ( 9.680171189290716072, 214.0920067884432854, 75.69886208192143329 ) ) ;
#9659 = ORIENTED_EDGE ( 'NONE', *, *, #13733, .F. ) ;
#9660 = CARTESIAN_POINT ( 'NONE',  ( 77.17499999726881299, 145.8408176439707802, -12.60653300113719588 ) ) ;
#9661 = CARTESIAN_POINT ( 'NONE',  ( -4.903702542908436435, 200.1653181626580249, 56.04886208192144181 ) ) ;
#9662 = ORIENTED_EDGE ( 'NONE', *, *, #14952, .F. ) ;
#9663 = VECTOR ( 'NONE', #30220, 1000.000000000000000 ) ;
#9664 = CARTESIAN_POINT ( 'NONE',  ( 80.77499999726880731, 140.1801316387863778, 4.815267126137185549 ) ) ;
#9665 = CARTESIAN_POINT ( 'NONE',  ( 6.500000000000000000, 3.752776749732563921, -8.000000000000000000 ) ) ;
#9666 = CARTESIAN_POINT ( 'NONE',  ( -58.50000000000002132, 194.9217985566782829, -2.500000000000000000 ) ) ;
#9667 = CARTESIAN_POINT ( 'NONE',  ( 56.02499999726880731, 160.0630714827496206, 15.58253174999999402 ) ) ;
#9668 = CARTESIAN_POINT ( 'NONE',  ( 3.999999999999999112, 0.000000000000000000, 3.469446951953614189E-15 ) ) ;
#9669 = CARTESIAN_POINT ( 'NONE',  ( -0.05014649552828403384, 217.5146222423826714, 45.24886208192143755 ) ) ;
#9670 = ORIENTED_EDGE ( 'NONE', *, *, #31256, .T. ) ;
#9671 = DIRECTION ( 'NONE',  ( -1.000000000000000000, 0.000000000000000000, 0.000000000000000000 ) ) ;
#9672 =( NAMED_UNIT ( * ) SI_UNIT ( $, .STERADIAN. ) SOLID_ANGLE_UNIT ( ) );
#9673 = CARTESIAN_POINT ( 'NONE',  ( -63.49999999999884892, 215.0000000000003979, 0.000000000000000000 ) ) ;
#9674 = DIRECTION ( 'NONE',  ( 0.000000000000000000, -0.4999999999999993339, 0.8660254037844389297 ) ) ;
#9675 = CARTESIAN_POINT ( 'NONE',  ( 4.903702542908435547, 213.8346818373419751, 21.54886208192143471 ) ) ;
#9676 = AXIS2_PLACEMENT_3D ( 'NONE', #18577, #32012, #28961 ) ;
#9677 = CARTESIAN_POINT ( 'NONE',  ( -3.135527875058821579, 197.5041725223112223, 59.90113791807856813 ) ) ;
#9678 = EDGE_CURVE ( 'NONE', #18054, #26344, #11940, .T. ) ;
#9679 = CARTESIAN_POINT ( 'NONE',  ( 8.118202686958039038, 212.8392687619912635, 46.70113791807857240 ) ) ;
#9680 = ITEM_DEFINED_TRANSFORMATION ( 'NONE', 'NONE', #8304,  #2404 ) ;
#9681 = CARTESIAN_POINT ( 'NONE',  ( 9.984503880673470277, 203.7031108863295401, 14.15113791807856458 ) ) ;
#9682 = CARTESIAN_POINT ( 'NONE',  ( 0.05014649552807626948, 215.4116977939061144, 4.251137918078566891 ) ) ;
#9683 = CARTESIAN_POINT ( 'NONE',  ( 51.02499999726880731, 149.9369285172503510, -15.58253175000000823 ) ) ;
#9684 =( NAMED_UNIT ( * ) SI_UNIT ( $, .STERADIAN. ) SOLID_ANGLE_UNIT ( ) );
#9685 = CARTESIAN_POINT ( 'NONE',  ( 87.50000000000000000, 160.9457742543943652, -14.40357817542362540 ) ) ;
#9686 = CARTESIAN_POINT ( 'NONE',  ( -9.736236675707914401, 199.9851607334237542, 33.20113791807856529 ) ) ;
#9687 = CARTESIAN_POINT ( 'NONE',  ( 58.50000000000001421, -88.00000000000000000, 30.00000000000000000 ) ) ;
#9688 = CARTESIAN_POINT ( 'NONE',  ( 8.062137200540920645, 201.0835637161417822, 80.30113791807858092 ) ) ;
#9689 = CARTESIAN_POINT ( 'NONE',  ( 9.984503880673473830, 203.7031108863295401, 50.15113791807856813 ) ) ;
#9690 = UNCERTAINTY_MEASURE_WITH_UNIT (LENGTH_MEASURE( 1.000000000000000082E-05 ), #16325, 'distance_accuracy_value', 'NONE');
#9691 = AXIS2_PLACEMENT_3D ( 'NONE', #7358, #2069, #4626 ) ;
#9692 = CYLINDRICAL_SURFACE ( 'NONE', #25171, 15.00000000000001776 ) ;
#9693 = CARTESIAN_POINT ( 'NONE',  ( 41.71132485994280614, 155.0000000000000000, -15.00000000000002487 ) ) ;
#9694 = CARTESIAN_POINT ( 'NONE',  ( -0.05014649552828442242, 219.6175466908591716, 15.24886208192143577 ) ) ;
#9695 = CARTESIAN_POINT ( 'NONE',  ( 3.044812012439969795, 216.5253028482143520, 18.39886208192143613 ) ) ;
#9696 = CARTESIAN_POINT ( 'NONE',  ( 71.59999999453762598, 141.2096805137202580, -4.480746418436742040 ) ) ;
#9697 = VERTEX_POINT ( 'NONE', #29998 ) ;
#9698 = CARTESIAN_POINT ( 'NONE',  ( -3.753561863808691168, 195.6020594897209435, 56.90113791807858235 ) ) ;
#9699 = CARTESIAN_POINT ( 'NONE',  ( -0.05014649552807731031, 198.5883022060938572, 80.75113791807856956 ) ) ;
#9700 = CARTESIAN_POINT ( 'NONE',  ( -3.135527875058982783, 216.4958274776886924, 39.09886208192143187 ) ) ;
#9701 = DIRECTION ( 'NONE',  ( 1.000000000000000000, -0.000000000000000000, -0.000000000000000000 ) ) ;
#9702 = ORIENTED_EDGE ( 'NONE', *, *, #24915, .F. ) ;
#9703 = ORIENTED_EDGE ( 'NONE', *, *, #22723, .F. ) ;
#9704 = B_SPLINE_CURVE_WITH_KNOTS ( 'NONE', 3,
 ( #19317, #9264, #1428, #16923, #32762, #16759 ),
 .UNSPECIFIED., .F., .F.,
 ( 4, 2, 4 ),
 ( 0.005649496001316489831, 0.006672230966438345498, 0.007694965931560201165 ),
 .UNSPECIFIED. ) ;
#9705 = AXIS2_PLACEMENT_3D ( 'NONE', #9991, #12705, #25993 ) ;
#9706 = ORIENTED_EDGE ( 'NONE', *, *, #4528, .F. ) ;
#9707 = PRODUCT ( 'pad', 'pad', '', ( #514 ) ) ;
#9708 = AXIS2_PLACEMENT_3D ( 'NONE', #1657, #27050, #22104 ) ;
#9709 = CARTESIAN_POINT ( 'NONE',  ( 58.38867513459481984, 140.7341522555726669, -4.635254915624220651 ) ) ;
#9710 = CYLINDRICAL_SURFACE ( 'NONE', #6190, 40.00000000000000711 ) ;
#9711 = ORIENTED_EDGE ( 'NONE', *, *, #33130, .T. ) ;
#9712 = CARTESIAN_POINT ( 'NONE',  ( 4.984841277089725686, 213.7757310962907411, 34.55113791807856671 ) ) ;
#9713 = CARTESIAN_POINT ( 'NONE',  ( 55.51132485994280330, 146.1832212156128890, -12.13525491562423042 ) ) ;
#9714 = CARTESIAN_POINT ( 'NONE',  ( -3.135527875058982783, 216.4958274776886924, 9.098862081921435419 ) ) ;
#9715 = CARTESIAN_POINT ( 'NONE',  ( 59.17499999726881299, 145.8408176439707802, -12.60653300113719588 ) ) ;
#9717 = ORIENTED_EDGE ( 'NONE', *, *, #1435, .F. ) ;
#9716 = AXIS2_PLACEMENT_3D ( 'NONE', #30775, #2158, #28216 ) ;
#9718 = CARTESIAN_POINT ( 'NONE',  ( 4.984841277089725686, 213.7757310962907411, 46.55113791807856671 ) ) ;
#9719 = CARTESIAN_POINT ( 'NONE',  ( 66.81132485994281467, 150.1262045565066785, 15.00000000000020250 ) ) ;
#9720 = CARTESIAN_POINT ( 'NONE',  ( 56.91132485994280898, 146.1832212156128890, 12.13525491562421976 ) ) ;
#9721 = CARTESIAN_POINT ( 'NONE',  ( 10.01549611932659545, 203.7984951890123853, 97.14886208192145034 ) ) ;
#9722 = CARTESIAN_POINT ( 'NONE',  ( 67.07499999726880446, 141.7447067706911810, -9.630534252274385310 ) ) ;
#9723 = CARTESIAN_POINT ( 'NONE',  ( -8.118202686958039038, 201.1607312380087080, 33.20113791807857240 ) ) ;
#9724 = CARTESIAN_POINT ( 'NONE',  ( 70.28867513459482552, 139.2280666364260071, -4.041636747397287284E-15 ) ) ;
#9725 = EDGE_CURVE ( 'NONE', #534, #14229, #20109, .T. ) ;
#9726 = CARTESIAN_POINT ( 'NONE',  ( -6.139770520408369237, 215.5359834540460042, 21.95113791807856884 ) ) ;
#9727 = DIRECTION ( 'NONE',  ( 1.000000000000000000, 0.000000000000000000, 0.000000000000000000 ) ) ;
#9728 = CARTESIAN_POINT ( 'NONE',  ( 77.50000000000001421, 155.0000000000000000, 14.49999999999999467 ) ) ;
#9729 = CARTESIAN_POINT ( 'NONE',  ( -56.12712552280034117, 194.9922069576863066, 0.8039670099889266730 ) ) ;
#9730 = DIRECTION ( 'NONE',  ( 0.000000000000000000, -1.000000000000000000, 0.000000000000000000 ) ) ;
#9731 = CARTESIAN_POINT ( 'NONE',  ( 12.00000000000000711, 206.9523078486586485, -0.9988620819214344415 ) ) ;
#9732 = AXIS2_PLACEMENT_3D ( 'NONE', #13338, #26613, #14003 ) ;
#9733 = CARTESIAN_POINT ( 'NONE',  ( 48.48867513459482836, 142.2402378747194405, -9.270509831248439525 ) ) ;
#9734 = CARTESIAN_POINT ( 'NONE',  ( 51.57499999726881157, 164.1591823560292198, -12.60653300113719766 ) ) ;
#9735 = CARTESIAN_POINT ( 'NONE',  ( -9.984503880673473830, 210.2968891136704315, 48.65113791807858235 ) ) ;
#9736 = CARTESIAN_POINT ( 'NONE',  ( 81.72499999726881015, 169.8198683612136222, 4.815267126137181997 ) ) ;
#9737 = EDGE_CURVE ( 'NONE', #25250, #355, #15611, .T. ) ;
#9738 = TOROIDAL_SURFACE ( 'NONE', #23338, 70.00000000000001421, 30.00000000000000000 ) ;
#9739 = CARTESIAN_POINT ( 'NONE',  ( 42.21132485994281325, 170.7719333635740497, -7.904646289410545231E-15 ) ) ;
#9740 = CARTESIAN_POINT ( 'NONE',  ( 10.01549611932659367, 203.7984951890124421, 28.14886208192144323 ) ) ;
#9741 = CARTESIAN_POINT ( 'NONE',  ( 77.50000000000000000, 155.0000000000000000, -6.938893903907228378E-15 ) ) ;
#9742 = CARTESIAN_POINT ( 'NONE',  ( 53.69999999453762030, 142.6655632788954620, -8.961492836873480528 ) ) ;
#9743 = ORIENTED_EDGE ( 'NONE', *, *, #21984, .T. ) ;
#9744 = CARTESIAN_POINT ( 'NONE',  ( 11.98450388067348271, 203.0532714938637753, 32.15113791807856103 ) ) ;
#9745 = DIRECTION ( 'NONE',  ( -0.1045284632676468234, 0.000000000000000000, 0.9945218953682740670 ) ) ;
#9746 = CARTESIAN_POINT ( 'NONE',  ( 12.01549611932659367, 203.1486557965466773, 103.1488620819214361 ) ) ;
#9747 = AXIS2_PLACEMENT_3D ( 'NONE', #15340, #8018, #2571 ) ;
#9748 = CARTESIAN_POINT ( 'NONE',  ( 3.399999999999999911, 0.000000000000000000, -7.554475477074173106 ) ) ;
#9749 = ORIENTED_EDGE ( 'NONE', *, *, #15399, .F. ) ;
#9750 = CARTESIAN_POINT ( 'NONE',  ( -6.139770520408369237, 215.5359834540460042, 0.9511379180785658471 ) ) ;
#9751 = CARTESIAN_POINT ( 'NONE',  ( -6.139770520408369237, 215.5359834540460042, 60.95113791807857950 ) ) ;
#9752 = EDGE_CURVE ( 'NONE', #5220, #29148, #24306, .T. ) ;
#9753 = EDGE_LOOP ( 'NONE', ( #9078, #567 ) ) ;
#9754 = CARTESIAN_POINT ( 'NONE',  ( 7.984503880673422316, 209.6470497212048372, 24.84886208192143897 ) ) ;
#9755 = DIRECTION ( 'NONE',  ( 0.000000000000000000, -1.000000000000000000, 0.000000000000000000 ) ) ;
#9756 = ORIENTED_EDGE ( 'NONE', *, *, #30533, .T. ) ;
#9757 = CARTESIAN_POINT ( 'NONE',  ( -8.000000000000008882, 207.0476921513413515, 3.501137918078566003 ) ) ;
#9758 = CIRCLE ( 'NONE', #31524, 13.00000000000001066 ) ;
#9759 = EDGE_CURVE ( 'NONE', #9440, #13631, #17804, .T. ) ;
#9760 = CARTESIAN_POINT ( 'NONE',  ( 0.000000000000000000, 0.000000000000000000, 0.000000000000000000 ) ) ;
#9761 = CARTESIAN_POINT ( 'NONE',  ( 9.736236675708031640, 199.9851607334238963, 88.29886208192142760 ) ) ;
#9762 = CARTESIAN_POINT ( 'NONE',  ( 37.17499999726881299, 145.8408176439707802, -12.60653300113719588 ) ) ;
#9763 = ORIENTED_EDGE ( 'NONE', *, *, #4596, .T. ) ;
#9764 = CARTESIAN_POINT ( 'NONE',  ( 45.22499999726881015, 160.0630714827496206, -15.58253175000000823 ) ) ;
#9765 = CARTESIAN_POINT ( 'NONE',  ( 8.399999999999998579, 0.000000000000000000, 0.000000000000000000 ) ) ;
#9766 = CARTESIAN_POINT ( 'NONE',  ( 54.41132485994280188, 167.7597621252805880, 9.270509831248428867 ) ) ;
#9767 = CARTESIAN_POINT ( 'NONE',  ( 3.135527875058981895, 197.5041725223112792, 73.59886208192143897 ) ) ;
#9768 = CARTESIAN_POINT ( 'NONE',  ( 49.67499999726879878, 168.2552932293087906, -9.630534252274385310 ) ) ;
#9769 = DIRECTION ( 'NONE',  ( -1.000000000000000000, 0.000000000000000000, 0.000000000000000000 ) ) ;
#9770 = CARTESIAN_POINT ( 'NONE',  ( 8.062137200540920645, 201.0835637161417822, 8.301137918078566713 ) ) ;
#9771 = LINE ( 'NONE', #16619, #5607 ) ;
#9772 = CARTESIAN_POINT ( 'NONE',  ( 60.70000000000000284, 163.5228861582408797, -11.73074641843674470 ) ) ;
#9773 = CARTESIAN_POINT ( 'NONE',  ( -8.118202686958039038, 201.1607312380087080, 93.20113791807857240 ) ) ;
#9774 = CARTESIAN_POINT ( 'NONE',  ( 64.61132485994281183, 159.8737954434938615, 14.99999999999982592 ) ) ;
#9775 = CARTESIAN_POINT ( 'NONE',  ( 6.139770520408368348, 198.4640165459539674, 77.45113791807854398 ) ) ;
#9776 = CARTESIAN_POINT ( 'NONE',  ( -5.276498195231978272, 6.073236878017963747, -7.633618187056680604 ) ) ;
#9777 = FACE_OUTER_BOUND ( 'NONE', #1325, .T. ) ;
#9778 = CARTESIAN_POINT ( 'NONE',  ( 12.00000000000000711, 207.0476921513415220, 90.99886208192144466 ) ) ;
#9779 = CARTESIAN_POINT ( 'NONE',  ( 66.62499999726881583, 138.6155565068815463, -3.929120461958505118E-15 ) ) ;
#9781 = ORIENTED_EDGE ( 'NONE', *, *, #14945, .F. ) ;
#9780 = CARTESIAN_POINT ( 'NONE',  ( 3.044812012440130555, 197.4746971517856764, 32.60113791807857098 ) ) ;
#9782 = FACE_OUTER_BOUND ( 'NONE', #27679, .T. ) ;
#9783 = CARTESIAN_POINT ( 'NONE',  ( 87.17499999726881299, 145.8408176439707802, -12.60653300113719588 ) ) ;
#9784 = CARTESIAN_POINT ( 'NONE',  ( -0.05014649552807705357, 194.3824533091408000, 89.75113791807858377 ) ) ;
#9785 = EDGE_CURVE ( 'NONE', #73, #29143, #8244, .T. ) ;
#9786 = ADVANCED_FACE ( 'NONE', ( #19772 ), #6825, .T. ) ;
#9787 = DIRECTION ( 'NONE',  ( -1.000000000000000000, -0.000000000000000000, -0.000000000000000000 ) ) ;
#9788 = ORIENTED_EDGE ( 'NONE', *, *, #14980, .T. ) ;
#9789 = CARTESIAN_POINT ( 'NONE',  ( -12.01549611932659722, 210.8513442034533227, 68.64886208192142192 ) ) ;
#9790 = CARTESIAN_POINT ( 'NONE',  ( 6.220909254589680693, 198.5229672870052582, 88.44886208192144750 ) ) ;
#9791 = CARTESIAN_POINT ( 'NONE',  ( -3.662846001189865142, 195.5725841191952838, 13.89886208192143613 ) ) ;
#9792 = CARTESIAN_POINT ( 'NONE',  ( 115.4999999999999858, 257.3881375866408803, -27.43481878086871717 ) ) ;
#9793 = CARTESIAN_POINT ( 'NONE',  ( -0.05014649552810635652, 196.4853777576173002, 29.75113791807856956 ) ) ;
#9794 = CARTESIAN_POINT ( 'NONE',  ( -3.096526599377909417, 6.872473572140716414, 1.143494478793305063E-15 ) ) ;
#9795 = ADVANCED_FACE ( 'NONE', ( #14658 ), #7482, .T. ) ;
#9796 = CARTESIAN_POINT ( 'NONE',  ( -10.00000000000000711, 206.9523078486584495, 98.49886208192143044 ) ) ;
#9797 = DIRECTION ( 'NONE',  ( -0.9945218953682777308, 1.280104479604737106E-17, -0.1045284632676128089 ) ) ;
#9798 = ORIENTED_EDGE ( 'NONE', *, *, #15338, .T. ) ;
#9799 = DIRECTION ( 'NONE',  ( -0.7071067811865355823, 0.000000000000000000, 0.7071067811865595631 ) ) ;
#9800 = CARTESIAN_POINT ( 'NONE',  ( 2.426778023690075337, 214.6231898156240447, 78.39886208192143613 ) ) ;
#9801 = EDGE_CURVE ( 'NONE', #3092, #26053, #14821, .T. ) ;
#9802 = EDGE_LOOP ( 'NONE', ( #4718, #4086, #17440, #4554 ) ) ;
#9803 = B_SPLINE_CURVE_WITH_KNOTS ( 'NONE', 3,
 ( #4758, #23329, #4312, #1867 ),
 .UNSPECIFIED., .F., .F.,
 ( 4, 4 ),
 ( 0.0001200665308319763828, 0.0006294823820153499106 ),
 .UNSPECIFIED. ) ;
#9804 = CARTESIAN_POINT ( 'NONE',  ( 2.000000000000000000, 1.773042676681340968, -2.276824562219559311E-15 ) ) ;
#9805 = VERTEX_POINT ( 'NONE', #25219 ) ;
#9806 = CARTESIAN_POINT ( 'NONE',  ( -67.50000000000000000, 155.0000000000000000, 6.938893903907228378E-15 ) ) ;
#9807 = B_SPLINE_CURVE_WITH_KNOTS ( 'NONE', 3,
 ( #25232, #9227, #1895, #12282, #22674, #20119 ),
 .UNSPECIFIED., .F., .F.,
 ( 4, 2, 4 ),
 ( -4.604908129291797664E-06, 0.0003318387708545240283, 0.0006682824498383398322 ),
 .UNSPECIFIED. ) ;
#9808 = CARTESIAN_POINT ( 'NONE',  ( 73.57499999726880446, 164.1591823560292198, -12.60653300113719766 ) ) ;
#9809 = CARTESIAN_POINT ( 'NONE',  ( 82.52499999726880731, 140.1801316387863778, 4.815267126137185549 ) ) ;
#9810 = DIRECTION ( 'NONE',  ( 1.000000000000000000, 0.000000000000000000, 0.000000000000000000 ) ) ;
#9811 =( BOUNDED_CURVE ( )  B_SPLINE_CURVE ( 2, ( #9650, #25149, #1989, #25323, #17485, #21799, #14137, #30445, #1815, #17824, #7105 ),
 .UNSPECIFIED., .F., .T. ) 
 B_SPLINE_CURVE_WITH_KNOTS ( ( 3, 2, 2, 2, 2, 3 ),
 ( 0.8750000000000001110, 0.8785714285714286698, 0.8821428571428572285, 0.8857142857142856762, 0.8892857142857142350, 0.8928571428571429047 ),
 .UNSPECIFIED. ) 
 CURVE ( )  GEOMETRIC_REPRESENTATION_ITEM ( )  RATIONAL_B_SPLINE_CURVE ( ( 0.9999999999999984457, 0.9510565162951549745, 1.000000000000000000, 0.9510565162951534202, 1.000000000000000000, 0.9510565162951534202, 1.000000000000000000, 0.9510565162951534202, 1.000000000000000000, 0.9510565162951534202, 1.000000000000000000 ) ) 
 REPRESENTATION_ITEM ( '' )  );
#9812 = CARTESIAN_POINT ( 'NONE',  ( -0.05014649552807731031, 198.5883022060938572, 77.75113791807856956 ) ) ;
#9813 = CARTESIAN_POINT ( 'NONE',  ( 117.5000000000000142, 155.0000000000000000, 70.00000000000000000 ) ) ;
#9814 =( NAMED_UNIT ( * ) SI_UNIT ( $, .STERADIAN. ) SOLID_ANGLE_UNIT ( ) );
#9815 = CARTESIAN_POINT ( 'NONE',  ( 44.50000000000000000, 155.0000000000000000, -14.50000000000000711 ) ) ;
#9816 = CARTESIAN_POINT ( 'NONE',  ( 4.984841277089891776, 200.2242689037093726, 52.44886208192144039 ) ) ;
#9817 = CARTESIAN_POINT ( 'NONE',  ( -63.50000000000001421, 210.0000000000000000, -3.061616997868383141E-16 ) ) ;
#9818 = CARTESIAN_POINT ( 'NONE',  ( 127.5000000000000000, 80.04668119422552763, -74.95331880577366235 ) ) ;
#9819 = FACE_OUTER_BOUND ( 'NONE', #2649, .T. ) ;
#9820 = CARTESIAN_POINT ( 'NONE',  ( 58.52499999726881441, 140.1801316387863778, 4.815267126137185549 ) ) ;
#9821 = CARTESIAN_POINT ( 'NONE',  ( 63.77499999726880731, 169.8198683612136222, -4.815267126137197984 ) ) ;
#9822 = CARTESIAN_POINT ( 'NONE',  ( 12.01549611932652972, 210.8513442034534933, 55.85113791807856387 ) ) ;
#9823 = DIRECTION ( 'NONE',  ( 0.000000000000000000, 0.000000000000000000, -1.000000000000000000 ) ) ;
#9824 = CARTESIAN_POINT ( 'NONE',  ( -7.375838497908182134, 217.2372850707499765, 3.951137918078565736 ) ) ;
#9825 = EDGE_CURVE ( 'NONE', #10137, #18787, #1884, .T. ) ;
#9826 = CARTESIAN_POINT ( 'NONE',  ( -9.984503880673475606, 210.2968891136704315, 75.65113791807857524 ) ) ;
#9827 = AXIS2_PLACEMENT_3D ( 'NONE', #11231, #3732, #24515 ) ;
#9828 = CARTESIAN_POINT ( 'NONE',  ( -3.662846001189865142, 195.5725841191952838, 37.89886208192143613 ) ) ;
#9829 = CARTESIAN_POINT ( 'NONE',  ( -9.984503880673420539, 203.7031108863293980, 44.34886208192143187 ) ) ;
#9830 = CARTESIAN_POINT ( 'NONE',  ( -6.500000000000000000, 3.149025070564754003, -0.5705737632551073357 ) ) ;
#9831 = CARTESIAN_POINT ( 'NONE',  ( -11.98450388067348804, 210.9467285061362247, 87.65113791807857524 ) ) ;
#9832 = CARTESIAN_POINT ( 'NONE',  ( -64.50000000000000000, 155.0000000000000000, 6.938893903907228378E-15 ) ) ;
#9833 = CARTESIAN_POINT ( 'NONE',  ( 3.135527875058820690, 216.4958274776887492, 7.401137918078566358 ) ) ;
#9834 = EDGE_CURVE ( 'NONE', #1337, #29281, #13277, .T. ) ;
#9835 = CARTESIAN_POINT ( 'NONE',  ( 9.984503880673420539, 210.2968891136705167, 72.84886208192143897 ) ) ;
#9836 = CARTESIAN_POINT ( 'NONE',  ( 4.764707147349631625E-14, -103.0000000000000284, 30.00000000000000000 ) ) ;
#9837 = EDGE_LOOP ( 'NONE', ( #13347, #23624, #16572, #4687 ) ) ;
#9838 = CARTESIAN_POINT ( 'NONE',  ( -9.736236675708031640, 214.0148392665760753, 74.79886208192142760 ) ) ;
#9839 = ORIENTED_EDGE ( 'NONE', *, *, #6430, .F. ) ;
#9840 = CARTESIAN_POINT ( 'NONE',  ( 79.47499999726881015, 160.0630714827496206, -15.58253175000000823 ) ) ;
#9841 = CARTESIAN_POINT ( 'NONE',  ( 6.500168698208244500, 202.3363017425938324, 52.29886208192144892 ) ) ;
#9842 = ORIENTED_EDGE ( 'NONE', *, *, #18474, .T. ) ;
#9843 = CARTESIAN_POINT ( 'NONE',  ( 72.22499999726881015, 149.9369285172503510, 15.58253174999999580 ) ) ;
#9844 = FACE_BOUND ( 'NONE', #20821, .T. ) ;
#9845 = CARTESIAN_POINT ( 'NONE',  ( 115.4999999999999858, 246.7986928011511907, 52.99999999999882760 ) ) ;
#9846 = CARTESIAN_POINT ( 'NONE',  ( 64.62499999726881583, 138.6155565068815463, -3.929120461958505118E-15 ) ) ;
#9847 = DIRECTION ( 'NONE',  ( -1.000000000000000000, 0.000000000000000000, 0.000000000000000000 ) ) ;
#9848 = CARTESIAN_POINT ( 'NONE',  ( 0.05014649552828275708, 196.4853777576173002, 40.74886208192143044 ) ) ;
#9849 = ORIENTED_EDGE ( 'NONE', *, *, #32645, .F. ) ;
#9850 = CARTESIAN_POINT ( 'NONE',  ( 34.49999999999997868, 7.979727989493303168E-15, 30.00000000000000000 ) ) ;
#9851 = PRESENTATION_STYLE_ASSIGNMENT (( #25517 ) ) ;
#9852 = CARTESIAN_POINT ( 'NONE',  ( 91.60208470531341618, 155.0000000000000000, -12.00000000000001066 ) ) ;
#9853 = DIRECTION ( 'NONE',  ( 1.000000000000000000, 0.000000000000000000, 0.000000000000000000 ) ) ;
#9854 = CARTESIAN_POINT ( 'NONE',  ( 0.05014649552828262524, 198.5883022060938572, 22.74886208192143755 ) ) ;
#9855 = CARTESIAN_POINT ( 'NONE',  ( 10.00000000000000711, 206.9523078486586201, 68.00113791807856956 ) ) ;
#9856 = CARTESIAN_POINT ( 'NONE',  ( 45.08867513459482268, 167.7597621252805880, -9.270509831248443078 ) ) ;
#9857 = CARTESIAN_POINT ( 'NONE',  ( -6.139770520408369237, 215.5359834540460042, 45.95113791807857950 ) ) ;
#9858 = CARTESIAN_POINT ( 'NONE',  ( -8.118202686958039038, 201.1607312380087080, 15.20113791807856884 ) ) ;
#9859 = CARTESIAN_POINT ( 'NONE',  ( -2.426778023690262742, 214.6231898156240163, 4.101137918078565647 ) ) ;
#9860 = LINE ( 'NONE', #33533, #12772 ) ;
#9861 = CARTESIAN_POINT ( 'NONE',  ( 39.92499999726881299, 164.1591823560292198, 12.60653300113718167 ) ) ;
#9862 = CARTESIAN_POINT ( 'NONE',  ( 9.736236675707914401, 214.0148392665762458, 28.70113791807857240 ) ) ;
#9863 = CARTESIAN_POINT ( 'NONE',  ( 81.98867513459481415, 146.1832212156128890, 12.13525491562421976 ) ) ;
#9864 = CARTESIAN_POINT ( 'NONE',  ( 10.00000000000000711, 206.9523078486586201, 71.00113791807858377 ) ) ;
#9865 = CARTESIAN_POINT ( 'NONE',  ( 6.139770520408367460, 198.4640165459539389, 53.45113791807856529 ) ) ;
#9866 = LINE ( 'NONE', #30999, #7262 ) ;
#9867 = CARTESIAN_POINT ( 'NONE',  ( 54.18867513459482410, 140.7341522555726669, 4.635254915624211769 ) ) ;
#9868 = CARTESIAN_POINT ( 'NONE',  ( 7.456977232089471386, 196.8216656703012006, 16.44886208192143684 ) ) ;
#9869 = CARTESIAN_POINT ( 'NONE',  ( -9.984503880673420539, 203.7031108863293980, 14.34886208192143542 ) ) ;
#9870 = VECTOR ( 'NONE', #17346, 1000.000000000000114 ) ;
#9871 = CARTESIAN_POINT ( 'NONE',  ( 73.69999999453762030, 142.6655632788954620, -8.961492836873480528 ) ) ;
#9872 = ORIENTED_EDGE ( 'NONE', *, *, #13553, .F. ) ;
#9873 = CARTESIAN_POINT ( 'NONE',  ( -7.375838497908182134, 217.2372850707499765, 54.95113791807855819 ) ) ;
#9874 = CARTESIAN_POINT ( 'NONE',  ( 6.444103211791042618, 202.2591342207267644, 74.30113791807858092 ) ) ;
#9875 = CARTESIAN_POINT ( 'NONE',  ( 10.01549611932659545, 203.7984951890123853, 40.14886208192143613 ) ) ;
#9876 = CARTESIAN_POINT ( 'NONE',  ( 125.0000000000000000, -24.99999999999995737, 35.00000000000000000 ) ) ;
#9877 = ORIENTED_EDGE ( 'NONE', *, *, #16132, .T. ) ;
#9878 = ORIENTED_EDGE ( 'NONE', *, *, #16395, .T. ) ;
#9879 = ORIENTED_EDGE ( 'NONE', *, *, #32900, .T. ) ;
#9880 = EDGE_CURVE ( 'NONE', #31294, #19176, #23174, .T. ) ;
#9881 =( REPRESENTATION_RELATIONSHIP ('NONE','NONE', #25663, #22175 ) REPRESENTATION_RELATIONSHIP_WITH_TRANSFORMATION ( #27065 )SHAPE_REPRESENTATION_RELATIONSHIP( ) );
#9882 = DIRECTION ( 'NONE',  ( 1.000000000000000000, -0.000000000000000000, -0.000000000000000000 ) ) ;
#9883 = CARTESIAN_POINT ( 'NONE',  ( 0.000000000000000000, -3.518949890710769246, 3.686287386450715076E-15 ) ) ;
#9884 = ORIENTED_EDGE ( 'NONE', *, *, #31661, .T. ) ;
#9885 = CARTESIAN_POINT ( 'NONE',  ( -4.984841277089726574, 200.2242689037092305, 30.05113791807857027 ) ) ;
#9886 = CARTESIAN_POINT ( 'NONE',  ( 0.000000000000000000, 0.000000000000000000, -25.03750572909317285 ) ) ;
#9887 = CARTESIAN_POINT ( 'NONE',  ( 6.220909254589681581, 198.5229672870052582, 10.44886208192143506 ) ) ;
#9888 = CARTESIAN_POINT ( 'NONE',  ( 56.67499999726881299, 141.7447067706911810, 9.630534252274376428 ) ) ;
#9889 = VERTEX_POINT ( 'NONE', #2564 ) ;
#9890 = CARTESIAN_POINT ( 'NONE',  ( -8.000000000000008882, 207.0476921513413515, 63.50113791807856956 ) ) ;
#9891 = CARTESIAN_POINT ( 'NONE',  ( 66.71132485994280614, 155.0000000000000000, 15.00000000000001243 ) ) ;
#9892 = VECTOR ( 'NONE', #8882, 1000.000000000000227 ) ;
#9893 = SURFACE_STYLE_USAGE ( .BOTH. , #12 ) ;
#9894 = CARTESIAN_POINT ( 'NONE',  ( 0.000000000000000000, 0.000000000000000000, -0.4621369752184044666 ) ) ;
#9895 = CARTESIAN_POINT ( 'NONE',  ( -3.044812012439970683, 197.4746971517856196, 100.8988620819214361 ) ) ;
#9896 = CARTESIAN_POINT ( 'NONE',  ( 68.07499999726881867, 168.2552932293087906, 9.630534252274372875 ) ) ;
#9897 = CARTESIAN_POINT ( 'NONE',  ( -9.984503880673473830, 210.2968891136704315, 42.65113791807856813 ) ) ;
#9898 = DIRECTION ( 'NONE',  ( 0.000000000000000000, 0.000000000000000000, 1.000000000000000000 ) ) ;
#9899 = CARTESIAN_POINT ( 'NONE',  ( -9.984503880673473830, 210.2968891136704315, 18.65113791807856813 ) ) ;
#9900 = FACE_OUTER_BOUND ( 'NONE', #8178, .T. ) ;
#9901 = PRODUCT_CONTEXT ( 'NONE', #28786, 'mechanical' ) ;
#9902 = AXIS2_PLACEMENT_3D ( 'NONE', #9992, #14924, #30944 ) ;
#9903 = CARTESIAN_POINT ( 'NONE',  ( 87.20000000000000284, 167.3344367211045096, 8.961492836873468093 ) ) ;
#9904 = CARTESIAN_POINT ( 'NONE',  ( -13.75000000000001243, -23.81569860407206107, 0.000000000000000000 ) ) ;
#9905 = CARTESIAN_POINT ( 'NONE',  ( 0.000000000000000000, 0.000000000000000000, 0.000000000000000000 ) ) ;
#9906 = CARTESIAN_POINT ( 'NONE',  ( 9.680171189290831535, 199.9079932115568852, 2.301137918078565825 ) ) ;
#9907 = CARTESIAN_POINT ( 'NONE',  ( 125.5000000000000000, 261.0000000000000000, 0.000000000000000000 ) ) ;
#9908 = CARTESIAN_POINT ( 'NONE',  ( 48.77499999726880731, 140.1801316387863778, 4.815267126137185549 ) ) ;
#9909 = CARTESIAN_POINT ( 'NONE',  ( -10.01549611932653860, 203.7984951890123284, 45.35113791807857808 ) ) ;
#9910 = LINE ( 'NONE', #23366, #24640 ) ;
#9911 = DIRECTION ( 'NONE',  ( 1.000000000000000000, 0.000000000000000000, 0.000000000000000000 ) ) ;
#9912 = DIRECTION ( 'NONE',  ( 0.000000000000000000, 0.000000000000000000, 1.000000000000000000 ) ) ;
#9913 = CARTESIAN_POINT ( 'NONE',  ( 55.89999999453761603, 150.2886644046228639, -14.50000000000000888 ) ) ;
#9914 = ORIENTED_EDGE ( 'NONE', *, *, #9988, .F. ) ;
#9915 = CARTESIAN_POINT ( 'NONE',  ( 11.98450388067348271, 203.0532714938637753, 26.15113791807857169 ) ) ;
#9916 = LINE ( 'NONE', #23373, #11098 ) ;
#9917 = CARTESIAN_POINT ( 'NONE',  ( 10.00000000000000711, 207.0476921513415220, 12.99886208192143400 ) ) ;
#9918 = LINE ( 'NONE', #4801, #23209 ) ;
#9919 = ORIENTED_EDGE ( 'NONE', *, *, #1826, .T. ) ;
#9920 = CARTESIAN_POINT ( 'NONE',  ( 3.135527875058820690, 216.4958274776887492, 7.401137918078566358 ) ) ;
#9921 = CARTESIAN_POINT ( 'NONE',  ( 10.00000000000000711, 206.9523078486586201, 62.00113791807856956 ) ) ;
#9922 = ORIENTED_EDGE ( 'NONE', *, *, #23228, .F. ) ;
#9923 = CARTESIAN_POINT ( 'NONE',  ( 8.000000000000008882, 207.0476921513415220, 18.99886208192143400 ) ) ;
#9924 = EDGE_CURVE ( 'NONE', #25076, #9805, #15331, .T. ) ;
#9925 = DIRECTION ( 'NONE',  ( 1.000000000000000000, 0.000000000000000000, 0.000000000000000000 ) ) ;
#9926 = VERTEX_POINT ( 'NONE', #10730 ) ;
#9927 = AXIS2_PLACEMENT_3D ( 'NONE', #16626, #19190, #3682 ) ;
#9928 = CARTESIAN_POINT ( 'NONE',  ( -4.903702542908602524, 213.8346818373418898, 6.951137918078566180 ) ) ;
#9929 = EDGE_CURVE ( 'NONE', #8601, #4633, #30566, .T. ) ;
#9930 = CIRCLE ( 'NONE', #28438, 2.149999999999985256 ) ;
#9931 = CARTESIAN_POINT ( 'NONE',  ( -0.05014649552828442242, 219.6175466908591716, 93.24886208192143044 ) ) ;
#9932 = CARTESIAN_POINT ( 'NONE',  ( 34.77499999726880731, 140.1801316387863778, 4.815267126137185549 ) ) ;
#9933 = ORIENTED_EDGE ( 'NONE', *, *, #26173, .F. ) ;
#9934 = CARTESIAN_POINT ( 'NONE',  ( 43.32499999726881157, 164.1591823560292198, -12.60653300113719766 ) ) ;
#9935 = CARTESIAN_POINT ( 'NONE',  ( 130.1133565525086908, 1.374176392886252485, 35.00001199999999812 ) ) ;
#9936 = EDGE_CURVE ( 'NONE', #22150, #8400, #18232, .T. ) ;
#9937 = LINE ( 'NONE', #7042, #31750 ) ;
#9938 = CARTESIAN_POINT ( 'NONE',  ( 3.044812012439969795, 216.5253028482143520, 69.39886208192143613 ) ) ;
#9939 = CARTESIAN_POINT ( 'NONE',  ( 48.17499999726881299, 164.1591823560292198, 12.60653300113718167 ) ) ;
#9940 = DIRECTION ( 'NONE',  ( 0.000000000000000000, 0.000000000000000000, -1.000000000000000000 ) ) ;
#9941 = CARTESIAN_POINT ( 'NONE',  ( 6.139770520408368348, 198.4640165459539674, -0.5488620819214343749 ) ) ;
#9942 = CARTESIAN_POINT ( 'NONE',  ( 58.21132485994281325, 170.7719333635740497, -7.904646289410545231E-15 ) ) ;
#9943 = CARTESIAN_POINT ( 'NONE',  ( 68.59999999999996589, 159.7113355953771077, -14.50000000000000888 ) ) ;
#9944 = CARTESIAN_POINT ( 'NONE',  ( 6.139770520408368348, 198.4640165459539674, 92.45113791807857240 ) ) ;
#9945 = CARTESIAN_POINT ( 'NONE',  ( -58.50000000000002132, 185.0000000000000000, -2.500000000000000000 ) ) ;
#9946 = CARTESIAN_POINT ( 'NONE',  ( -3.135527875058821579, 197.5041725223112223, 71.90113791807857524 ) ) ;
#9947 = CARTESIAN_POINT ( 'NONE',  ( 27.50000000000000355, -15.87713240271473580, -18.00000000000000000 ) ) ;
#9948 = CARTESIAN_POINT ( 'NONE',  ( 34.67499999726880588, 141.7447067706911810, 9.630534252274376428 ) ) ;
#9949 = CARTESIAN_POINT ( 'NONE',  ( -7.375838497908014268, 196.7627149292498530, 89.04886208192142760 ) ) ;
#9950 = CARTESIAN_POINT ( 'NONE',  ( 62.72499999726881015, 140.1801316387863778, -4.815267126137194431 ) ) ;
#9952 = ORIENTED_EDGE ( 'NONE', *, *, #827, .T. ) ;
#9951 = CARTESIAN_POINT ( 'NONE',  ( 10.01549611932653860, 210.2015048109876716, 34.85113791807857098 ) ) ;
#9953 = CARTESIAN_POINT ( 'NONE',  ( 115.4999999999999858, 182.4348187808683690, 102.3881375866409513 ) ) ;
#9954 = AXIS2_PLACEMENT_3D ( 'NONE', #14550, #11996, #20002 ) ;
#9955 = CARTESIAN_POINT ( 'NONE',  ( 87.47499999726883857, 160.0630714827496206, -15.58253175000000823 ) ) ;
#9956 = CARTESIAN_POINT ( 'NONE',  ( -0.05014649552807705357, 194.3824533091408000, 98.75113791807856956 ) ) ;
#9957 = ADVANCED_FACE ( 'NONE', ( #20950 ), #15167, .F. ) ;
#9958 = CIRCLE ( 'NONE', #16446, 98.00000000000000000 ) ;
#9959 = DIRECTION ( 'NONE',  ( 0.000000000000000000, 0.000000000000000000, -1.000000000000000000 ) ) ;
#9960 = ORIENTED_EDGE ( 'NONE', *, *, #28282, .F. ) ;
#9961 = CARTESIAN_POINT ( 'NONE',  ( -6.139770520408224463, 198.4640165459539105, 83.04886208192144181 ) ) ;
#9962 = CARTESIAN_POINT ( 'NONE',  ( -9.680171189290716072, 199.9079932115567146, 23.19886208192143684 ) ) ;
#9963 = DIRECTION ( 'NONE',  ( 0.000000000000000000, 0.000000000000000000, -1.000000000000000000 ) ) ;
#9964 = CARTESIAN_POINT ( 'NONE',  ( -8.062137200540920645, 212.9164362838581894, 33.80113791807857382 ) ) ;
#9965 = ORIENTED_EDGE ( 'NONE', *, *, #20838, .F. ) ;
#9966 = CARTESIAN_POINT ( 'NONE',  ( -9.984503880673420539, 203.7031108863293980, 98.34886208192143897 ) ) ;
#9967 = ADVANCED_FACE ( 'NONE', ( #28791 ), #3665, .F. ) ;
#9968 = AXIS2_PLACEMENT_3D ( 'NONE', #24694, #17361, #27914 ) ;
#9969 = LINE ( 'NONE', #23077, #13753 ) ;
#9970 = VERTEX_POINT ( 'NONE', #5447 ) ;
#9971 = CARTESIAN_POINT ( 'NONE',  ( 70.01132485994281751, 167.7597621252805880, -9.270509831248443078 ) ) ;
#9972 = CARTESIAN_POINT ( 'NONE',  ( 8.015496119326595448, 204.4483345814782638, 79.14886208192143613 ) ) ;
#9973 = ORIENTED_EDGE ( 'NONE', *, *, #7727, .F. ) ;
#9974 = LINE ( 'NONE', #4857, #31993 ) ;
#9975 = ORIENTED_EDGE ( 'NONE', *, *, #36, .T. ) ;
#9976 = CARTESIAN_POINT ( 'NONE',  ( 8.000000000000000000, 0.000000000000000000, 0.000000000000000000 ) ) ;
#9977 = AXIS2_PLACEMENT_3D ( 'NONE', #28165, #15881, #10946 ) ;
#9978 = CIRCLE ( 'NONE', #29012, 1.000000000000000888 ) ;
#9979 = AXIS2_PLACEMENT_3D ( 'NONE', #16779, #8948, #24453 ) ;
#9980 = CARTESIAN_POINT ( 'NONE',  ( 82.22499999726882436, 149.9369285172503510, 15.58253174999999580 ) ) ;
#9981 = DIRECTION ( 'NONE',  ( -1.000000000000000000, 0.000000000000000000, 0.000000000000000000 ) ) ;
#9982 = CARTESIAN_POINT ( 'NONE',  ( 8.000000000000008882, 206.9523078486586485, 77.00113791807858377 ) ) ;
#9983 = EDGE_CURVE ( 'NONE', #14862, #11826, #12944, .T. ) ;
#9984 = DIRECTION ( 'NONE',  ( 0.000000000000000000, 0.000000000000000000, -1.000000000000000000 ) ) ;
#9985 = AXIS2_PLACEMENT_3D ( 'NONE', #30374, #14691, #22702 ) ;
#9986 = CARTESIAN_POINT ( 'NONE',  ( 43.70000000000000284, 146.4771138417591203, 11.73074641843673227 ) ) ;
#9987 = CARTESIAN_POINT ( 'NONE',  ( -7.984503880673422316, 204.3529502787951628, 65.34886208192142476 ) ) ;
#9988 = EDGE_CURVE ( 'NONE', #31987, #11107, #24333, .T. ) ;
#9989 = VECTOR ( 'NONE', #22301, 1000.000000000000000 ) ;
#9990 = CARTESIAN_POINT ( 'NONE',  ( -3.044812012440131443, 216.5253028482142952, 4.101137918078565647 ) ) ;
#9991 = CARTESIAN_POINT ( 'NONE',  ( 0.000000000000000000, 0.000000000000000000, -9.449444346342714240 ) ) ;
#9992 = CARTESIAN_POINT ( 'NONE',  ( 0.000000000000000000, 0.000000000000000000, 0.000000000000000000 ) ) ;
#9993 = CARTESIAN_POINT ( 'NONE',  ( 54.72499999726881015, 140.1801316387863778, -4.815267126137194431 ) ) ;
#9994 = CARTESIAN_POINT ( 'NONE',  ( 72.07499999726880446, 168.2552932293087906, 9.630534252274372875 ) ) ;
#9995 = COLOUR_RGB ( '', 0.66274510, 0.83137255, 0.94901961) ;
#9996 = CARTESIAN_POINT ( 'NONE',  ( 9.680171189290831535, 199.9079932115568852, 71.30113791807856671 ) ) ;
#9997 = DIRECTION ( 'NONE',  ( 1.000000000000000000, 0.000000000000000000, 0.000000000000000000 ) ) ;
#9998 = ADVANCED_FACE ( 'NONE', ( #12952 ), #26222, .T. ) ;
#9999 = PRODUCT_DEFINITION_SHAPE ( 'NONE', 'NONE',  #33139 ) ;
#10000 = CARTESIAN_POINT ( 'NONE',  ( 0.05014649552807549926, 219.6175466908591716, 7.251137918078565114 ) ) ;
#10001 = CARTESIAN_POINT ( 'NONE',  ( -0.05014649552810635652, 196.4853777576173002, 83.75113791807856956 ) ) ;
#10002 = CARTESIAN_POINT ( 'NONE',  ( -9.680171189290716072, 199.9079932115567146, 41.19886208192144039 ) ) ;
#10003 = CARTESIAN_POINT ( 'NONE',  ( 10.00000000000000711, 207.0476921513415220, 60.99886208192143755 ) ) ;
#10004 = PLANE ( 'NONE',  #33519 ) ;
#10005 = CONICAL_SURFACE ( 'NONE', #29034, 37.00000000000000711, 0.7853981633974482790 ) ;
#10006 = CARTESIAN_POINT ( 'NONE',  ( -9.680171189290831535, 214.0920067884431148, 96.80113791807858092 ) ) ;
#10007 = CARTESIAN_POINT ( 'NONE',  ( 0.1999999999999987899, 4.286263797015736595E-16, -3.500000000000000000 ) ) ;
#10008 = CARTESIAN_POINT ( 'NONE',  ( 3.135527875058820690, 216.4958274776887492, 1.401137918078565914 ) ) ;
#10009 = AXIS2_PLACEMENT_3D ( 'NONE', #8049, #12813, #28984 ) ;
#10010 = CARTESIAN_POINT ( 'NONE',  ( 0.05014649552828275708, 196.4853777576173002, 73.74886208192144466 ) ) ;
#10011 = CIRCLE ( 'NONE', #8374, 2.149999999999974598 ) ;
#10012 = FACE_OUTER_BOUND ( 'NONE', #7039, .T. ) ;
#10013 = ORIENTED_EDGE ( 'NONE', *, *, #28764, .F. ) ;
#10014 = CARTESIAN_POINT ( 'NONE',  ( -3.662846001189865142, 195.5725841191952838, 67.89886208192143613 ) ) ;
#10015 = CARTESIAN_POINT ( 'NONE',  ( 3.135527875058820690, 216.4958274776887492, 91.40113791807857524 ) ) ;
#10016 = ORIENTED_EDGE ( 'NONE', *, *, #21184, .F. ) ;
#10017 = CARTESIAN_POINT ( 'NONE',  ( 76.87499999726881583, 138.6155565068815463, -3.929120461958505118E-15 ) ) ;
#10018 = CARTESIAN_POINT ( 'NONE',  ( -0.05014649552828365914, 215.4116977939061144, 51.24886208192144466 ) ) ;
#10019 = ORIENTED_EDGE ( 'NONE', *, *, #9111, .F. ) ;
#10020 =( BOUNDED_CURVE ( )  B_SPLINE_CURVE ( 2, ( #8038, #5471, #3404, #856, #15857, #18913, #357, #18589, #16183, #26250, #8520 ),
 .UNSPECIFIED., .F., .T. ) 
 B_SPLINE_CURVE_WITH_KNOTS ( ( 3, 2, 2, 2, 2, 3 ),
 ( 0.7678571428571427937, 0.7714285714285713524, 0.7749999999999999112, 0.7785714285714285809, 0.7821428571428571397, 0.7857142857142856984 ),
 .UNSPECIFIED. ) 
 CURVE ( )  GEOMETRIC_REPRESENTATION_ITEM ( )  RATIONAL_B_SPLINE_CURVE ( ( 1.000000000000001554, 0.9510565162951518658, 1.000000000000000000, 0.9510565162951534202, 1.000000000000000000, 0.9510565162951534202, 1.000000000000000000, 0.9510565162951534202, 1.000000000000000000, 0.9510565162951534202, 1.000000000000000000 ) ) 
 REPRESENTATION_ITEM ( '' )  );
#10021 = CARTESIAN_POINT ( 'NONE',  ( 70.52499999726880731, 140.1801316387863778, 4.815267126137185549 ) ) ;
#10022 = FACE_BOUND ( 'NONE', #30836, .T. ) ;
#10023 = CIRCLE ( 'NONE', #25229, 97.99999999999997158 ) ;
#10024 = CYLINDRICAL_SURFACE ( 'NONE', #9437, 32.00000000000002842 ) ;
#10025 = CARTESIAN_POINT ( 'NONE',  ( 65.92499999726881299, 164.1591823560292198, 12.60653300113718167 ) ) ;
#10026 = ADVANCED_FACE ( 'NONE', ( #18060, #5114 ), #15668, .T. ) ;
#10027 = EDGE_CURVE ( 'NONE', #17374, #2210, #10572, .T. ) ;
#10028 = CARTESIAN_POINT ( 'NONE',  ( 0.05014649552828275708, 196.4853777576173002, 49.74886208192141623 ) ) ;
#10029 = ORIENTED_EDGE ( 'NONE', *, *, #10643, .T. ) ;
#10030 = FACE_OUTER_BOUND ( 'NONE', #4888, .T. ) ;
#10031 = AXIS2_PLACEMENT_3D ( 'NONE', #25736, #26233, #15177 ) ;
#10032 = CARTESIAN_POINT ( 'NONE',  ( 0.9108756637647450471, -6.979659189788935514, -6.219623095965384429 ) ) ;
#10033 = CARTESIAN_POINT ( 'NONE',  ( 127.5000000000000000, 261.0000000000000000, -2.149999999999985256 ) ) ;
#10034 = CARTESIAN_POINT ( 'NONE',  ( 2.517493886309087436, 199.4062855549015865, 22.59886208192143542 ) ) ;
#10035 = AXIS2_PLACEMENT_3D ( 'NONE', #24711, #3248, #21307 ) ;
#10036 = CARTESIAN_POINT ( 'NONE',  ( 6.139770520408368348, 198.4640165459539674, 71.45113791807857240 ) ) ;
#10037 = CARTESIAN_POINT ( 'NONE',  ( -52.50000000000002132, -95.00000000000000000, -20.00000000000000000 ) ) ;
#10038 = ADVANCED_FACE ( 'NONE', ( #12607 ), #10763, .T. ) ;
#10039 = CARTESIAN_POINT ( 'NONE',  ( 8.062137200540920645, 201.0835637161417822, 59.30113791807857382 ) ) ;
#10040 = ITEM_DEFINED_TRANSFORMATION ( 'NONE', 'NONE', #2859,  #2404 ) ;
#10041 = CARTESIAN_POINT ( 'NONE',  ( -8.062137200540920645, 212.9164362838581894, 30.80113791807856671 ) ) ;
#10042 = CARTESIAN_POINT ( 'NONE',  ( -6.444103211791042618, 211.7408657792732356, 0.8011379180785661580 ) ) ;
#10043 = CARTESIAN_POINT ( 'NONE',  ( -64.50000000000000000, -2.605762844159085212, 20.00000000000000000 ) ) ;
#10044 = CARTESIAN_POINT ( 'NONE',  ( 40.82499999726880446, 141.7447067706911810, -9.630534252274387086 ) ) ;
#10045 = ADVANCED_BREP_SHAPE_REPRESENTATION ( '', ( #619, #2404 ), #29608 ) ;
#10046 = CARTESIAN_POINT ( 'NONE',  ( -7.375838497908182134, 217.2372850707499765, 33.95113791807856529 ) ) ;
#10047 = CARTESIAN_POINT ( 'NONE',  ( 117.5000000000000000, 155.0000000000000000, -6.938893903907228378E-15 ) ) ;
#10048 = CARTESIAN_POINT ( 'NONE',  ( 3.135527875058820690, 216.4958274776887492, 82.40113791807857524 ) ) ;
#10049 = CARTESIAN_POINT ( 'NONE',  ( -8.118202686958039038, 201.1607312380087080, 48.20113791807857950 ) ) ;
#10050 = FACE_OUTER_BOUND ( 'NONE', #28933, .T. ) ;
#10051 = CARTESIAN_POINT ( 'NONE',  ( -11.98450388067341876, 203.0532714938636047, 11.34886208192143542 ) ) ;
#10052 = CARTESIAN_POINT ( 'NONE',  ( -6.220909254589682469, 215.4770327129947134, 26.94886208192143329 ) ) ;
#10053 = CARTESIAN_POINT ( 'NONE',  ( 75.39999999453762314, 141.2096805137202580, 4.480746418436733158 ) ) ;
#10054 = ORIENTED_EDGE ( 'NONE', *, *, #29938, .T. ) ;
#10055 = CARTESIAN_POINT ( 'NONE',  ( 11.98450388067348271, 203.0532714938637753, 59.15113791807857524 ) ) ;
#10056 = CARTESIAN_POINT ( 'NONE',  ( 4.984841277089725686, 213.7757310962907411, 82.55113791807858092 ) ) ;
#10057 = CARTESIAN_POINT ( 'NONE',  ( -6.139770520408224463, 198.4640165459539389, 41.04886208192142760 ) ) ;
#10058 = CARTESIAN_POINT ( 'NONE',  ( 75.01132485994280330, 142.2402378747194405, 9.270509831248432420 ) ) ;
#10059 = ORIENTED_EDGE ( 'NONE', *, *, #4099, .F. ) ;
#10060 = CARTESIAN_POINT ( 'NONE',  ( 9.680171189290716072, 214.0920067884432854, 39.69886208192144039 ) ) ;
#10061 = AXIS2_PLACEMENT_3D ( 'NONE', #14745, #14078, #12026 ) ;
#10062 = EDGE_LOOP ( 'NONE', ( #29979, #31502, #3211 ) ) ;
#10063 = ORIENTED_EDGE ( 'NONE', *, *, #1607, .F. ) ;
#10064 = CARTESIAN_POINT ( 'NONE',  ( 32.50000000000000000, 155.0000000000000000, 15.00000000000001243 ) ) ;
#10065 = CARTESIAN_POINT ( 'NONE',  ( 56.78867513459481842, 155.0000000000000000, -15.00000000000002487 ) ) ;
#10066 = ORIENTED_EDGE ( 'NONE', *, *, #16616, .F. ) ;
#10067 = CARTESIAN_POINT ( 'NONE',  ( 0.05014649552807626948, 215.4116977939061144, 31.25113791807856956 ) ) ;
#10068 = FACE_OUTER_BOUND ( 'NONE', #29734, .T. ) ;
#10069 = CARTESIAN_POINT ( 'NONE',  ( -10.01549611932659722, 210.2015048109875011, 17.64886208192143613 ) ) ;
#10070 = CARTESIAN_POINT ( 'NONE',  ( 58.97499999726881015, 140.1801316387863778, -4.815267126137194431 ) ) ;
#10071 = VERTEX_POINT ( 'NONE', #7345 ) ;
#10072 = CARTESIAN_POINT ( 'NONE',  ( 6.444103211791042618, 202.2591342207267644, 56.30113791807857382 ) ) ;
#10073 = CARTESIAN_POINT ( 'NONE',  ( 16.00000000000000000, 1.971681346627238735E-16, -1.610000000000000098 ) ) ;
#10074 = LINE ( 'NONE', #19773, #9171 ) ;
#10075 = CARTESIAN_POINT ( 'NONE',  ( -6.220909254589682469, 215.4770327129946850, 101.9488620819214333 ) ) ;
#10076 = CARTESIAN_POINT ( 'NONE',  ( 64.97499999726881015, 140.1801316387863778, -4.815267126137194431 ) ) ;
#10077 = CARTESIAN_POINT ( 'NONE',  ( 3.135527875058820690, 216.4958274776887492, 37.40113791807857524 ) ) ;
#10078 =( NAMED_UNIT ( * ) SI_UNIT ( $, .STERADIAN. ) SOLID_ANGLE_UNIT ( ) );
#10079 = CARTESIAN_POINT ( 'NONE',  ( 3.044812012440130555, 197.4746971517856764, 26.60113791807856742 ) ) ;
#10080 = DIRECTION ( 'NONE',  ( 0.000000000000000000, -1.000000000000000000, 0.000000000000000000 ) ) ;
#10081 = B_SPLINE_CURVE_WITH_KNOTS ( 'NONE', 3,
 ( #14335, #9387, #9226, #6668 ),
 .UNSPECIFIED., .F., .F.,
 ( 4, 4 ),
 ( 2.380739283024902572E-07, 0.002044882221487580483 ),
 .UNSPECIFIED. ) ;
#10082 = DIRECTION ( 'NONE',  ( 0.9237280213470682178, 0.3830490080632377725, 1.131240564625405124E-16 ) ) ;
#10083 = CARTESIAN_POINT ( 'NONE',  ( 86.40000000000001990, 150.2886644046228639, -14.50000000000000888 ) ) ;
#10084 = CARTESIAN_POINT ( 'NONE',  ( 107.5000000000000000, 155.0000000000000000, -70.00000000000000000 ) ) ;
#10085 = CARTESIAN_POINT ( 'NONE',  ( -58.50000000000002132, 185.0000000000000000, 0.000000000000000000 ) ) ;
#10086 = CARTESIAN_POINT ( 'NONE',  ( -7.375838497908182134, 217.2372850707499765, 0.9511379180785655141 ) ) ;
#10087 = CARTESIAN_POINT ( 'NONE',  ( 64.48867513459482836, 142.2402378747194405, -9.270509831248439525 ) ) ;
#10088 = CARTESIAN_POINT ( 'NONE',  ( 48.67499999726881299, 141.7447067706911810, 9.630534252274376428 ) ) ;
#10089 = CARTESIAN_POINT ( 'NONE',  ( -6.220909254589537696, 198.5229672870051161, 45.05113791807855961 ) ) ;
#10090 = DIRECTION ( 'NONE',  ( 0.000000000000000000, 0.000000000000000000, 1.000000000000000000 ) ) ;
#10091 = CARTESIAN_POINT ( 'NONE',  ( -52.50000000000002132, 155.0000000000000000, 6.938893903907228378E-15 ) ) ;
#10092 = DIRECTION ( 'NONE',  ( 1.000000000000000000, -0.000000000000000000, -0.000000000000000000 ) ) ;
#10093 = CARTESIAN_POINT ( 'NONE',  ( 57.09999999453762598, 150.2886644046228639, 14.49999999999999645 ) ) ;
#10094 = ORIENTED_EDGE ( 'NONE', *, *, #1371, .T. ) ;
#10095 = CARTESIAN_POINT ( 'NONE',  ( -11.98450388067348804, 210.9467285061362247, 24.65113791807857169 ) ) ;
#10096 = DIRECTION ( 'NONE',  ( 1.000000000000000000, 0.000000000000000000, 0.000000000000000000 ) ) ;
#10097 = CARTESIAN_POINT ( 'NONE',  ( -6.220909254589682469, 215.4770327129946850, 8.948862081921435063 ) ) ;
#10098 = CYLINDRICAL_SURFACE ( 'NONE', #7996, 2.149999999999985256 ) ;
#10099 = ORIENTED_EDGE ( 'NONE', *, *, #351, .T. ) ;
#10100 = CARTESIAN_POINT ( 'NONE',  ( 6.139770520408368348, 198.4640165459539674, 11.45113791807856707 ) ) ;
#10101 = CARTESIAN_POINT ( 'NONE',  ( 9.984503880673470277, 203.7031108863295401, 68.15113791807857524 ) ) ;
#10102 = VERTEX_POINT ( 'NONE', #17724 ) ;
#10103 = CARTESIAN_POINT ( 'NONE',  ( -6.500168698208244500, 211.6636982574061676, 23.79886208192143826 ) ) ;
#10104 = CYLINDRICAL_SURFACE ( 'NONE', #25211, 2.149999999999985256 ) ;
#10105 = ORIENTED_EDGE ( 'NONE', *, *, #8509, .F. ) ;
#10106 = CARTESIAN_POINT ( 'NONE',  ( 2.426778023690261410, 199.3768101843759837, -0.3988620819214340751 ) ) ;
#10107 = CARTESIAN_POINT ( 'NONE',  ( -12.00000000000000711, 206.9523078486584780, 92.49886208192144466 ) ) ;
#10108 = CARTESIAN_POINT ( 'NONE',  ( 37.57499999726881157, 164.1591823560292198, -12.60653300113719766 ) ) ;
#10109 = ORIENTED_EDGE ( 'NONE', *, *, #27467, .T. ) ;
#10110 = CARTESIAN_POINT ( 'NONE',  ( 41.82499999726881157, 168.2552932293087906, 9.630534252274372875 ) ) ;
#10111 = CARTESIAN_POINT ( 'NONE',  ( 39.71132485994280614, 155.0000000000000000, -15.00000000000002487 ) ) ;
#10112 = CARTESIAN_POINT ( 'NONE',  ( 6.220909254589536808, 215.4770327129947702, 4.551137918078564937 ) ) ;
#10113 = CARTESIAN_POINT ( 'NONE',  ( -0.05014649552828403384, 217.5146222423826714, 72.24886208192140202 ) ) ;
#10114 = CARTESIAN_POINT ( 'NONE',  ( 46.57499999726881157, 145.8408176439707802, 12.60653300113718345 ) ) ;
#10115 = CARTESIAN_POINT ( 'NONE',  ( -67.50001199999999812, 138.5437169723398938, -4.407803664655109976 ) ) ;
#10116 = CARTESIAN_POINT ( 'NONE',  ( 6.139770520408368348, 198.4640165459539674, 8.451137918078565292 ) ) ;
#10117 = DIRECTION ( 'NONE',  ( 0.000000000000000000, 0.000000000000000000, -1.000000000000000000 ) ) ;
#10118 = CARTESIAN_POINT ( 'NONE',  ( 67.39999999999997726, 159.7113355953771077, 14.49999999999999289 ) ) ;
#10119 = CARTESIAN_POINT ( 'NONE',  ( -8.062137200540920645, 212.9164362838581894, 96.80113791807858092 ) ) ;
#10120 = DIRECTION ( 'NONE',  ( -1.000000000000000000, -0.000000000000000000, 0.000000000000000000 ) ) ;
#10121 = CARTESIAN_POINT ( 'NONE',  ( -9.984503880673473830, 210.2968891136704315, 78.65113791807854682 ) ) ;
#10122 = CARTESIAN_POINT ( 'NONE',  ( -58.50000000000002132, 185.0000000000000000, -2.500000000000000000 ) ) ;
#10123 = CARTESIAN_POINT ( 'NONE',  ( 27.50000000000000711, 5.390523180938862957, -0.2837416352459796176 ) ) ;
#10124 = CARTESIAN_POINT ( 'NONE',  ( 0.05014649552828288198, 194.3824533091408000, 82.74886208192144466 ) ) ;
#10125 = EDGE_CURVE ( 'NONE', #29866, #12770, #25976, .T. ) ;
#10126 = CARTESIAN_POINT ( 'NONE',  ( 72.92499999726881299, 145.8408176439707802, -12.60653300113719588 ) ) ;
#10127 = VERTEX_POINT ( 'NONE', #3378 ) ;
#10128 = CARTESIAN_POINT ( 'NONE',  ( -60.99994150909498103, 194.9999963443187028, 0.1639972282098350886 ) ) ;
#10129 = CARTESIAN_POINT ( 'NONE',  ( 34.19999999453762740, 163.5228861582408797, -11.73074641843674470 ) ) ;
#10130 = CARTESIAN_POINT ( 'NONE',  ( -12.00000000000000711, 207.0476921513413515, 99.50113791807856956 ) ) ;
#10131 = FACE_OUTER_BOUND ( 'NONE', #14524, .T. ) ;
#10132 = ORIENTED_EDGE ( 'NONE', *, *, #6484, .T. ) ;
#10133 = CARTESIAN_POINT ( 'NONE',  ( 10.01549611932659367, 203.7984951890124421, 85.14886208192143613 ) ) ;
#10134 = CARTESIAN_POINT ( 'NONE',  ( -12.00000000000000711, 206.9523078486584780, 26.49886208192143400 ) ) ;
#10135 = DIRECTION ( 'NONE',  ( -1.000000000000000000, 0.000000000000000000, 0.000000000000000000 ) ) ;
#10136 = CARTESIAN_POINT ( 'NONE',  ( -9.984503880673473830, 210.2968891136704315, 42.65113791807856813 ) ) ;
#10137 = VERTEX_POINT ( 'NONE', #29445 ) ;
#10138 = CARTESIAN_POINT ( 'NONE',  ( -8.062137200540822946, 201.0835637161416400, 101.1988620819214475 ) ) ;
#10139 = LINE ( 'NONE', #30924, #3415 ) ;
#10140 = ORIENTED_EDGE ( 'NONE', *, *, #19258, .T. ) ;
#10141 = DIRECTION ( 'NONE',  ( -1.000000000000000000, -0.000000000000000000, -0.000000000000000000 ) ) ;
#10142 = CARTESIAN_POINT ( 'NONE',  ( -0.05014649552828365914, 215.4116977939061144, 81.24886208192143044 ) ) ;
#10143 = VERTEX_POINT ( 'NONE', #14108 ) ;
#10144 = DIRECTION ( 'NONE',  ( 1.000000000000000000, 0.000000000000000000, 0.000000000000000000 ) ) ;
#10145 = EDGE_LOOP ( 'NONE', ( #13224, #13843, #20442, #28499 ) ) ;
#10146 = DIRECTION ( 'NONE',  ( -1.000000000000000000, 0.000000000000000000, 0.000000000000000000 ) ) ;
#10147 = CARTESIAN_POINT ( 'NONE',  ( 4.984841277089725686, 213.7757310962907411, 64.55113791807856671 ) ) ;
#10148 = CARTESIAN_POINT ( 'NONE',  ( 80.82499999726880446, 141.7447067706911810, -9.630534252274385310 ) ) ;
#10149 = DIRECTION ( 'NONE',  ( -0.000000000000000000, 0.8660254037844391517, 0.4999999999999990563 ) ) ;
#10150 = CARTESIAN_POINT ( 'NONE',  ( -0.05014649552807731031, 198.5883022060938572, 83.75113791807856956 ) ) ;
#10151 = DIRECTION ( 'NONE',  ( 0.000000000000000000, 0.4999999999999990008, -0.8660254037844391517 ) ) ;
#10152 = CARTESIAN_POINT ( 'NONE',  ( 47.00000000000000000, 170.2462022514548323, -7.872454543227099337E-15 ) ) ;
#10153 = CARTESIAN_POINT ( 'NONE',  ( -2.517493886309087880, 214.5937144450984135, 60.09886208192145318 ) ) ;
#10154 = CARTESIAN_POINT ( 'NONE',  ( 5.000000000000000000, 3.513898075855361292, 2.028749999999997833 ) ) ;
#10155 = EDGE_CURVE ( 'NONE', #31163, #13926, #416, .T. ) ;
#10156 = AXIS2_PLACEMENT_3D ( 'NONE', #11584, #6642, #29648 ) ;
#10157 = CARTESIAN_POINT ( 'NONE',  ( -10.00000000000000711, 207.0476921513413515, 0.5011379180785656695 ) ) ;
#10158 = FACE_OUTER_BOUND ( 'NONE', #4081, .T. ) ;
#10159 = FACE_OUTER_BOUND ( 'NONE', #3909, .T. ) ;
#10160 = CARTESIAN_POINT ( 'NONE',  ( 54.22499999726881015, 149.9369285172503510, 15.58253174999999580 ) ) ;
#10161 = CARTESIAN_POINT ( 'NONE',  ( 68.57499999726881867, 145.8408176439707802, 12.60653300113718345 ) ) ;
#10162 = CARTESIAN_POINT ( 'NONE',  ( -9.680171189290831535, 214.0920067884431148, 63.80113791807858092 ) ) ;
#10163 = DIRECTION ( 'NONE',  ( -0.000000000000000000, -0.000000000000000000, -1.000000000000000000 ) ) ;
#10164 = CARTESIAN_POINT ( 'NONE',  ( -12.01549611932652972, 203.1486557965464499, 6.351137918078565647 ) ) ;
#10165 = B_SPLINE_CURVE_WITH_KNOTS ( 'NONE', 3,
 ( #26134, #13511, #5677, #3795, #26621, #29356 ),
 .UNSPECIFIED., .F., .F.,
 ( 4, 2, 4 ),
 ( 0.000000000000000000, 0.002307655110370376069, 0.004615310220740751271 ),
 .UNSPECIFIED. ) ;
#10166 = CARTESIAN_POINT ( 'NONE',  ( -3.135527875058821579, 197.5041725223112223, 83.90113791807857524 ) ) ;
#10167 = CONICAL_SURFACE ( 'NONE', #1448, 5.000000000000001776, 0.9599310885968795892 ) ;
#10168 = EDGE_CURVE ( 'NONE', #21673, #30739, #5763, .T. ) ;
#10169 = CARTESIAN_POINT ( 'NONE',  ( 9.736236675708031640, 199.9851607334238963, 55.29886208192143471 ) ) ;
#10170 = CARTESIAN_POINT ( 'NONE',  ( -8.118202686958138514, 212.8392687619910930, 59.79886208192143471 ) ) ;
#10171 = FACE_OUTER_BOUND ( 'NONE', #30702, .T. ) ;
#10172 = CARTESIAN_POINT ( 'NONE',  ( 11.98450388067348271, 203.0532714938637753, 98.15113791807856103 ) ) ;
#10173 = CARTESIAN_POINT ( 'NONE',  ( -67.50001199999999812, 169.7531371834000993, 8.519561460567040001 ) ) ;
#10174 = CARTESIAN_POINT ( 'NONE',  ( 3.044812012440130555, 197.4746971517856764, 2.601137918078566091 ) ) ;
#10175 = CARTESIAN_POINT ( 'NONE',  ( -6.139770520408224463, 198.4640165459539389, 71.04886208192139918 ) ) ;
#10176 = CARTESIAN_POINT ( 'NONE',  ( 27.50000000000000355, 15.87713240271474291, -15.54379906938135214 ) ) ;
#10177 = ORIENTED_EDGE ( 'NONE', *, *, #24157, .T. ) ;
#10178 = CARTESIAN_POINT ( 'NONE',  ( 9.736236675708031640, 199.9851607334238963, 82.29886208192144181 ) ) ;
#10179 = CARTESIAN_POINT ( 'NONE',  ( -6.220909254589537696, 198.5229672870051161, 93.05113791807853829 ) ) ;
#10180 = VERTEX_POINT ( 'NONE', #21603 ) ;
#10181 = CARTESIAN_POINT ( 'NONE',  ( 78.87499999726878741, 138.6155565068815463, -3.929120461958505118E-15 ) ) ;
#10182 = CARTESIAN_POINT ( 'NONE',  ( 6.500168698208244500, 202.3363017425938324, 49.29886208192144892 ) ) ;
#10183 = EDGE_LOOP ( 'NONE', ( #23247, #11254, #20346, #5861 ) ) ;
#10184 = EDGE_CURVE ( 'NONE', #12765, #11884, #2711, .T. ) ;
#10185 = VECTOR ( 'NONE', #28774, 1000.000000000000000 ) ;
#10186 = CARTESIAN_POINT ( 'NONE',  ( 73.52499999726882152, 169.8198683612136222, -4.815267126137197984 ) ) ;
#10187 = CARTESIAN_POINT ( 'NONE',  ( 6.500000000000296652, 3.350125858420170299, -6.343571411523281967 ) ) ;
#10188 = AXIS2_PLACEMENT_3D ( 'NONE', #9886, #17205, #22656 ) ;
#10189 = CARTESIAN_POINT ( 'NONE',  ( -7.500000000000000000, -4.330127018922199866, -1.000000000000000888 ) ) ;
#10190 = ADVANCED_FACE ( 'NONE', ( #11396 ), #24328, .T. ) ;
#10191 = CARTESIAN_POINT ( 'NONE',  ( 66.72499999726881015, 140.1801316387863778, -4.815267126137194431 ) ) ;
#10192 = DIRECTION ( 'NONE',  ( -1.000000000000000000, 0.000000000000000000, 0.000000000000000000 ) ) ;
#10193 = CARTESIAN_POINT ( 'NONE',  ( 6.220909254589681581, 198.5229672870052582, 49.44886208192144039 ) ) ;
#10194 = ORIENTED_EDGE ( 'NONE', *, *, #16046, .T. ) ;
#10195 = VECTOR ( 'NONE', #20365, 1000.000000000000000 ) ;
#10196 = CARTESIAN_POINT ( 'NONE',  ( 16.66875746037182537, 22.13055319862716175, -17.88577775926227531 ) ) ;
#10197 = PRESENTATION_STYLE_ASSIGNMENT (( #30804 ) ) ;
#10198 = DIRECTION ( 'NONE',  ( 0.8191520442889912434, 0.000000000000000000, 0.5735764363510469366 ) ) ;
#10199 = CARTESIAN_POINT ( 'NONE',  ( -6.500168698208244500, 211.6636982574061676, 35.79886208192144181 ) ) ;
#10200 = CARTESIAN_POINT ( 'NONE',  ( -3.044812012440131443, 216.5253028482142952, 73.10113791807857808 ) ) ;
#10201 = CYLINDRICAL_SURFACE ( 'NONE', #14210, 2.149999999999985256 ) ;
#10202 = CARTESIAN_POINT ( 'NONE',  ( 3.044812012440130555, 197.4746971517856764, 56.60113791807857098 ) ) ;
#10203 = CARTESIAN_POINT ( 'NONE',  ( -9.984503880673473830, 210.2968891136704315, 27.65113791807855748 ) ) ;
#10204 = CARTESIAN_POINT ( 'NONE',  ( -8.015496119326531499, 204.4483345814780364, 18.35113791807856387 ) ) ;
#10205 = CARTESIAN_POINT ( 'NONE',  ( 86.87499999726880162, 138.6155565068815747, -3.929120461958505118E-15 ) ) ;
#10206 = CARTESIAN_POINT ( 'NONE',  ( -65.20000000000000284, -0.9203920079924774456, 19.30000000000001847 ) ) ;
#10207 = CARTESIAN_POINT ( 'NONE',  ( 41.22499999726881015, 160.0630714827496206, -15.58253175000000823 ) ) ;
#10208 = CARTESIAN_POINT ( 'NONE',  ( -11.98450388067348804, 210.9467285061362247, 42.65113791807856813 ) ) ;
#10209 = CARTESIAN_POINT ( 'NONE',  ( -125.0000000000000000, 25.00000000000000000, -35.00000000000000000 ) ) ;
#10210 = AXIS2_PLACEMENT_3D ( 'NONE', #1376, #22152, #1707 ) ;
#10211 = CARTESIAN_POINT ( 'NONE',  ( 0.05014649552810505201, 217.5146222423826714, 88.25113791807858377 ) ) ;
#10212 = CARTESIAN_POINT ( 'NONE',  ( -6.220909254589537696, 198.5229672870051445, 63.05113791807858092 ) ) ;
#10213 = AXIS2_PLACEMENT_3D ( 'NONE', #4377, #17663, #1993 ) ;
#10214 = CARTESIAN_POINT ( 'NONE',  ( 125.5000000000000000, 157.1500000000010573, 105.9999999999999858 ) ) ;
#10215 = CARTESIAN_POINT ( 'NONE',  ( 7.456977232089471386, 196.8216656703012006, 19.44886208192143329 ) ) ;
#10216 = VECTOR ( 'NONE', #22722, 1000.000000000000114 ) ;
#10217 = CARTESIAN_POINT ( 'NONE',  ( 9.984503880673420539, 210.2968891136705736, 30.84886208192143187 ) ) ;
#10218 = CARTESIAN_POINT ( 'NONE',  ( 70.29999999453762882, 167.3344367211045096, -8.961492836873482304 ) ) ;
#10219 = ORIENTED_EDGE ( 'NONE', *, *, #29945, .T. ) ;
#10220 = CARTESIAN_POINT ( 'NONE',  ( -7.456977232089304408, 196.8216656703010301, 72.05113791807858092 ) ) ;
#10221 = CARTESIAN_POINT ( 'NONE',  ( 2.426778023690261410, 199.3768101843759837, 74.60113791807854966 ) ) ;
#10222 = ADVANCED_FACE ( 'NONE', ( #662 ), #13435, .F. ) ;
#10223 = CARTESIAN_POINT ( 'NONE',  ( 6.139770520408223575, 215.5359834540460611, 42.54886208192142050 ) ) ;
#10224 = EDGE_CURVE ( 'NONE', #15702, #4983, #8369, .T. ) ;
#10225 = DIRECTION ( 'NONE',  ( -1.000000000000000000, 0.000000000000000000, 0.000000000000000000 ) ) ;
#10226 = VECTOR ( 'NONE', #18617, 1000.000000000000000 ) ;
#10227 = VERTEX_POINT ( 'NONE', #31512 ) ;
#10228 = CARTESIAN_POINT ( 'NONE',  ( -7.456977232089471386, 217.1783343296987709, 47.94886208192143329 ) ) ;
#10229 = ORIENTED_EDGE ( 'NONE', *, *, #25342, .T. ) ;
#10230 = ORIENTED_EDGE ( 'NONE', *, *, #14579, .F. ) ;
#10231 = EDGE_CURVE ( 'NONE', #3461, #18094, #6164, .T. ) ;
#10232 = DIRECTION ( 'NONE',  ( -0.000000000000000000, -0.000000000000000000, 1.000000000000000000 ) ) ;
#10233 = CARTESIAN_POINT ( 'NONE',  ( 56.08867513459481557, 142.2402378747194405, 9.270509831248432420 ) ) ;
#10234 = ORIENTED_EDGE ( 'NONE', *, *, #28764, .T. ) ;
#10235 = CARTESIAN_POINT ( 'NONE',  ( -4.903702542908602524, 213.8346818373418898, 39.95113791807856529 ) ) ;
#10236 = AXIS2_PLACEMENT_3D ( 'NONE', #7302, #18357, #28247 ) ;
#10237 = EDGE_CURVE ( 'NONE', #32735, #5752, #26890, .T. ) ;
#10239 =( LENGTH_UNIT ( ) NAMED_UNIT ( * ) SI_UNIT ( .MILLI., .METRE. ) );
#10238 = B_SPLINE_CURVE_WITH_KNOTS ( 'NONE', 3,
 ( #33166, #1812, #15096, #4707, #30611, #28393, #17321, #9830, #27869, #12208 ),
 .UNSPECIFIED., .F., .F.,
 ( 4, 2, 2, 2, 4 ),
 ( 0.009353627468483380336, 0.01031000219096067302, 0.01126637691343796571, 0.01222275163591525840, 0.01317912635839255109 ),
 .UNSPECIFIED. ) ;
#10240 = CONICAL_SURFACE ( 'NONE', #22180, 37.00000000000000711, 0.7853981633974482790 ) ;
#10241 = CARTESIAN_POINT ( 'NONE',  ( 8.118202686958138514, 201.1607312380088501, 19.29886208192143471 ) ) ;
#10242 = CARTESIAN_POINT ( 'NONE',  ( 65.17499999726881299, 145.8408176439707802, -12.60653300113719588 ) ) ;
#10243 = ORIENTED_EDGE ( 'NONE', *, *, #17718, .T. ) ;
#10244 = CARTESIAN_POINT ( 'NONE',  ( 6.293430271071537518, -5.026740376715104652, -0.4524126574264552558 ) ) ;
#10245 = PRESENTATION_LAYER_ASSIGNMENT (  '', '', ( #21089 ) ) ;
#10246 =( NAMED_UNIT ( * ) PLANE_ANGLE_UNIT ( ) SI_UNIT ( $, .RADIAN. ) );
#10247 = DIRECTION ( 'NONE',  ( 0.000000000000000000, 0.000000000000000000, -1.000000000000000000 ) ) ;
#10248 = CARTESIAN_POINT ( 'NONE',  ( -4.903702542908436435, 200.1653181626580249, 2.048862081921434708 ) ) ;
#10249 = CARTESIAN_POINT ( 'NONE',  ( -10.01549611932653860, 203.7984951890123284, 39.35113791807857098 ) ) ;
#10250 = CARTESIAN_POINT ( 'NONE',  ( 87.21132485994283456, 139.2280666364260071, -4.041636747397287284E-15 ) ) ;
#10251 = CARTESIAN_POINT ( 'NONE',  ( 8.062137200540920645, 201.0835637161417822, 26.30113791807856671 ) ) ;
#10252 = CARTESIAN_POINT ( 'NONE',  ( -6.220909254589682469, 215.4770327129947134, 101.9488620819214617 ) ) ;
#10253 = SHAPE_DEFINITION_REPRESENTATION ( #28218, #17198 ) ;
#10254 = CARTESIAN_POINT ( 'NONE',  ( 4.984841277089891776, 200.2242689037093726, 85.44886208192144750 ) ) ;
#10255 = CARTESIAN_POINT ( 'NONE',  ( 83.90000000000000568, 141.2096805137202580, 4.480746418436733158 ) ) ;
#10256 = CARTESIAN_POINT ( 'NONE',  ( -65.50384660342780307, 120.9385549553365848, -18.99615339657220758 ) ) ;
#10257 = CARTESIAN_POINT ( 'NONE',  ( -16.09259079475562615, 22.46320317811876421, -18.00000000000000711 ) ) ;
#10258 = CARTESIAN_POINT ( 'NONE',  ( -0.05014649552807705357, 194.3824533091408000, 8.751137918078567779 ) ) ;
#10259 = CARTESIAN_POINT ( 'NONE',  ( 64.28867513459482552, 139.2280666364260071, -4.041636747397287284E-15 ) ) ;
#10260 = CARTESIAN_POINT ( 'NONE',  ( 52.97499999726881015, 140.1801316387863778, -4.815267126137194431 ) ) ;
#10261 = CARTESIAN_POINT ( 'NONE',  ( 8.062137200540920645, 201.0835637161417822, 56.30113791807857382 ) ) ;
#10262 = ADVANCED_FACE ( 'NONE', ( #24838, #9331 ), #24674, .F. ) ;
#10263 = CARTESIAN_POINT ( 'NONE',  ( 87.52499999726882152, 169.8198683612136222, -4.815267126137197984 ) ) ;
#10264 = CARTESIAN_POINT ( 'NONE',  ( 78.31132485994280046, 169.2658477444273331, 4.635254915624208216 ) ) ;
#10265 = CARTESIAN_POINT ( 'NONE',  ( 65.41132485994282320, 142.2402378747194405, -9.270509831248439525 ) ) ;
#10266 = CARTESIAN_POINT ( 'NONE',  ( 56.39999999453762314, 168.7903194862797420, -4.480746418436745593 ) ) ;
#10267 = VERTEX_POINT ( 'NONE', #27893 ) ;
#10268 =( BOUNDED_CURVE ( )  B_SPLINE_CURVE ( 2, ( #14124, #9013, #19402, #26405, #8354, #18742, #29128, #25184, #9863, #22298, #4068 ),
 .UNSPECIFIED., .F., .F. ) 
 B_SPLINE_CURVE_WITH_KNOTS ( ( 3, 2, 2, 2, 2, 3 ),
 ( 0.08928571428571410729, 0.09285714285714277705, 0.09642857142857132191, 0.09999999999999988065, 0.1035714285714284255, 0.1071428571428569843 ),
 .UNSPECIFIED. ) 
 CURVE ( )  GEOMETRIC_REPRESENTATION_ITEM ( )  RATIONAL_B_SPLINE_CURVE ( ( 1.000000000000001110, 0.9510565162951523099, 1.000000000000000000, 0.9510565162951534202, 1.000000000000000000, 0.9510565162951534202, 1.000000000000000000, 0.9510565162951534202, 1.000000000000000000, 0.9510565162951549745, 0.9999999999999984457 ) ) 
 REPRESENTATION_ITEM ( '' )  );
#10269 = CARTESIAN_POINT ( 'NONE',  ( 9.680171189290831535, 199.9079932115568852, 41.30113791807857382 ) ) ;
#10270 = CIRCLE ( 'NONE', #32528, 5.250000000000004441 ) ;
#10271 = CARTESIAN_POINT ( 'NONE',  ( 46.81132485994280756, 150.1262045565063659, 14.99999999999997158 ) ) ;
#10272 = CARTESIAN_POINT ( 'NONE',  ( -6.220909254589682469, 215.4770327129946850, 14.94886208192143151 ) ) ;
#10273 = CIRCLE ( 'NONE', #29851, 32.00000000000000000 ) ;
#10274 = DIRECTION ( 'NONE',  ( -1.000000000000000000, -0.000000000000000000, -0.000000000000000000 ) ) ;
#10275 = ORIENTED_EDGE ( 'NONE', *, *, #31628, .T. ) ;
#10276 = CARTESIAN_POINT ( 'NONE',  ( 3.135527875058820690, 216.4958274776887492, 10.40113791807856636 ) ) ;
#10277 = CARTESIAN_POINT ( 'NONE',  ( -6.139770520408369237, 215.5359834540460042, 72.95113791807854398 ) ) ;
#10278 = ORIENTED_EDGE ( 'NONE', *, *, #18328, .T. ) ;
#10279 = CARTESIAN_POINT ( 'NONE',  ( -0.05014649552828365914, 215.4116977939061144, 36.24886208192143755 ) ) ;
#10280 = CARTESIAN_POINT ( 'NONE',  ( 89.50000000000002842, 155.0000000000000000, 0.000000000000000000 ) ) ;
#10281 = CARTESIAN_POINT ( 'NONE',  ( 74.77499999726880731, 140.1801316387863778, 4.815267126137185549 ) ) ;
#10282 = EDGE_LOOP ( 'NONE', ( #29905, #2385, #12773, #13718 ) ) ;
#10283 = CARTESIAN_POINT ( 'NONE',  ( 4.984841277089725686, 213.7757310962907411, 13.55113791807856849 ) ) ;
#10284 = CARTESIAN_POINT ( 'NONE',  ( 3.753561863808876797, 195.6020594897209719, 100.5988620819214532 ) ) ;
#10285 = CARTESIAN_POINT ( 'NONE',  ( 35.87499999726881583, 171.3844434931184253, -7.942151717890134290E-15 ) ) ;
#10286 = VERTEX_POINT ( 'NONE', #12228 ) ;
#10287 = CARTESIAN_POINT ( 'NONE',  ( 44.92499999726880588, 145.8408176439707802, -12.60653300113719588 ) ) ;
#10288 = FACE_OUTER_BOUND ( 'NONE', #17538, .T. ) ;
#10289 = CARTESIAN_POINT ( 'NONE',  ( 3.135527875058820690, 216.4958274776887492, 7.401137918078566358 ) ) ;
#10290 = CARTESIAN_POINT ( 'NONE',  ( -3.044812012439970683, 197.4746971517856196, 67.89886208192143613 ) ) ;
#10291 = CARTESIAN_POINT ( 'NONE',  ( 46.37499999726880873, 155.0000000000000000, 15.58253174999999402 ) ) ;
#10292 = CARTESIAN_POINT ( 'NONE',  ( 8.062137200540920645, 201.0835637161417822, 11.30113791807856671 ) ) ;
#10293 = PRODUCT_DEFINITION_SHAPE ( 'NONE', 'NONE',  #3132 ) ;
#10294 = DIRECTION ( 'NONE',  ( 0.000000000000000000, 1.000000000000000000, -1.290957005378097920E-14 ) ) ;
#10295 = VECTOR ( 'NONE', #13231, 1000.000000000000114 ) ;
#10296 = AXIS2_PLACEMENT_3D ( 'NONE', #29837, #27270, #14325 ) ;
#10297 = CARTESIAN_POINT ( 'NONE',  ( 67.29999999999999716, 163.5228861582408797, 11.73074641843673049 ) ) ;
#10298 = CARTESIAN_POINT ( 'NONE',  ( -0.05014649552810635652, 196.4853777576173002, 95.75113791807856956 ) ) ;
#10299 = CARTESIAN_POINT ( 'NONE',  ( 38.28867513459483263, 139.2280666364260071, -4.041636747397287284E-15 ) ) ;
#10300 = CARTESIAN_POINT ( 'NONE',  ( 9.984503880673470277, 203.7031108863295401, 74.15113791807854682 ) ) ;
#10301 = CARTESIAN_POINT ( 'NONE',  ( 85.88867513459484826, 150.1262045565064795, 15.00000000000005507 ) ) ;
#10302 = CARTESIAN_POINT ( 'NONE',  ( 3.500000000000004885, 2.020725942163676070, -2.899999999999999911 ) ) ;
#10303 = CARTESIAN_POINT ( 'NONE',  ( 12.01549611932659367, 203.1486557965466773, 100.1488620819214646 ) ) ;
#10304 = CARTESIAN_POINT ( 'NONE',  ( 72.82499999726879025, 141.7447067706911810, -9.630534252274385310 ) ) ;
#10305 = ORIENTED_EDGE ( 'NONE', *, *, #13935, .T. ) ;
#10306 = CARTESIAN_POINT ( 'NONE',  ( -125.0000000000000000, 25.00000000000000000, -20.00000000000000000 ) ) ;
#10307 = CARTESIAN_POINT ( 'NONE',  ( 86.57499999726880446, 145.8408176439707802, 12.60653300113718345 ) ) ;
#10308 = CARTESIAN_POINT ( 'NONE',  ( 9.680171189290831535, 199.9079932115568852, 95.30113791807858092 ) ) ;
#10309 = DIRECTION ( 'NONE',  ( 0.000000000000000000, 0.000000000000000000, 1.000000000000000000 ) ) ;
#10310 = ORIENTED_EDGE ( 'NONE', *, *, #16236, .T. ) ;
#10311 = CARTESIAN_POINT ( 'NONE',  ( -6.139770520408224463, 198.4640165459539105, 86.04886208192144181 ) ) ;
#10312 = CARTESIAN_POINT ( 'NONE',  ( 0.05014649552828288198, 194.3824533091408000, 19.74886208192143400 ) ) ;
#10313 = CARTESIAN_POINT ( 'NONE',  ( -64.50000000000000000, -2.605762844159085212, 20.00000000000000000 ) ) ;
#10314 = VECTOR ( 'NONE', #10468, 1000.000000000000000 ) ;
#10315 = CARTESIAN_POINT ( 'NONE',  ( 10.00000000000000711, 206.9523078486586201, 44.00113791807857666 ) ) ;
#10316 = EDGE_LOOP ( 'NONE', ( #26793, #21061, #3744, #244 ) ) ;
#10317 = CARTESIAN_POINT ( 'NONE',  ( 7.984503880673422316, 209.6470497212048372, 3.848862081921434530 ) ) ;
#10318 = AXIS2_PLACEMENT_3D ( 'NONE', #7849, #16001, #31023 ) ;
#10319 = CARTESIAN_POINT ( 'NONE',  ( 49.71132485994280614, 155.0000000000000000, -15.00000000000002487 ) ) ;
#10320 = ORIENTED_EDGE ( 'NONE', *, *, #15725, .T. ) ;
#10321 = CARTESIAN_POINT ( 'NONE',  ( 8.000000000000008882, 207.0476921513415220, 81.99886208192144466 ) ) ;
#10322 = ORIENTED_EDGE ( 'NONE', *, *, #25212, .T. ) ;
#10323 = EDGE_CURVE ( 'NONE', #16399, #19918, #14564, .T. ) ;
#10324 = DIRECTION ( 'NONE',  ( 1.000000000000000000, 0.000000000000000000, 0.000000000000000000 ) ) ;
#10325 = ORIENTED_EDGE ( 'NONE', *, *, #12185, .T. ) ;
#10326 = DIRECTION ( 'NONE',  ( 0.000000000000000000, 0.000000000000000000, -1.000000000000000000 ) ) ;
#10327 = CARTESIAN_POINT ( 'NONE',  ( -4.903702542908602524, 213.8346818373418898, 57.95113791807855819 ) ) ;
#10328 = CARTESIAN_POINT ( 'NONE',  ( 84.72499999726882436, 140.1801316387863778, -4.815267126137194431 ) ) ;
#10329 = DIRECTION ( 'NONE',  ( 0.000000000000000000, 1.000000000000000000, -3.227392513445223895E-15 ) ) ;
#10330 = CARTESIAN_POINT ( 'NONE',  ( 2.426778023690261410, 199.3768101843759837, 86.60113791807857808 ) ) ;
#10331 = DIRECTION ( 'NONE',  ( -0.000000000000000000, -0.000000000000000000, 1.000000000000000000 ) ) ;
#10332 = CARTESIAN_POINT ( 'NONE',  ( 49.99999999999999289, 139.7537977485451393, -4.138211985947621020E-15 ) ) ;
#10333 = CARTESIAN_POINT ( 'NONE',  ( 6.444103211790928043, 211.7408657792734061, 60.69886208192144750 ) ) ;
#10334 = AXIS2_PLACEMENT_3D ( 'NONE', #5466, #2757, #24020 ) ;
#10335 = DIRECTION ( 'NONE',  ( -0.000000000000000000, -0.000000000000000000, 1.000000000000000000 ) ) ;
#10336 = CARTESIAN_POINT ( 'NONE',  ( 54.12499999726881583, 155.0000000000000000, 15.58253174999999402 ) ) ;
#10337 = CARTESIAN_POINT ( 'NONE',  ( -8.062137200540920645, 212.9164362838581894, 3.801137918078565825 ) ) ;
#10338 = CARTESIAN_POINT ( 'NONE',  ( 100.3117322205716420, 155.0000000000000000, 0.000000000000000000 ) ) ;
#10339 = CARTESIAN_POINT ( 'NONE',  ( 57.82499999726880446, 168.2552932293087906, 9.630534252274372875 ) ) ;
#10340 = CARTESIAN_POINT ( 'NONE',  ( 72.97499999726881015, 140.1801316387863778, -4.815267126137194431 ) ) ;
#10341 = CARTESIAN_POINT ( 'NONE',  ( -3.662846001190052991, 218.4274158808045740, 64.10113791807857808 ) ) ;
#10342 = EDGE_CURVE ( 'NONE', #9697, #10890, #12379, .T. ) ;
#10343 = DIRECTION ( 'NONE',  ( 0.000000000000000000, 0.000000000000000000, 1.000000000000000000 ) ) ;
#10344 = CARTESIAN_POINT ( 'NONE',  ( -12.01549611932652972, 203.1486557965464499, 12.35113791807856565 ) ) ;
#10345 = CARTESIAN_POINT ( 'NONE',  ( -6.139770520408368348, 215.5359834540460042, 84.95113791807858661 ) ) ;
#10346 = CARTESIAN_POINT ( 'NONE',  ( -12.00000000000000711, 206.9523078486584780, 53.49886208192144466 ) ) ;
#10347 = CARTESIAN_POINT ( 'NONE',  ( 8.118202686958138514, 201.1607312380088501, 58.29886208192143471 ) ) ;
#10348 = CARTESIAN_POINT ( 'NONE',  ( 9.736236675707914401, 214.0148392665762458, 94.70113791807858661 ) ) ;
#10349 = CARTESIAN_POINT ( 'NONE',  ( -67.50001199999998391, 168.5168296348864203, -10.36982646209943759 ) ) ;
#10350 = CARTESIAN_POINT ( 'NONE',  ( -8.118202686958039038, 201.1607312380087080, 18.20113791807856884 ) ) ;
#10351 = CARTESIAN_POINT ( 'NONE',  ( 10.00000000000000711, 207.0476921513415220, 72.99886208192144466 ) ) ;
#10352 = ORIENTED_EDGE ( 'NONE', *, *, #9517, .F. ) ;
#10353 = CARTESIAN_POINT ( 'NONE',  ( -0.05014649552828442242, 219.6175466908591716, 78.24886208192144466 ) ) ;
#10354 = CARTESIAN_POINT ( 'NONE',  ( -9.898309971686792608, 228.3698647632124334, 103.4854814124440452 ) ) ;
#10355 = ORIENTED_EDGE ( 'NONE', *, *, #4985, .F. ) ;
#10356 = CARTESIAN_POINT ( 'NONE',  ( 76.37499999726881583, 155.0000000000000000, 15.58253174999999402 ) ) ;
#10357 = CARTESIAN_POINT ( 'NONE',  ( -2.517493886309087880, 214.5937144450984135, 51.09886208192143897 ) ) ;
#10358 = ORIENTED_EDGE ( 'NONE', *, *, #13073, .F. ) ;
#10359 = ADVANCED_FACE ( 'NONE', ( #22112 ), #26523, .T. ) ;
#10360 = CARTESIAN_POINT ( 'NONE',  ( 73.42499999726881299, 168.2552932293087906, -9.630534252274387086 ) ) ;
#10361 = CARTESIAN_POINT ( 'NONE',  ( 6.826581433398040133, -2.695947255479557381, -6.331032031596317999 ) ) ;
#10362 = CARTESIAN_POINT ( 'NONE',  ( -56.96409840163092753, 194.9506684299840913, -1.999309141333601492 ) ) ;
#10363 = CARTESIAN_POINT ( 'NONE',  ( 62.42499999726881299, 141.7447067706911810, 9.630534252274376428 ) ) ;
#10364 = CARTESIAN_POINT ( 'NONE',  ( -7.499999999999653610, -1.545780083834116247, -7.491787297939224821 ) ) ;
#10365 = CARTESIAN_POINT ( 'NONE',  ( 6.139770520408223575, 215.5359834540460611, 54.54886208192144181 ) ) ;
#10366 = VERTEX_POINT ( 'NONE', #11898 ) ;
#10367 = LINE ( 'NONE', #22960, #33620 ) ;
#10368 = EDGE_CURVE ( 'NONE', #2085, #25209, #12057, .T. ) ;
#10369 = CARTESIAN_POINT ( 'NONE',  ( 107.5000000000000000, 155.0000000000000000, 97.99999999999997158 ) ) ;
#10370 = CARTESIAN_POINT ( 'NONE',  ( -2.517493886309087880, 214.5937144450984135, 30.09886208192144252 ) ) ;
#10371 = CARTESIAN_POINT ( 'NONE',  ( -8.118202686958039038, 201.1607312380087080, 69.20113791807858661 ) ) ;
#10372 = FACE_OUTER_BOUND ( 'NONE', #20184, .T. ) ;
#10373 = CARTESIAN_POINT ( 'NONE',  ( -10.00000000000000711, 207.0476921513413515, 54.50113791807857666 ) ) ;
#10374 = CARTESIAN_POINT ( 'NONE',  ( 10.01549611932653860, 210.2015048109876716, 31.85113791807857453 ) ) ;
#10375 = CARTESIAN_POINT ( 'NONE',  ( -8.000000000000008882, 207.0476921513413515, 12.50113791807856600 ) ) ;
#10376 = CARTESIAN_POINT ( 'NONE',  ( -10.00000000000000178, 207.7681335166370502, 108.3800599224786367 ) ) ;
#10377 = FACE_OUTER_BOUND ( 'NONE', #30484, .T. ) ;
#10378 = CARTESIAN_POINT ( 'NONE',  ( 37.62499999726880873, 171.3844434931184253, -7.942151717890134290E-15 ) ) ;
#10379 = CARTESIAN_POINT ( 'NONE',  ( -0.05014649552807705357, 194.3824533091408000, 41.75113791807856245 ) ) ;
#10380 = LINE ( 'NONE', #13251, #18958 ) ;
#10381 = EDGE_CURVE ( 'NONE', #22604, #15895, #19389, .T. ) ;
#10382 = CARTESIAN_POINT ( 'NONE',  ( -0.05014649552810635652, 196.4853777576173002, 80.75113791807854113 ) ) ;
#10383 = CARTESIAN_POINT ( 'NONE',  ( 3.044812012440130555, 197.4746971517856764, 59.60113791807857808 ) ) ;
#10384 = DIRECTION ( 'NONE',  ( 1.000000000000000000, -0.000000000000000000, -0.000000000000000000 ) ) ;
#10385 = CARTESIAN_POINT ( 'NONE',  ( -11.98450388067341876, 203.0532714938636047, 23.34886208192143542 ) ) ;
#10386 = CARTESIAN_POINT ( 'NONE',  ( 9.984503880673420539, 210.2968891136705736, 24.84886208192143897 ) ) ;
#10387 = CARTESIAN_POINT ( 'NONE',  ( 78.39999999453763735, 168.7903194862797420, -4.480746418436745593 ) ) ;
#10388 = CARTESIAN_POINT ( 'NONE',  ( -9.736236675707914401, 199.9851607334237542, 66.20113791807857240 ) ) ;
#10389 = CARTESIAN_POINT ( 'NONE',  ( 0.05014649552807626948, 215.4116977939061144, 88.25113791807856956 ) ) ;
#10390 = ADVANCED_FACE ( 'NONE', ( #1338 ), #22283, .F. ) ;
#10391 = CARTESIAN_POINT ( 'NONE',  ( -9.984503880673420539, 203.7031108863293980, 44.34886208192142476 ) ) ;
#10392 = DIRECTION ( 'NONE',  ( 0.000000000000000000, 0.000000000000000000, -1.000000000000000000 ) ) ;
#10393 = ORIENTED_EDGE ( 'NONE', *, *, #20830, .F. ) ;
#10394 = CARTESIAN_POINT ( 'NONE',  ( 3.753561863808876797, 195.6020594897209719, 49.59886208192143897 ) ) ;
#10395 = AXIS2_PLACEMENT_3D ( 'NONE', #29788, #31831, #21278 ) ;
#10396 = VERTEX_POINT ( 'NONE', #16995 ) ;
#10397 = ORIENTED_EDGE ( 'NONE', *, *, #26748, .F. ) ;
#10398 = ADVANCED_FACE ( 'NONE', ( #22616 ), #14444, .T. ) ;
#10399 = DIRECTION ( 'NONE',  ( 1.000000000000000000, 0.000000000000000000, 0.000000000000000000 ) ) ;
#10400 = CARTESIAN_POINT ( 'NONE',  ( 56.48867513459482126, 142.2402378747194405, -9.270509831248439525 ) ) ;
#10401 = VERTEX_POINT ( 'NONE', #32666 ) ;
#10402 = CARTESIAN_POINT ( 'NONE',  ( -6.500168698208129925, 202.3363017425936050, 45.20113791807857240 ) ) ;
#10403 = CARTESIAN_POINT ( 'NONE',  ( -10.01549611932659722, 210.2015048109875011, 23.64886208192142902 ) ) ;
#10404 = CARTESIAN_POINT ( 'NONE',  ( 61.47499999726881015, 160.0630714827496206, -15.58253175000000823 ) ) ;
#10405 = VERTEX_POINT ( 'NONE', #4392 ) ;
#10406 = DIRECTION ( 'NONE',  ( -1.000000000000000000, 0.000000000000000000, 0.000000000000000000 ) ) ;
#10407 =( NAMED_UNIT ( * ) SI_UNIT ( $, .STERADIAN. ) SOLID_ANGLE_UNIT ( ) );
#10408 = FACE_OUTER_BOUND ( 'NONE', #24029, .T. ) ;
#10409 = CARTESIAN_POINT ( 'NONE',  ( 4.903702542908435547, 213.8346818373419751, 3.548862081921434264 ) ) ;
#10410 = CARTESIAN_POINT ( 'NONE',  ( 8.062137200540920645, 201.0835637161417822, 41.30113791807857382 ) ) ;
#10411 = DIRECTION ( 'NONE',  ( 0.000000000000000000, 0.000000000000000000, 1.000000000000000000 ) ) ;
#10412 = ADVANCED_FACE ( 'NONE', ( #30120 ), #17167, .F. ) ;
#10413 = CARTESIAN_POINT ( 'NONE',  ( -10.00000000000000711, 207.0476921513413515, 24.50113791807856600 ) ) ;
#10414 = CARTESIAN_POINT ( 'NONE',  ( -3.044812012439970683, 197.4746971517856196, 100.8988620819214361 ) ) ;
#10415 = DIRECTION ( 'NONE',  ( 1.224646799147353207E-16, -4.064521778635712183E-50, -1.000000000000000000 ) ) ;
#10416 = CIRCLE ( 'NONE', #27268, 5.249999999999991118 ) ;
#10417 = CARTESIAN_POINT ( 'NONE',  ( 6.444103211790928043, 211.7408657792734061, 96.69886208192144750 ) ) ;
#10418 = CARTESIAN_POINT ( 'NONE',  ( 33.92499999726881299, 164.1591823560292198, 12.60653300113718167 ) ) ;
#10419 = CARTESIAN_POINT ( 'NONE',  ( -56.84624105109630676, 194.9558714263463912, 1.881936590917415941 ) ) ;
#10420 = CARTESIAN_POINT ( 'NONE',  ( -4.000000000000000000, 4.898587196589412829E-16, -25.03750572909317285 ) ) ;
#10421 = CARTESIAN_POINT ( 'NONE',  ( 3.662846001190051659, 195.5725841191953691, 8.601137918078565647 ) ) ;
#10422 = CARTESIAN_POINT ( 'NONE',  ( 64.58867513459482268, 146.1832212156128890, -12.13525491562423042 ) ) ;
#10423 = CARTESIAN_POINT ( 'NONE',  ( 57.77499999726881441, 169.8198683612136222, -4.815267126137197984 ) ) ;
#10424 = ADVANCED_FACE ( 'NONE', ( #14955 ), #11555, .T. ) ;
#10425 = CARTESIAN_POINT ( 'NONE',  ( 0.05014649552810505201, 217.5146222423826714, 61.25113791807856245 ) ) ;
#10426 = DIRECTION ( 'NONE',  ( 0.000000000000000000, -0.5000000000000009992, -0.8660254037844380415 ) ) ;
#10427 = CARTESIAN_POINT ( 'NONE',  ( 42.31132485994280756, 169.2658477444273331, 4.635254915624208216 ) ) ;
#10428 = PLANE ( 'NONE',  #30421 ) ;
#10429 = CARTESIAN_POINT ( 'NONE',  ( 52.39999999453763024, 168.7903194862797420, -4.480746418436745593 ) ) ;
#10430 = VERTEX_POINT ( 'NONE', #16832 ) ;
#10431 = CARTESIAN_POINT ( 'NONE',  ( -9.736236675707914401, 199.9851607334237542, 42.20113791807857240 ) ) ;
#10432 = EDGE_CURVE ( 'NONE', #25081, #10143, #30325, .T. ) ;
#10433 = DIRECTION ( 'NONE',  ( 1.000000000000000000, -0.000000000000000000, -0.000000000000000000 ) ) ;
#10434 = CARTESIAN_POINT ( 'NONE',  ( -6.139770520408224463, 198.4640165459539389, 11.04886208192143648 ) ) ;
#10435 = CARTESIAN_POINT ( 'NONE',  ( 79.50000000000000000, 155.0000000000000000, -6.938893903907228378E-15 ) ) ;
#10436 = ORIENTED_EDGE ( 'NONE', *, *, #767, .F. ) ;
#10437 = CARTESIAN_POINT ( 'NONE',  ( 0.05014649552810505201, 217.5146222423826714, 7.251137918078566003 ) ) ;
#10438 = CARTESIAN_POINT ( 'NONE',  ( 3.135527875058820690, 216.4958274776887492, 70.40113791807857524 ) ) ;
#10439 = VERTEX_POINT ( 'NONE', #14616 ) ;
#10440 = CARTESIAN_POINT ( 'NONE',  ( 2.517493886309087436, 199.4062855549015865, 31.59886208192144252 ) ) ;
#10441 = DIRECTION ( 'NONE',  ( 1.000000000000000000, 0.000000000000000000, 0.000000000000000000 ) ) ;
#10442 = AXIS2_PLACEMENT_3D ( 'NONE', #21324, #18780, #718 ) ;
#10443 = ORIENTED_EDGE ( 'NONE', *, *, #18983, .F. ) ;
#10444 = CARTESIAN_POINT ( 'NONE',  ( 8.015496119326531499, 209.5516654185219636, 13.85113791807856742 ) ) ;
#10445 = CARTESIAN_POINT ( 'NONE',  ( 9.680171189290716072, 214.0920067884432854, 96.69886208192144750 ) ) ;
#10446 = CARTESIAN_POINT ( 'NONE',  ( 43.07499999726881867, 141.7447067706911810, -9.630534252274387086 ) ) ;
#10447 = ORIENTED_EDGE ( 'NONE', *, *, #5025, .F. ) ;
#10448 = CARTESIAN_POINT ( 'NONE',  ( 52.32499999726881157, 145.8408176439707802, 12.60653300113718345 ) ) ;
#10449 = CYLINDRICAL_SURFACE ( 'NONE', #18628, 2.149999999999985256 ) ;
#10450 = CARTESIAN_POINT ( 'NONE',  ( -9.984503880673473830, 210.2968891136704315, 9.651137918078568134 ) ) ;
#10451 = CARTESIAN_POINT ( 'NONE',  ( 3.135527875058981895, 197.5041725223112792, 79.59886208192143897 ) ) ;
#10452 = CARTESIAN_POINT ( 'NONE',  ( 51.77499999726881441, 169.8198683612136222, -4.815267126137197984 ) ) ;
#10453 = CARTESIAN_POINT ( 'NONE',  ( -67.50001199999998391, 149.5223338078428412, -16.13174377802661752 ) ) ;
#10454 = CARTESIAN_POINT ( 'NONE',  ( -9.984503880673473830, 210.2968891136704315, 12.65113791807856281 ) ) ;
#10455 = CARTESIAN_POINT ( 'NONE',  ( 93.60208470531338776, 155.0000000000000000, 0.000000000000000000 ) ) ;
#10456 = ADVANCED_FACE ( 'NONE', ( #25012 ), #20554, .T. ) ;
#10457 = CARTESIAN_POINT ( 'NONE',  ( 67.09999999999999432, 168.7903194862797420, 4.480746418436729606 ) ) ;
#10458 = CARTESIAN_POINT ( 'NONE',  ( 8.062137200540920645, 201.0835637161417822, 101.3011379180785809 ) ) ;
#10459 = CARTESIAN_POINT ( 'NONE',  ( 38.48867513459482126, 142.2402378747194405, -9.270509831248439525 ) ) ;
#10460 =( BOUNDED_SURFACE ( )  B_SPLINE_SURFACE ( 3, 2, ( 
 ( #10706, #26862, #18858 ),
 ( #6244, #29254, #16301 ),
 ( #8311, #3521, #16130 ),
 ( #18538, #16632, #26522 ),
 ( #21084, #10875, #3194 ),
 ( #11368, #13914, #478 ),
 ( #967, #21250, #13583 ),
 ( #24299, #21747, #19196 ) ),
 .UNSPECIFIED., .F., .F., .T. ) 
 B_SPLINE_SURFACE_WITH_KNOTS ( ( 4, 2, 2, 4 ),
 ( 3, 3 ),
 ( 0.03850042371095789562, 0.04313406099830585649, 0.04545087964197984387, 0.04776769828565382431 ),
 ( 0.000000000000000000, 1.000000000000000000 ),
 .UNSPECIFIED. ) 
 GEOMETRIC_REPRESENTATION_ITEM ( )  RATIONAL_B_SPLINE_SURFACE ( (
 ( 1.000000000000000000, 0.8047781847388135734, 1.000000000000000000),
 ( 1.000000000000000000, 0.8123760230793541925, 1.000000000000000000),
 ( 1.000000000000000000, 0.8190653851695529619, 1.000000000000000000),
 ( 1.000000000000000000, 0.8191940386278896424, 1.000000000000000000),
 ( 1.000000000000000000, 0.8176096570055705337, 1.000000000000000000),
 ( 1.000000000000000000, 0.8122964723277524834, 1.000000000000000000),
 ( 1.000000000000000000, 0.8086312464132844324, 1.000000000000000000),
 ( 1.000000000000000000, 0.8047712192439641088, 1.000000000000000000) ) ) 
 REPRESENTATION_ITEM ( '' )  SURFACE ( )  );
#10461 = CARTESIAN_POINT ( 'NONE',  ( -3.044812012440131443, 216.5253028482142952, 88.10113791807857808 ) ) ;
#10462 = DIRECTION ( 'NONE',  ( 0.000000000000000000, 0.000000000000000000, 1.000000000000000000 ) ) ;
#10463 = DIRECTION ( 'NONE',  ( -1.000000000000000000, 0.000000000000000000, 0.000000000000000000 ) ) ;
#10464 = ADVANCED_FACE ( 'NONE', ( #32837 ), #11290, .F. ) ;
#10465 = CARTESIAN_POINT ( 'NONE',  ( 0.05014649552828288198, 194.3824533091408000, 100.7488620819214304 ) ) ;
#10466 = CARTESIAN_POINT ( 'NONE',  ( 70.62499999726881583, 138.6155565068815463, -3.929120461958505118E-15 ) ) ;
#10467 = VERTEX_POINT ( 'NONE', #25170 ) ;
#10468 = DIRECTION ( 'NONE',  ( 1.000000000000000000, 1.804112415015879378E-16, 0.000000000000000000 ) ) ;
#10469 = CIRCLE ( 'NONE', #118, 0.2000000000000000944 ) ;
#10470 = CARTESIAN_POINT ( 'NONE',  ( 34.39999999453762314, 168.7903194862797420, -4.480746418436745593 ) ) ;
#10471 = CARTESIAN_POINT ( 'NONE',  ( 12.00000000000000711, 206.9523078486586485, 101.0011379180785696 ) ) ;
#10472 = DIRECTION ( 'NONE',  ( 0.000000000000000000, 0.000000000000000000, -1.000000000000000000 ) ) ;
#10473 = VERTEX_POINT ( 'NONE', #33004 ) ;
#10474 = CARTESIAN_POINT ( 'NONE',  ( 8.062137200540822946, 212.9164362838583315, 84.69886208192144750 ) ) ;
#10475 = CIRCLE ( 'NONE', #651, 2.500000000000000000 ) ;
#10476 = CARTESIAN_POINT ( 'NONE',  ( -3.753561863808878130, 218.3979405102790281, 24.09886208192143897 ) ) ;
#10477 = CARTESIAN_POINT ( 'NONE',  ( 13.75000000000000888, -23.81569860407206463, 0.000000000000000000 ) ) ;
#10478 = CARTESIAN_POINT ( 'NONE',  ( 3.044812012440130555, 197.4746971517856764, 44.60113791807857098 ) ) ;
#10479 = ORIENTED_EDGE ( 'NONE', *, *, #13743, .F. ) ;
#10480 = CARTESIAN_POINT ( 'NONE',  ( -6.500168698208244500, 211.6636982574061676, 2.798862081921434708 ) ) ;
#10481 = DIRECTION ( 'NONE',  ( 1.000000000000000000, 0.000000000000000000, 0.000000000000000000 ) ) ;
#10482 = ORIENTED_EDGE ( 'NONE', *, *, #28130, .T. ) ;
#10483 = CARTESIAN_POINT ( 'NONE',  ( 0.05014649552828262524, 198.5883022060938572, 91.74886208192144466 ) ) ;
#10484 = ORIENTED_EDGE ( 'NONE', *, *, #15948, .F. ) ;
#10485 = CARTESIAN_POINT ( 'NONE',  ( 4.903702542908601636, 200.1653181626581102, 35.45113791807857240 ) ) ;
#10486 = DIRECTION ( 'NONE',  ( -0.000000000000000000, -0.000000000000000000, 1.000000000000000000 ) ) ;
#10487 = EDGE_LOOP ( 'NONE', ( #14939, #1996, #15165, #9839 ) ) ;
#10488 = CARTESIAN_POINT ( 'NONE',  ( 2.411464220263165092, 7.267994521134541586, -7.491772860716163329 ) ) ;
#10489 = AXIS2_PLACEMENT_3D ( 'NONE', #29039, #15915, #3301 ) ;
#10490 = CARTESIAN_POINT ( 'NONE',  ( 84.82499999726880446, 141.7447067706911810, -9.630534252274385310 ) ) ;
#10491 = DIRECTION ( 'NONE',  ( 0.000000000000000000, 0.000000000000000000, -1.000000000000000000 ) ) ;
#10492 = CARTESIAN_POINT ( 'NONE',  ( -4.984841277089726574, 200.2242689037092305, 90.05113791807858092 ) ) ;
#10493 = CARTESIAN_POINT ( 'NONE',  ( -125.0000000000000000, -25.00000000000000000, 20.00000000000000000 ) ) ;
#10495 = CIRCLE ( 'NONE', #12640, 2.149999999999985256 ) ;
#10494 = DIRECTION ( 'NONE',  ( 0.000000000000000000, 0.000000000000000000, 1.000000000000000000 ) ) ;
#10496 = CARTESIAN_POINT ( 'NONE',  ( 46.40000000000000568, 150.2886644046228639, -14.50000000000000888 ) ) ;
#10497 = CARTESIAN_POINT ( 'NONE',  ( 2.517493886309087436, 199.4062855549015865, 67.59886208192143897 ) ) ;
#10498 = CARTESIAN_POINT ( 'NONE',  ( 27.50000000000000355, 0.000000000000000000, 0.000000000000000000 ) ) ;
#10499 = AXIS2_PLACEMENT_3D ( 'NONE', #9107, #26659, #6386 ) ;
#10500 = ADVANCED_FACE ( 'NONE', ( #33356 ), #4730, .F. ) ;
#10501 = CARTESIAN_POINT ( 'NONE',  ( 54.52499999726881441, 140.1801316387863778, 4.815267126137185549 ) ) ;
#10502 = CARTESIAN_POINT ( 'NONE',  ( 8.118202686958039038, 212.8392687619912635, 4.701137918078565292 ) ) ;
#10503 = DIRECTION ( 'NONE',  ( -0.000000000000000000, -0.000000000000000000, 1.000000000000000000 ) ) ;
#10504 = CARTESIAN_POINT ( 'NONE',  ( 56.92499999726881299, 145.8408176439707802, -12.60653300113719588 ) ) ;
#10505 = CARTESIAN_POINT ( 'NONE',  ( 68.07499999726881867, 168.2552932293087906, 9.630534252274372875 ) ) ;
#10506 = CARTESIAN_POINT ( 'NONE',  ( -7.456977232089304408, 196.8216656703010301, 66.05113791807858092 ) ) ;
#10507 = CARTESIAN_POINT ( 'NONE',  ( 145.0000000000000000, 3.306546357697854049E-14, -20.00000000000000355 ) ) ;
#10508 = CARTESIAN_POINT ( 'NONE',  ( -7.456977232089304408, 196.8216656703010301, 9.051137918078564937 ) ) ;
#10509 = CARTESIAN_POINT ( 'NONE',  ( 10.00000000000000711, 206.9523078486586201, 89.00113791807858377 ) ) ;
#10510 = CARTESIAN_POINT ( 'NONE',  ( -1.474514954580286030E-14, 206.9977241638431167, -6.000000000000014211 ) ) ;
#10511 = CARTESIAN_POINT ( 'NONE',  ( 12.00000000000000711, 207.0476921513415220, 51.99886208192143044 ) ) ;
#10512 = CARTESIAN_POINT ( 'NONE',  ( 0.05014649552828275014, 196.4853777576173002, 61.74886208192143755 ) ) ;
#10513 = CARTESIAN_POINT ( 'NONE',  ( -12.01549611932652972, 203.1486557965464499, 96.35113791807857808 ) ) ;
#10514 = CARTESIAN_POINT ( 'NONE',  ( -67.50001199999999812, 170.2801603273571516, 7.533570508255919229 ) ) ;
#10515 = CARTESIAN_POINT ( 'NONE',  ( 8.118202686958039038, 212.8392687619912635, 10.70113791807856529 ) ) ;
#10516 = CARTESIAN_POINT ( 'NONE',  ( -10.01549611932659722, 210.2015048109875011, 80.64886208192143613 ) ) ;
#10517 = ORIENTED_EDGE ( 'NONE', *, *, #27513, .F. ) ;
#10518 = CARTESIAN_POINT ( 'NONE',  ( -9.680171189290716072, 199.9079932115567146, 77.19886208192143329 ) ) ;
#10519 = CARTESIAN_POINT ( 'NONE',  ( 0.05014649552810505201, 217.5146222423826714, 97.25113791807854113 ) ) ;
#10520 = CIRCLE ( 'NONE', #20275, 1.000000000000000888 ) ;
#10521 = ORIENTED_EDGE ( 'NONE', *, *, #19173, .T. ) ;
#10522 = CARTESIAN_POINT ( 'NONE',  ( 2.547548355748054857E-16, 8.895721644649732696, -7.917989418073286600 ) ) ;
#10523 = CARTESIAN_POINT ( 'NONE',  ( -7.984503880673422316, 204.3529502787951628, 65.34886208192142476 ) ) ;
#10524 = VECTOR ( 'NONE', #25460, 1000.000000000000000 ) ;
#10525 = ORIENTED_EDGE ( 'NONE', *, *, #21669, .F. ) ;
#10526 = CARTESIAN_POINT ( 'NONE',  ( 72.82499999726879025, 141.7447067706911810, -9.630534252274387086 ) ) ;
#10527 = FACE_OUTER_BOUND ( 'NONE', #11847, .T. ) ;
#10528 = CARTESIAN_POINT ( 'NONE',  ( -57.39039945611308013, 194.9369330859559284, 2.246172506675526481 ) ) ;
#10529 = CARTESIAN_POINT ( 'NONE',  ( 63.82499999726881867, 168.2552932293087906, 9.630534252274372875 ) ) ;
#10530 = CARTESIAN_POINT ( 'NONE',  ( -7.908228835406498902, 3.123118350879302341, -7.776694659841278501 ) ) ;
#10531 = CARTESIAN_POINT ( 'NONE',  ( 3.135527875058981895, 197.5041725223112792, 55.59886208192143187 ) ) ;
#10532 = VERTEX_POINT ( 'NONE', #15792 ) ;
#10533 = CARTESIAN_POINT ( 'NONE',  ( 18.40782811468575986, 21.12650028821923698, -17.71727689882192891 ) ) ;
#10534 = AXIS2_PLACEMENT_3D ( 'NONE', #17982, #10149, #30763 ) ;
#10535 = FILL_AREA_STYLE ('',( #2700 ) ) ;
#10536 = LINE ( 'NONE', #31632, #28101 ) ;
#10537 = CARTESIAN_POINT ( 'NONE',  ( 0.05014649552828262524, 198.5883022060938572, 31.74886208192143755 ) ) ;
#10538 = CARTESIAN_POINT ( 'NONE',  ( 8.118202686958039038, 212.8392687619912635, 70.70113791807857240 ) ) ;
#10539 = DIRECTION ( 'NONE',  ( 0.000000000000000000, -1.000000000000000000, 0.000000000000000000 ) ) ;
#10540 = CARTESIAN_POINT ( 'NONE',  ( -3.135527875058821579, 197.5041725223112223, 59.90113791807856813 ) ) ;
#10541 = CARTESIAN_POINT ( 'NONE',  ( 9.984503880673470277, 203.7031108863295401, 23.15113791807856813 ) ) ;
#10542 = CARTESIAN_POINT ( 'NONE',  ( -8.015496119326531499, 204.4483345814780364, 12.35113791807856565 ) ) ;
#10543 = CARTESIAN_POINT ( 'NONE',  ( -6.837824896291514243, 3.947820044545427454, -6.564402953523716278 ) ) ;
#10544 = AXIS2_PLACEMENT_3D ( 'NONE', #19274, #11116, #27113 ) ;
#10545 = CARTESIAN_POINT ( 'NONE',  ( 39.62499999726880162, 171.3844434931184253, -7.942151717890134290E-15 ) ) ;
#10546 = CARTESIAN_POINT ( 'NONE',  ( 3.753561863808689836, 218.3979405102790565, 40.40113791807857524 ) ) ;
#10547 = DIRECTION ( 'NONE',  ( 0.000000000000000000, 0.000000000000000000, 1.000000000000000000 ) ) ;
#10548 = AXIS2_PLACEMENT_3D ( 'NONE', #9573, #6855, #20139 ) ;
#10549 = CARTESIAN_POINT ( 'NONE',  ( -8.118202686958039038, 201.1607312380087080, 84.20113791807858661 ) ) ;
#10550 = ADVANCED_FACE ( 'NONE', ( #10030 ), #9116, .T. ) ;
#10551 = CARTESIAN_POINT ( 'NONE',  ( -10.01549611932653860, 203.7984951890123000, 57.35113791807857098 ) ) ;
#10552 = CIRCLE ( 'NONE', #23598, 4.199999999999988631 ) ;
#10553 = CARTESIAN_POINT ( 'NONE',  ( 9.736236675708031640, 199.9851607334238963, 25.29886208192143826 ) ) ;
#10554 = CARTESIAN_POINT ( 'NONE',  ( -6.139770520408224463, 198.4640165459539105, 29.04886208192144181 ) ) ;
#10555 = CARTESIAN_POINT ( 'NONE',  ( 78.99999999453763166, 155.0000000000000000, 14.49999999999999467 ) ) ;
#10556 = CARTESIAN_POINT ( 'NONE',  ( 7.456977232089302632, 217.1783343296989131, 70.55113791807856671 ) ) ;
#10557 = CARTESIAN_POINT ( 'NONE',  ( 4.903702542908601636, 200.1653181626581102, 89.45113791807857240 ) ) ;
#10558 = CARTESIAN_POINT ( 'NONE',  ( -10.01549611932659722, 210.2015048109875011, 50.64886208192143613 ) ) ;
#10559 = CYLINDRICAL_SURFACE ( 'NONE', #8532, 15.00000000000001776 ) ;
#10560 = ORIENTED_EDGE ( 'NONE', *, *, #27240, .T. ) ;
#10561 = CARTESIAN_POINT ( 'NONE',  ( 7.375838497908012492, 217.2372850707501186, 51.54886208192144181 ) ) ;
#10562 = ORIENTED_EDGE ( 'NONE', *, *, #32280, .F. ) ;
#10563 = ORIENTED_EDGE ( 'NONE', *, *, #15365, .F. ) ;
#10564 = CARTESIAN_POINT ( 'NONE',  ( 50.88867513459482694, 159.8737954434936057, -15.00000000000002665 ) ) ;
#10565 = CARTESIAN_POINT ( 'NONE',  ( -60.00000000000000000, -7.347880794884118356E-15, 35.00000000000000000 ) ) ;
#10566 = CARTESIAN_POINT ( 'NONE',  ( 7.984503880673485376, 204.3529502787953902, 38.15113791807856813 ) ) ;
#10567 = CIRCLE ( 'NONE', #1843, 3.047499999999999876 ) ;
#10568 = DIRECTION ( 'NONE',  ( 0.8191520442889872466, 1.003171929053519200E-16, -0.5735764363510525987 ) ) ;
#10569 = CARTESIAN_POINT ( 'NONE',  ( 8.118202686958138514, 201.1607312380088501, 25.29886208192143826 ) ) ;
#10570 = CARTESIAN_POINT ( 'NONE',  ( 64.07499999726881867, 168.2552932293087906, 9.630534252274372875 ) ) ;
#10571 = ORIENTED_EDGE ( 'NONE', *, *, #32692, .T. ) ;
#10572 = LINE ( 'NONE', #2397, #5850 ) ;
#10573 =( NAMED_UNIT ( * ) SI_UNIT ( $, .STERADIAN. ) SOLID_ANGLE_UNIT ( ) );
#10574 = CARTESIAN_POINT ( 'NONE',  ( 32.50000000000000000, 155.0000000000000000, -15.00000000000002487 ) ) ;
#10575 = CARTESIAN_POINT ( 'NONE',  ( 4.903702542908435547, 213.8346818373419751, 6.548862081921434708 ) ) ;
#10576 = ADVANCED_FACE ( 'NONE', ( #5408 ), #15119, .F. ) ;
#10577 = CARTESIAN_POINT ( 'NONE',  ( -3.135527875058821579, 197.5041725223112223, 44.90113791807857524 ) ) ;
#10578 = CARTESIAN_POINT ( 'NONE',  ( 80.01132485994281751, 167.7597621252805880, -9.270509831248443078 ) ) ;
#10579 = CARTESIAN_POINT ( 'NONE',  ( 0.05014649552810505201, 217.5146222423826714, 31.25113791807857311 ) ) ;
#10580 = CARTESIAN_POINT ( 'NONE',  ( -9.945352646237287431, 205.9548993908332193, 104.4520571433695579 ) ) ;
#10581 = PRODUCT_CONTEXT ( 'NONE', #15501, 'mechanical' ) ;
#10582 = CARTESIAN_POINT ( 'NONE',  ( 7.984503880673422316, 209.6470497212048372, 90.84886208192142476 ) ) ;
#10583 = CARTESIAN_POINT ( 'NONE',  ( 84.60000000000000853, 159.7113355953771077, -14.50000000000000888 ) ) ;
#10584 = CARTESIAN_POINT ( 'NONE',  ( 81.58867513459483689, 163.8167787843871110, 12.13525491562421621 ) ) ;
#10585 = FACE_OUTER_BOUND ( 'NONE', #18134, .T. ) ;
#10586 = CARTESIAN_POINT ( 'NONE',  ( -3.662846001190052991, 218.4274158808045740, 7.101137918078566535 ) ) ;
#10587 = DIRECTION ( 'NONE',  ( 0.000000000000000000, 0.000000000000000000, 1.000000000000000000 ) ) ;
#10588 = CARTESIAN_POINT ( 'NONE',  ( 59.57499999726881157, 164.1591823560292198, -12.60653300113719766 ) ) ;
#10589 = CARTESIAN_POINT ( 'NONE',  ( -0.05014649552810635652, 196.4853777576173002, 56.75113791807855534 ) ) ;
#10590 = ADVANCED_FACE ( 'NONE', ( #13077 ), #17847, .F. ) ;
#10591 = CARTESIAN_POINT ( 'NONE',  ( 6.139770520408367460, 198.4640165459539389, 26.45113791807856884 ) ) ;
#10592 = CARTESIAN_POINT ( 'NONE',  ( 86.82499999726879025, 141.7447067706911810, -9.630534252274385310 ) ) ;
#10593 = CARTESIAN_POINT ( 'NONE',  ( 55.48867513459482836, 167.7597621252805880, 9.270509831248428867 ) ) ;
#10594 = DIRECTION ( 'NONE',  ( 0.000000000000000000, 0.000000000000000000, -1.000000000000000000 ) ) ;
#10595 = CIRCLE ( 'NONE', #14923, 4.250000000000000000 ) ;
#10596 = CARTESIAN_POINT ( 'NONE',  ( 61.69999999453762030, 142.6655632788954620, -8.961492836873480528 ) ) ;
#10597 = ORIENTED_EDGE ( 'NONE', *, *, #12033, .F. ) ;
#10598 = CARTESIAN_POINT ( 'NONE',  ( -3.753561863808691168, 195.6020594897209435, 41.90113791807856813 ) ) ;
#10599 = CARTESIAN_POINT ( 'NONE',  ( 36.98867513459482126, 163.8167787843871110, -12.13525491562423397 ) ) ;
#10600 = B_SPLINE_CURVE_WITH_KNOTS ( 'NONE', 3,
 ( #23702, #4852, #19845, #28017 ),
 .UNSPECIFIED., .F., .F.,
 ( 4, 4 ),
 ( 2.380739283024784782E-07, 0.002044882221487580917 ),
 .UNSPECIFIED. ) ;
#10601 = CARTESIAN_POINT ( 'NONE',  ( 10.00000000000000711, 207.0476921513415220, 18.99886208192143755 ) ) ;
#10602 = CARTESIAN_POINT ( 'NONE',  ( 59.61132485994281893, 150.1262045565063659, -14.99999999999998046 ) ) ;
#10603 = ORIENTED_EDGE ( 'NONE', *, *, #6042, .T. ) ;
#10604 = EDGE_CURVE ( 'NONE', #6898, #23864, #17158, .T. ) ;
#10605 = CARTESIAN_POINT ( 'NONE',  ( 8.062137200540920645, 201.0835637161417822, 68.30113791807856671 ) ) ;
#10606 = ORIENTED_EDGE ( 'NONE', *, *, #7462, .F. ) ;
#10607 = CARTESIAN_POINT ( 'NONE',  ( 44.61132485994281893, 159.8737954434936057, 15.00000000000003730 ) ) ;
#10608 = ORIENTED_EDGE ( 'NONE', *, *, #16895, .T. ) ;
#10609 = CARTESIAN_POINT ( 'NONE',  ( 7.984503880673485376, 204.3529502787953902, 17.15113791807856458 ) ) ;
#10610 = ADVANCED_FACE ( 'NONE', ( #20232 ), #7465, .T. ) ;
#10611 = CARTESIAN_POINT ( 'NONE',  ( 9.736236675708031640, 199.9851607334238963, 97.29886208192142760 ) ) ;
#10612 = CARTESIAN_POINT ( 'NONE',  ( 44.27499999726881441, 160.0630714827496206, 15.58253174999999224 ) ) ;
#10613 = ORIENTED_EDGE ( 'NONE', *, *, #33487, .T. ) ;
#10614 = CARTESIAN_POINT ( 'NONE',  ( 52.02499999726880020, 160.0630714827496206, 15.58253174999999402 ) ) ;
#10615 = CARTESIAN_POINT ( 'NONE',  ( 126.3741763928862269, 5.113356552508691699, 35.00001199999999102 ) ) ;
#10616 = CARTESIAN_POINT ( 'NONE',  ( -9.984503880673473830, 210.2968891136704315, 12.65113791807856281 ) ) ;
#10617 = CARTESIAN_POINT ( 'NONE',  ( 8.118202686958138514, 201.1607312380088501, 82.29886208192144181 ) ) ;
#10618 = ADVANCED_FACE ( 'NONE', ( #12568 ), #2183, .F. ) ;
#10619 = CARTESIAN_POINT ( 'NONE',  ( 54.27499999726880020, 160.0630714827496206, 15.58253174999999402 ) ) ;
#10620 = CARTESIAN_POINT ( 'NONE',  ( -67.50001199999998391, 143.7659452401275644, -12.80757580047017896 ) ) ;
#10621 = CARTESIAN_POINT ( 'NONE',  ( -3.135527875058821579, 197.5041725223112223, 11.90113791807856636 ) ) ;
#10622 = DIRECTION ( 'NONE',  ( -1.000000000000000000, -0.000000000000000000, -0.000000000000000000 ) ) ;
#10623 = CARTESIAN_POINT ( 'NONE',  ( 66.70000000000000284, 163.5228861582408797, -11.73074641843674470 ) ) ;
#10624 = DIRECTION ( 'NONE',  ( 0.000000000000000000, 0.000000000000000000, -1.000000000000000000 ) ) ;
#10625 = CARTESIAN_POINT ( 'NONE',  ( 22.99387487948480668, 18.47874495404628092, -1.090893241169154315 ) ) ;
#10626 = CARTESIAN_POINT ( 'NONE',  ( -10.00000000000000711, 207.0476921513413515, 84.50113791807856956 ) ) ;
#10627 = CARTESIAN_POINT ( 'NONE',  ( 86.78867513459481131, 155.0000000000000000, -15.00000000000002487 ) ) ;
#10628 = CARTESIAN_POINT ( 'NONE',  ( 35.17499999726881299, 145.8408176439707802, -12.60653300113719588 ) ) ;
#10629 = CARTESIAN_POINT ( 'NONE',  ( -3.753561863808878130, 218.3979405102790281, 93.09886208192145318 ) ) ;
#10630 = CARTESIAN_POINT ( 'NONE',  ( 70.42499999726881299, 141.7447067706911810, 9.630534252274376428 ) ) ;
#10631 = ORIENTED_EDGE ( 'NONE', *, *, #23137, .F. ) ;
#10632 = CARTESIAN_POINT ( 'NONE',  ( -59.14727863148851839, 194.9267258542059835, 2.420242894197758510 ) ) ;
#10633 = CARTESIAN_POINT ( 'NONE',  ( 41.39999999453762314, 141.2096805137202580, 4.480746418436733158 ) ) ;
#10634 = CARTESIAN_POINT ( 'NONE',  ( -9.736236675707914401, 199.9851607334237542, 93.20113791807858661 ) ) ;
#10635 = DIRECTION ( 'NONE',  ( 1.000000000000000000, -0.000000000000000000, -0.000000000000000000 ) ) ;
#10636 = EDGE_LOOP ( 'NONE', ( #27796, #3504 ) ) ;
#10637 = CARTESIAN_POINT ( 'NONE',  ( 6.139770520408223575, 215.5359834540460611, 96.54886208192142760 ) ) ;
#10638 = CARTESIAN_POINT ( 'NONE',  ( 3.753561863808876797, 195.6020594897209719, 19.59886208192143897 ) ) ;
#10639 = DIRECTION ( 'NONE',  ( 0.000000000000000000, 0.000000000000000000, 1.000000000000000000 ) ) ;
#10640 = CARTESIAN_POINT ( 'NONE',  ( -8.118202686958039038, 201.1607312380087080, 42.20113791807857240 ) ) ;
#10641 = ORIENTED_EDGE ( 'NONE', *, *, #23480, .T. ) ;
#10642 = CARTESIAN_POINT ( 'NONE',  ( -8.015496119326597224, 209.5516654185217362, 8.648862081921436129 ) ) ;
#10643 = EDGE_CURVE ( 'NONE', #16362, #32773, #10367, .T. ) ;
#10644 = ADVANCED_FACE ( 'NONE', ( #28749 ), #31137, .T. ) ;
#10645 = DIRECTION ( 'NONE',  ( 0.000000000000000000, 0.7071067811865475727, 0.7071067811865475727 ) ) ;
#10646 = EDGE_LOOP ( 'NONE', ( #3531, #16769, #2418, #28542, #6653, #5793 ) ) ;
#10647 = CARTESIAN_POINT ( 'NONE',  ( -4.903702542908436435, 200.1653181626580249, 86.04886208192145602 ) ) ;
#10648 = ADVANCED_FACE ( 'NONE', ( #28413 ), #4903, .F. ) ;
#10649 = CARTESIAN_POINT ( 'NONE',  ( -6.444103211791042618, 211.7408657792732356, 27.80113791807857027 ) ) ;
#10650 = CARTESIAN_POINT ( 'NONE',  ( 1.500000000000001332, 0.000000000000000000, 6.500000000000000888 ) ) ;
#10651 = ORIENTED_EDGE ( 'NONE', *, *, #8262, .T. ) ;
#10652 = CARTESIAN_POINT ( 'NONE',  ( 5.174575781541291164, 5.672711317429402378, -7.030005583190089169 ) ) ;
#10653 =( BOUNDED_CURVE ( )  B_SPLINE_CURVE ( 2, ( #27456, #33069, #17742, #15687, #31202, #23192, #8034, #10265, #25913, #2586, #3073 ),
 .UNSPECIFIED., .F., .T. ) 
 B_SPLINE_CURVE_WITH_KNOTS ( ( 3, 2, 2, 2, 2, 3 ),
 ( 0.5535714285714283811, 0.5571428571428569398, 0.5607142857142854986, 0.5642857142857141683, 0.5678571428571427271, 0.5714285714285712858 ),
 .UNSPECIFIED. ) 
 CURVE ( )  GEOMETRIC_REPRESENTATION_ITEM ( )  RATIONAL_B_SPLINE_CURVE ( ( 1.000000000000003109, 0.9510565162951504226, 1.000000000000000000, 0.9510565162951534202, 1.000000000000000000, 0.9510565162951534202, 1.000000000000000000, 0.9510565162951534202, 1.000000000000000000, 0.9510565162951549745, 0.9999999999999984457 ) ) 
 REPRESENTATION_ITEM ( '' )  );
#10654 = ADVANCED_FACE ( 'NONE', ( #20577 ), #2596, .T. ) ;
#10655 = CARTESIAN_POINT ( 'NONE',  ( 34.37499999726881583, 155.0000000000000000, 15.58253174999999402 ) ) ;
#10656 = CYLINDRICAL_SURFACE ( 'NONE', #17595, 2.149999999999985256 ) ;
#10657 = CARTESIAN_POINT ( 'NONE',  ( 4.903702542908601636, 200.1653181626581102, 92.45113791807857240 ) ) ;
#10658 = DIRECTION ( 'NONE',  ( 2.932322765073599105E-18, -0.9538853976007117819, -0.3001710316538423462 ) ) ;
#10659 = CARTESIAN_POINT ( 'NONE',  ( 49.30000000000000426, 163.5228861582408797, 11.73074641843673049 ) ) ;
#10660 = CARTESIAN_POINT ( 'NONE',  ( 8.015496119326595448, 204.4483345814782638, 64.14886208192143613 ) ) ;
#10661 = CARTESIAN_POINT ( 'NONE',  ( 0.000000000000000000, -1.759474945355381958, 3.047500000000001208 ) ) ;
#10662 = CARTESIAN_POINT ( 'NONE',  ( 49.92499999726881299, 164.1591823560292198, 12.60653300113718167 ) ) ;
#10663 = CARTESIAN_POINT ( 'NONE',  ( -9.984503880673475606, 210.2968891136704315, 0.6511379180785656917 ) ) ;
#10664 = DIRECTION ( 'NONE',  ( 1.000000000000000000, -4.625929269271484928E-16, 0.000000000000000000 ) ) ;
#10665 = CARTESIAN_POINT ( 'NONE',  ( 62.22499999726881015, 149.9369285172503510, 15.58253174999999580 ) ) ;
#10666 = CARTESIAN_POINT ( 'NONE',  ( 68.17499999726881299, 164.1591823560292198, 12.60653300113718167 ) ) ;
#10667 = CARTESIAN_POINT ( 'NONE',  ( 3.753561863808689836, 218.3979405102790565, 70.40113791807856103 ) ) ;
#10668 = CARTESIAN_POINT ( 'NONE',  ( 48.71132485994280614, 155.0000000000000000, 15.00000000000001243 ) ) ;
#10669 = CARTESIAN_POINT ( 'NONE',  ( 3.135527875058820690, 216.4958274776887492, 85.40113791807857524 ) ) ;
#10670 = CARTESIAN_POINT ( 'NONE',  ( 35.58867513459482268, 163.8167787843871110, 12.13525491562421621 ) ) ;
#10671 = CARTESIAN_POINT ( 'NONE',  ( 0.05014649552828288198, 194.3824533091408000, 49.74886208192143044 ) ) ;
#10672 = CARTESIAN_POINT ( 'NONE',  ( -3.044812012439970683, 197.4746971517856196, 58.89886208192143613 ) ) ;
#10673 = CARTESIAN_POINT ( 'NONE',  ( 12.01549611932652972, 210.8513442034534933, 94.85113791807856387 ) ) ;
#10674 = CARTESIAN_POINT ( 'NONE',  ( -67.50001199999999812, 169.7531371834000993, -8.519561460567018685 ) ) ;
#10675 = CARTESIAN_POINT ( 'NONE',  ( -0.05014649552810635652, 196.4853777576173002, 11.75113791807856778 ) ) ;
#10676 = CARTESIAN_POINT ( 'NONE',  ( 3.044812012439969795, 216.5253028482143520, 78.39886208192143613 ) ) ;
#10677 = ORIENTED_EDGE ( 'NONE', *, *, #30798, .F. ) ;
#10678 = CARTESIAN_POINT ( 'NONE',  ( 2.000000000000000000, 1.773042676681340968, -2.276824562219559311E-15 ) ) ;
#10679 = ORIENTED_EDGE ( 'NONE', *, *, #31581, .F. ) ;
#10680 = CARTESIAN_POINT ( 'NONE',  ( -2.426778023690076225, 199.3768101843759553, 61.89886208192143613 ) ) ;
#10681 = VERTEX_POINT ( 'NONE', #30980 ) ;
#10682 = CARTESIAN_POINT ( 'NONE',  ( 78.72499999726881015, 140.1801316387863778, -4.815267126137194431 ) ) ;
#10683 = CARTESIAN_POINT ( 'NONE',  ( 6.499999999999999112, 4.014041399406598210, -6.470356572124273953 ) ) ;
#10684 = CYLINDRICAL_SURFACE ( 'NONE', #32260, 1.000000000000000000 ) ;
#10685 = UNCERTAINTY_MEASURE_WITH_UNIT (LENGTH_MEASURE( 1.000000000000000082E-05 ), #29632, 'distance_accuracy_value', 'NONE');
#10686 = CARTESIAN_POINT ( 'NONE',  ( 67.42499999726879878, 168.2552932293087906, -9.630534252274385310 ) ) ;
#10687 = CARTESIAN_POINT ( 'NONE',  ( 7.984503880673485376, 204.3529502787953902, 56.15113791807857524 ) ) ;
#10688 = DIRECTION ( 'NONE',  ( 0.000000000000000000, 0.000000000000000000, -1.000000000000000000 ) ) ;
#10689 = CARTESIAN_POINT ( 'NONE',  ( 10.00000000000000711, 207.0476921513415220, 54.99886208192143755 ) ) ;
#10690 = AXIS2_PLACEMENT_3D ( 'NONE', #28518, #14880, #17609 ) ;
#10691 = DIRECTION ( 'NONE',  ( -1.000000000000000000, 0.000000000000000000, 0.000000000000000000 ) ) ;
#10692 = CIRCLE ( 'NONE', #6320, 37.00000000000000711 ) ;
#10693 =( NAMED_UNIT ( * ) SI_UNIT ( $, .STERADIAN. ) SOLID_ANGLE_UNIT ( ) );
#10694 = CARTESIAN_POINT ( 'NONE',  ( 0.000000000000000000, 0.000000000000000000, 0.000000000000000000 ) ) ;
#10695 = CARTESIAN_POINT ( 'NONE',  ( -4.984841277089891776, 213.7757310962905990, 32.94886208192144039 ) ) ;
#10696 = CARTESIAN_POINT ( 'NONE',  ( -0.05014649552810635652, 196.4853777576173002, 83.75113791807856956 ) ) ;
#10697 = CARTESIAN_POINT ( 'NONE',  ( 110.1179863365115636, 155.0000000000000000, 32.10452846326764131 ) ) ;
#10698 = CARTESIAN_POINT ( 'NONE',  ( 10.01549611932653860, 210.2015048109876716, 52.85113791807854966 ) ) ;
#10699 = VECTOR ( 'NONE', #32500, 1000.000000000000000 ) ;
#10700 = CARTESIAN_POINT ( 'NONE',  ( -8.118202686958039038, 201.1607312380087080, 27.20113791807856884 ) ) ;
#10701 = CARTESIAN_POINT ( 'NONE',  ( -2.517493886308901807, 199.4062855549015012, 14.90113791807856636 ) ) ;
#10702 = CARTESIAN_POINT ( 'NONE',  ( 46.28867513459482552, 139.2280666364260071, -4.041636747397287284E-15 ) ) ;
#10703 = DIRECTION ( 'NONE',  ( -1.000000000000000000, -0.000000000000000000, -0.000000000000000000 ) ) ;
#10704 = CARTESIAN_POINT ( 'NONE',  ( 44.52499999726881441, 140.1801316387863778, 4.815267126137185549 ) ) ;
#10705 = CARTESIAN_POINT ( 'NONE',  ( -12.00000000000000711, 207.0476921513413515, 39.50113791807856245 ) ) ;
#10706 = CARTESIAN_POINT ( 'NONE',  ( 7.500000000000000000, -4.730916290271713898, -7.493595886788494198 ) ) ;
#10707 = CARTESIAN_POINT ( 'NONE',  ( 8.062137200540920645, 201.0835637161417822, 86.30113791807856671 ) ) ;
#10708 = CARTESIAN_POINT ( 'NONE',  ( -3.135527875058821579, 197.5041725223112223, 59.90113791807856813 ) ) ;
#10709 = CARTESIAN_POINT ( 'NONE',  ( -0.05014649552828442242, 219.6175466908591716, 21.24886208192143755 ) ) ;
#10710 = CARTESIAN_POINT ( 'NONE',  ( 0.05014649552828275014, 196.4853777576173002, 25.74886208192143400 ) ) ;
#10711 = CARTESIAN_POINT ( 'NONE',  ( 81.79999999453762882, 146.4771138417591203, -11.73074641843674470 ) ) ;
#10712 = CARTESIAN_POINT ( 'NONE',  ( 9.680171189290831535, 199.9079932115568852, 71.30113791807856671 ) ) ;
#10713 = CARTESIAN_POINT ( 'NONE',  ( 4.903702542908601636, 200.1653181626581102, 92.45113791807857240 ) ) ;
#10714 = CARTESIAN_POINT ( 'NONE',  ( -6.220909254589682469, 215.4770327129946850, 53.94886208192144039 ) ) ;
#10715 = FACE_OUTER_BOUND ( 'NONE', #8688, .T. ) ;
#10716 = ORIENTED_EDGE ( 'NONE', *, *, #26464, .T. ) ;
#10717 = CARTESIAN_POINT ( 'NONE',  ( 3.753561863808876797, 195.6020594897209719, 55.59886208192143897 ) ) ;
#10718 = AXIS2_PLACEMENT_3D ( 'NONE', #19425, #29323, #31707 ) ;
#10719 = VERTEX_POINT ( 'NONE', #25858 ) ;
#10720 = EDGE_LOOP ( 'NONE', ( #10764, #7712, #26502, #30891, #16944 ) ) ;
#10721 = AXIS2_PLACEMENT_3D ( 'NONE', #3841, #17300, #6568 ) ;
#10722 = CARTESIAN_POINT ( 'NONE',  ( 86.78867513459481131, 155.0000000000000000, -15.00000000000002487 ) ) ;
#10723 = CARTESIAN_POINT ( 'NONE',  ( -60.00000000000000000, -7.347880794884118356E-15, 20.00000000000001776 ) ) ;
#10724 = CARTESIAN_POINT ( 'NONE',  ( -8.015496119326531499, 204.4483345814780364, 45.35113791807857098 ) ) ;
#10725 = DIRECTION ( 'NONE',  ( 1.000000000000000000, 0.000000000000000000, 0.000000000000000000 ) ) ;
#10726 = ADVANCED_FACE ( 'NONE', ( #2522 ), #20741, .T. ) ;
#10727 = CARTESIAN_POINT ( 'NONE',  ( -8.118202686958138514, 212.8392687619910930, 20.79886208192143471 ) ) ;
#10728 = CARTESIAN_POINT ( 'NONE',  ( 60.77499999726881441, 140.1801316387863778, 4.815267126137185549 ) ) ;
#10729 = ORIENTED_EDGE ( 'NONE', *, *, #15768, .F. ) ;
#10730 = CARTESIAN_POINT ( 'NONE',  ( 105.9028607166213192, 155.0000000000000000, 32.10452846326769816 ) ) ;
#10731 = CYLINDRICAL_SURFACE ( 'NONE', #11927, 15.00000000000001776 ) ;
#10732 = CARTESIAN_POINT ( 'NONE',  ( 4.903702542908435547, 213.8346818373419751, 9.548862081921432932 ) ) ;
#10733 = CIRCLE ( 'NONE', #29763, 1.535500000000000087 ) ;
#10734 = CARTESIAN_POINT ( 'NONE',  ( 10.00000000000000711, 206.9523078486586201, 47.00113791807856956 ) ) ;
#10735 = CARTESIAN_POINT ( 'NONE',  ( 87.31132485994280046, 140.7341522555726669, -4.635254915624220651 ) ) ;
#10736 = CARTESIAN_POINT ( 'NONE',  ( -3.135527875058821579, 197.5041725223112223, 26.90113791807856813 ) ) ;
#10737 = CARTESIAN_POINT ( 'NONE',  ( 85.87499999726881583, 171.3844434931184253, -7.942151717890132712E-15 ) ) ;
#10738 = AXIS2_PLACEMENT_3D ( 'NONE', #12932, #2380, #22645 ) ;
#10739 = ITEM_DEFINED_TRANSFORMATION ( 'NONE', 'NONE', #1754,  #2404 ) ;
#10740 = VECTOR ( 'NONE', #2850, 1000.000000000000000 ) ;
#10741 = CARTESIAN_POINT ( 'NONE',  ( 8.000000000000008882, 207.0476921513415220, 93.99886208192144466 ) ) ;
#10742 = CARTESIAN_POINT ( 'NONE',  ( 36.82499999726881157, 141.7447067706911810, -9.630534252274385310 ) ) ;
#10743 = PRESENTATION_STYLE_ASSIGNMENT (( #28468 ) ) ;
#10744 = DIRECTION ( 'NONE',  ( 1.000000000000000000, 0.000000000000000000, 0.000000000000000000 ) ) ;
#10745 = CARTESIAN_POINT ( 'NONE',  ( -12.00000000000000711, 207.0476921513413515, 6.501137918078566891 ) ) ;
#10746 = CARTESIAN_POINT ( 'NONE',  ( 64.68867513459485963, 150.1262045565065364, -15.00000000000012434 ) ) ;
#10747 = CARTESIAN_POINT ( 'NONE',  ( 56.27499999726880020, 160.0630714827496206, 15.58253174999999402 ) ) ;
#10748 = CARTESIAN_POINT ( 'NONE',  ( -10.00000000000000711, 207.0476921513413515, 54.50113791807857666 ) ) ;
#10749 = CARTESIAN_POINT ( 'NONE',  ( -6.220909254589537696, 198.5229672870051445, 33.05113791807857382 ) ) ;
#10750 = AXIS2_PLACEMENT_3D ( 'NONE', #8591, #6541, #9089 ) ;
#10751 = DIRECTION ( 'NONE',  ( -0.000000000000000000, -0.000000000000000000, 1.000000000000000000 ) ) ;
#10752 = CARTESIAN_POINT ( 'NONE',  ( -6.837824896291515131, -3.947820044545435447, -6.564402953523717166 ) ) ;
#10753 = LINE ( 'NONE', #23369, #20074 ) ;
#10754 = CARTESIAN_POINT ( 'NONE',  ( 62.59999999453763309, 168.7903194862797420, 4.480746418436729606 ) ) ;
#10755 = ORIENTED_EDGE ( 'NONE', *, *, #18143, .T. ) ;
#10756 = CARTESIAN_POINT ( 'NONE',  ( -7.375838497908182134, 217.2372850707499765, 42.95113791807857240 ) ) ;
#10757 = CARTESIAN_POINT ( 'NONE',  ( 117.5000000000000000, 155.0000000000000000, 98.00000000000000000 ) ) ;
#10758 = CARTESIAN_POINT ( 'NONE',  ( -0.05014649552828403384, 217.5146222423826714, 18.24886208192143755 ) ) ;
#10759 = CARTESIAN_POINT ( 'NONE',  ( 0.000000000000000000, 0.000000000000000000, -30.00000000000000000 ) ) ;
#10760 = EDGE_LOOP ( 'NONE', ( #10928, #5474, #4113, #30189 ) ) ;
#10761 = ADVANCED_FACE ( 'NONE', ( #15956 ), #26184, .T. ) ;
#10762 = CARTESIAN_POINT ( 'NONE',  ( -8.062137200540920645, 212.9164362838581894, 72.80113791807856671 ) ) ;
#10763 = TOROIDAL_SURFACE ( 'NONE', #27620, 1.000000000000059064, 1.000000000000000222 ) ;
#10764 = ORIENTED_EDGE ( 'NONE', *, *, #30412, .F. ) ;
#10765 = COLOUR_RGB ( '', 0.40784314, 0.44705882, 0.49803922) ;
#10766 = CARTESIAN_POINT ( 'NONE',  ( 67.50000000000000000, 155.0000000000000000, -6.938893903907228378E-15 ) ) ;
#10767 = VECTOR ( 'NONE', #19523, 1000.000000000000000 ) ;
#10768 = CARTESIAN_POINT ( 'NONE',  ( 44.21132485994281325, 170.7719333635740497, -7.904646289410545231E-15 ) ) ;
#10769 = VERTEX_POINT ( 'NONE', #8142 ) ;
#10770 = CARTESIAN_POINT ( 'NONE',  ( -0.05014649552807731031, 198.5883022060938572, 11.75113791807856600 ) ) ;
#10771 = EDGE_CURVE ( 'NONE', #31294, #25209, #23633, .T. ) ;
#10772 = CARTESIAN_POINT ( 'NONE',  ( -12.01549611932659722, 210.8513442034533227, 101.6488620819214361 ) ) ;
#10773 = CARTESIAN_POINT ( 'NONE',  ( 40.97499999726881725, 140.1801316387863778, -4.815267126137194431 ) ) ;
#10775 = ORIENTED_EDGE ( 'NONE', *, *, #23292, .F. ) ;
#10774 = CIRCLE ( 'NONE', #31982, 5.000000000000000888 ) ;
#10776 = CARTESIAN_POINT ( 'NONE',  ( 53.52499999726881441, 169.8198683612136222, -4.815267126137197984 ) ) ;
#10777 = CYLINDRICAL_SURFACE ( 'NONE', #27324, 32.00000000000001421 ) ;
#10778 = CARTESIAN_POINT ( 'NONE',  ( 10.01549611932653860, 210.2015048109876716, 4.851137918078563871 ) ) ;
#10779 = CARTESIAN_POINT ( 'NONE',  ( 8.062137200540822946, 212.9164362838583315, 78.69886208192143329 ) ) ;
#10780 = CARTESIAN_POINT ( 'NONE',  ( 52.37499999726881583, 155.0000000000000000, 15.58253174999999402 ) ) ;
#10781 = CARTESIAN_POINT ( 'NONE',  ( 2.000000000000000000, 0.8865213383406687075, -1.535500000000000975 ) ) ;
#10782 = CARTESIAN_POINT ( 'NONE',  ( 9.984503880673470277, 203.7031108863295401, 11.15113791807856636 ) ) ;
#10783 = DIRECTION ( 'NONE',  ( 0.000000000000000000, 1.000000000000000000, -1.100686371591861952E-15 ) ) ;
#10784 = EDGE_CURVE ( 'NONE', #2476, #24113, #13901, .T. ) ;
#10785 = CARTESIAN_POINT ( 'NONE',  ( 75.50000000000001421, 155.0000000000000000, 14.49999999999999467 ) ) ;
#10786 = CARTESIAN_POINT ( 'NONE',  ( 6.139770520408368348, 198.4640165459539674, 98.45113791807854398 ) ) ;
#10787 = CARTESIAN_POINT ( 'NONE',  ( 38.18867513459482410, 140.7341522555726669, 4.635254915624211769 ) ) ;
#10788 = CARTESIAN_POINT ( 'NONE',  ( 8.062137200540920645, 201.0835637161417822, 89.30113791807858092 ) ) ;
#10789 = CIRCLE ( 'NONE', #29276, 2.428571428571428381 ) ;
#10790 = CARTESIAN_POINT ( 'NONE',  ( 86.18867513459483121, 140.7341522555726669, 4.635254915624211769 ) ) ;
#10791 = CARTESIAN_POINT ( 'NONE',  ( 40.47499999726881725, 149.9369285172503510, 15.58253174999999580 ) ) ;
#10792 = CARTESIAN_POINT ( 'NONE',  ( -7.375838497908014268, 196.7627149292498530, 95.04886208192144181 ) ) ;
#10793 = AXIS2_PLACEMENT_3D ( 'NONE', #29824, #17376, #4084 ) ;
#10794 = CARTESIAN_POINT ( 'NONE',  ( 72.12499999726881583, 155.0000000000000000, 15.58253174999999402 ) ) ;
#10795 = ORIENTED_EDGE ( 'NONE', *, *, #5019, .F. ) ;
#10796 = DIRECTION ( 'NONE',  ( 0.000000000000000000, -0.7071067811865434649, 0.7071067811865515695 ) ) ;
#10797 = CARTESIAN_POINT ( 'NONE',  ( 40.89999999453763024, 159.7113355953771077, 14.49999999999999289 ) ) ;
#10798 = EDGE_CURVE ( 'NONE', #25814, #24261, #13897, .T. ) ;
#10799 = DIRECTION ( 'NONE',  ( 0.000000000000000000, 0.000000000000000000, 1.000000000000000000 ) ) ;
#10800 = AXIS2_PLACEMENT_3D ( 'NONE', #12371, #13050, #9823 ) ;
#10801 = CARTESIAN_POINT ( 'NONE',  ( -0.3875187462251565851, -8.436519985395204202, -7.781689322724289148 ) ) ;
#10802 = EDGE_LOOP ( 'NONE', ( #10830, #2122, #11554, #493 ) ) ;
#10803 = CARTESIAN_POINT ( 'NONE',  ( -9.984503880673420539, 203.7031108863293980, 95.34886208192143897 ) ) ;
#10804 = CARTESIAN_POINT ( 'NONE',  ( 7.375838497908012492, 217.2372850707501186, 33.54886208192143471 ) ) ;
#10805 = FACE_OUTER_BOUND ( 'NONE', #984, .T. ) ;
#10806 = CARTESIAN_POINT ( 'NONE',  ( 8.118202686958039038, 212.8392687619912635, 40.70113791807857240 ) ) ;
#10807 = ADVANCED_FACE ( 'NONE', ( #29578 ), #6231, .F. ) ;
#10808 = ORIENTED_EDGE ( 'NONE', *, *, #26337, .T. ) ;
#10809 = CARTESIAN_POINT ( 'NONE',  ( 3.135527875058981895, 197.5041725223112792, 103.5988620819214390 ) ) ;
#10810 = DIRECTION ( 'NONE',  ( -0.000000000000000000, 0.000000000000000000, -1.000000000000000000 ) ) ;
#10811 = ORIENTED_EDGE ( 'NONE', *, *, #1063, .F. ) ;
#10812 = CARTESIAN_POINT ( 'NONE',  ( 2.426778023690075337, 214.6231898156240447, 93.39886208192143613 ) ) ;
#10813 = CIRCLE ( 'NONE', #1556, 27.50000000000000355 ) ;
#10814 = AXIS2_PLACEMENT_3D ( 'NONE', #7117, #31131, #4897 ) ;
#10815 = CARTESIAN_POINT ( 'NONE',  ( 7.984503880673485376, 204.3529502787953902, 29.15113791807857169 ) ) ;
#10816 = FACE_OUTER_BOUND ( 'NONE', #8207, .T. ) ;
#10817 = ORIENTED_EDGE ( 'NONE', *, *, #19154, .T. ) ;
#10818 = CARTESIAN_POINT ( 'NONE',  ( 34.52499999726880731, 140.1801316387863778, 4.815267126137185549 ) ) ;
#10819 = AXIS2_PLACEMENT_3D ( 'NONE', #8873, #6313, #21653 ) ;
#10820 = CARTESIAN_POINT ( 'NONE',  ( 87.92499999726881299, 164.1591823560292198, 12.60653300113718167 ) ) ;
#10821 = CARTESIAN_POINT ( 'NONE',  ( -4.984841277089726574, 200.2242689037092305, 84.05113791807858092 ) ) ;
#10822 = CONICAL_SURFACE ( 'NONE', #6458, 32.10452846326769816, 1.466076571675243523 ) ;
#10823 = SURFACE_SIDE_STYLE ('',( #31274 ) ) ;
#10824 = CARTESIAN_POINT ( 'NONE',  ( 51.00000000000000711, 170.2462022514548323, -7.872454543227099337E-15 ) ) ;
#10825 = CARTESIAN_POINT ( 'NONE',  ( 2.517493886309087436, 199.4062855549015865, 73.59886208192142476 ) ) ;
#10826 = CARTESIAN_POINT ( 'NONE',  ( 84.11132485994279762, 169.2658477444273331, -4.635254915624224203 ) ) ;
#10827 = ADVANCED_FACE ( 'NONE', ( #28908 ), #463, .T. ) ;
#10828 = CARTESIAN_POINT ( 'NONE',  ( 51.72499999726881725, 169.8198683612136222, 4.815267126137181997 ) ) ;
#10830 = ORIENTED_EDGE ( 'NONE', *, *, #395, .F. ) ;
#10829 = CARTESIAN_POINT ( 'NONE',  ( -6.139770520408368348, 215.5359834540460042, 12.95113791807856174 ) ) ;
#10831 = CARTESIAN_POINT ( 'NONE',  ( 37.31132485994280756, 140.7341522555726669, -4.635254915624220651 ) ) ;
#10832 = CARTESIAN_POINT ( 'NONE',  ( 64.82499999726881867, 141.7447067706911810, -9.630534252274387086 ) ) ;
#10833 = CARTESIAN_POINT ( 'NONE',  ( 76.77499999726880731, 140.1801316387863778, 4.815267126137185549 ) ) ;
#10834 = CARTESIAN_POINT ( 'NONE',  ( -9.736236675707914401, 199.9851607334237542, 81.20113791807858661 ) ) ;
#10835 = CARTESIAN_POINT ( 'NONE',  ( 103.4083388212532810, 155.0000000000000000, 0.000000000000000000 ) ) ;
#10836 = CIRCLE ( 'NONE', #17913, 8.000000000000000000 ) ;
#10837 = EDGE_CURVE ( 'NONE', #3168, #9151, #13223, .T. ) ;
#10838 = CARTESIAN_POINT ( 'NONE',  ( -8.062137200540920645, 212.9164362838581894, 96.80113791807858092 ) ) ;
#10839 = CARTESIAN_POINT ( 'NONE',  ( 85.58867513459482268, 163.8167787843871110, 12.13525491562421621 ) ) ;
#10840 = ORIENTED_EDGE ( 'NONE', *, *, #15413, .T. ) ;
#10841 = AXIS2_PLACEMENT_3D ( 'NONE', #13987, #32048, #8711 ) ;
#10842 = CARTESIAN_POINT ( 'NONE',  ( 12.01549611932659367, 203.1486557965466773, 49.14886208192143613 ) ) ;
#10843 = CARTESIAN_POINT ( 'NONE',  ( -10.00000000000000711, 206.9523078486584495, 71.49886208192144466 ) ) ;
#10844 = CARTESIAN_POINT ( 'NONE',  ( -11.94915498584342295, 219.8409957184640291, 102.9933096652613642 ) ) ;
#10845 = DIRECTION ( 'NONE',  ( 1.000000000000000000, 0.000000000000000000, 0.000000000000000000 ) ) ;
#10846 = CARTESIAN_POINT ( 'NONE',  ( -8.062137200540920645, 212.9164362838581894, 12.80113791807856671 ) ) ;
#10847 = ADVANCED_FACE ( 'NONE', ( #21072 ), #2891, .F. ) ;
#10848 = CARTESIAN_POINT ( 'NONE',  ( 10.00000000000000711, 207.0476921513415220, 81.99886208192143044 ) ) ;
#10849 = ORIENTED_EDGE ( 'NONE', *, *, #213, .T. ) ;
#10850 = CARTESIAN_POINT ( 'NONE',  ( -8.062137200540920645, 212.9164362838581894, 99.80113791807858092 ) ) ;
#10851 = EDGE_LOOP ( 'NONE', ( #2768, #13759, #4344, #26480 ) ) ;
#10852 = FILL_AREA_STYLE_COLOUR ( '', #10765 ) ;
#10853 = CARTESIAN_POINT ( 'NONE',  ( 0.05014649552828262524, 198.5883022060938572, 58.74886208192143755 ) ) ;
#10854 = ORIENTED_EDGE ( 'NONE', *, *, #20018, .T. ) ;
#10855 = CARTESIAN_POINT ( 'NONE',  ( 80.52499999726880731, 140.1801316387863778, 4.815267126137185549 ) ) ;
#10856 = CARTESIAN_POINT ( 'NONE',  ( 32.50000000000000000, 155.0000000000000000, -6.938893903907228378E-15 ) ) ;
#10857 = DIRECTION ( 'NONE',  ( 0.000000000000000000, 0.000000000000000000, -1.000000000000000000 ) ) ;
#10858 = CIRCLE ( 'NONE', #520, 0.9999999999999968914 ) ;
#10859 = CARTESIAN_POINT ( 'NONE',  ( 70.22499999726879594, 149.9369285172503510, 15.58253174999999580 ) ) ;
#10860 = CARTESIAN_POINT ( 'NONE',  ( -6.444103211791042618, 211.7408657792732356, 54.80113791807857382 ) ) ;
#10861 = LINE ( 'NONE', #954, #12408 ) ;
#10862 = DIRECTION ( 'NONE',  ( -5.782411586589351722E-16, 0.000000000000000000, -1.000000000000000000 ) ) ;
#10863 = CARTESIAN_POINT ( 'NONE',  ( -67.50000000000000000, -92.00000000000000000, -17.00000000000001421 ) ) ;
#10864 = CARTESIAN_POINT ( 'NONE',  ( 6.500168698208244500, 202.3363017425938324, 34.29886208192144181 ) ) ;
#10865 = CARTESIAN_POINT ( 'NONE',  ( -9.984503880673473830, 210.2968891136704315, 84.65113791807857524 ) ) ;
#10866 = DIRECTION ( 'NONE',  ( -0.000000000000000000, -0.000000000000000000, -1.000000000000000000 ) ) ;
#10867 = CARTESIAN_POINT ( 'NONE',  ( 8.118202686958039038, 212.8392687619912635, 61.70113791807857240 ) ) ;
#10868 = EDGE_CURVE ( 'NONE', #82, #23658, #5565, .T. ) ;
#10869 = DIRECTION ( 'NONE',  ( -0.1045284632676468234, 1.217938055844715641E-16, -0.9945218953682740670 ) ) ;
#10870 = CARTESIAN_POINT ( 'NONE',  ( 6.444103211791042618, 202.2591342207267644, 11.30113791807856671 ) ) ;
#10871 = CARTESIAN_POINT ( 'NONE',  ( 126.3741763928862554, -5.113356552508631303, 35.00001200000001234 ) ) ;
#10872 = CARTESIAN_POINT ( 'NONE',  ( 59.88867513459482694, 150.1262045565063659, 14.99999999999997158 ) ) ;
#10873 = CARTESIAN_POINT ( 'NONE',  ( 41.42499999726881299, 168.2552932293087906, -9.630534252274387086 ) ) ;
#10874 = CARTESIAN_POINT ( 'NONE',  ( -7.375838497908182134, 217.2372850707499765, 42.95113791807857240 ) ) ;
#10875 = CARTESIAN_POINT ( 'NONE',  ( 7.500000000000000000, 1.545478204151513157, -7.491761935628701075 ) ) ;
#10876 = CARTESIAN_POINT ( 'NONE',  ( -0.05014649552810635652, 196.4853777576173002, 98.75113791807854113 ) ) ;
#10877 = ADVANCED_FACE ( 'NONE', ( #26510 ), #6058, .F. ) ;
#10878 = CARTESIAN_POINT ( 'NONE',  ( 9.984503880673473830, 203.7031108863295401, 62.15113791807857524 ) ) ;
#10879 = CARTESIAN_POINT ( 'NONE',  ( 7.375838497908012492, 217.2372850707501186, 18.54886208192143116 ) ) ;
#10880 = CARTESIAN_POINT ( 'NONE',  ( 6.139770520408223575, 215.5359834540460611, 42.54886208192142760 ) ) ;
#10881 = CARTESIAN_POINT ( 'NONE',  ( 76.49999999453761745, 170.2462022514548323, -7.872454543227099337E-15 ) ) ;
#10882 = CARTESIAN_POINT ( 'NONE',  ( 7.375838497908181246, 196.7627149292499666, 71.45113791807854398 ) ) ;
#10883 = VECTOR ( 'NONE', #32353, 1000.000000000000000 ) ;
#10884 = CARTESIAN_POINT ( 'NONE',  ( 6.444103211791042618, 202.2591342207267644, 92.30113791807858092 ) ) ;
#10885 = CARTESIAN_POINT ( 'NONE',  ( 0.05014649552828275708, 196.4853777576173002, 49.74886208192141623 ) ) ;
#10886 = DIRECTION ( 'NONE',  ( 0.000000000000000000, 0.000000000000000000, -1.000000000000000000 ) ) ;
#10887 = ORIENTED_EDGE ( 'NONE', *, *, #22513, .F. ) ;
#10888 = CARTESIAN_POINT ( 'NONE',  ( -9.680171189290716072, 199.9079932115567146, 50.19886208192144039 ) ) ;
#10889 = ORIENTED_EDGE ( 'NONE', *, *, #19928, .F. ) ;
#10890 = VERTEX_POINT ( 'NONE', #5892 ) ;
#10891 = CARTESIAN_POINT ( 'NONE',  ( 78.07499999726881867, 168.2552932293087906, 9.630534252274372875 ) ) ;
#10892 = DIRECTION ( 'NONE',  ( 0.000000000000000000, 0.000000000000000000, 1.000000000000000000 ) ) ;
#10893 = CARTESIAN_POINT ( 'NONE',  ( 92.60208470531341618, 155.0000000000000000, 12.10452846326763598 ) ) ;
#10894 = CARTESIAN_POINT ( 'NONE',  ( -2.517493886308901807, 199.4062855549015012, 41.90113791807856813 ) ) ;
#10895 = CARTESIAN_POINT ( 'NONE',  ( 8.062137200540822946, 212.9164362838583315, 24.69886208192143684 ) ) ;
#10896 = CARTESIAN_POINT ( 'NONE',  ( 60.07499999726880446, 168.2552932293087906, 9.630534252274372875 ) ) ;
#10897 = VERTEX_POINT ( 'NONE', #11022 ) ;
#10898 = CARTESIAN_POINT ( 'NONE',  ( 35.71132485994280614, 155.0000000000000000, -15.00000000000002487 ) ) ;
#10899 = PRESENTATION_STYLE_ASSIGNMENT (( #28792 ) ) ;
#10900 = FACE_OUTER_BOUND ( 'NONE', #7065, .T. ) ;
#10901 = CARTESIAN_POINT ( 'NONE',  ( 4.984841277089891776, 200.2242689037093726, 7.448862081921436840 ) ) ;
#10902 = CARTESIAN_POINT ( 'NONE',  ( 6.139770520408368348, 198.4640165459539674, 50.45113791807857240 ) ) ;
#10903 = PRODUCT_DEFINITION_SHAPE ( 'NONE', 'NONE',  #33717 ) ;
#10904 =( BOUNDED_CURVE ( )  B_SPLINE_CURVE ( 2, ( #23099, #15760, #22925, #12873, #269, #28382, #20376, #15590, #7431, #33488, #10157, #10663, #2662, #21039, #8109, #20540, #23266, #4869, #15430, #28034, #20708, #2317, #4695, #33320, #15257, #33661, #7607, #18162, #20881, #17812, #15085, #30942, #10337, #31109, #9990, #28556, #23435, #99, #10502, #31279, #18321, #28716, #5372, #26155, #2821, #13205, #25479, #23604, #5697, #18990, #8594, #759, #11490, #21204, #3307, #31762, #11321, #13535, #16086, #923, #13869, #29209, #21705, #31599, #6199, #21533, #2986, #1099, #18492, #29044, #11158, #14038, #3148, #26814, #21868, #23929, #8428, #16417, #3644, #592, #10987, #26479, #5860, #32262, #18654, #6025, #24435, #31923, #21366, #18814, #3477, #26644, #28875, #10829, #29380, #13691, #16258, #24254, #8264, #32096, #29545, #8758, #5531, #24092, #19147, #15922, #16587, #26979, #26320, #13366, #23762, #427, #14710, #6544, #9602, #22556, #24774, #24943, #32601, #1600, #6371, #9439, #11991, #12330, #27659, #8930, #17108, #1763, #30225, #19829, #14543, #25103, #27822, #32941, #1430, #6880, #27492, #16762, #4492, #22727, #1267, #25277, #3987, #14207, #22044, #9094, #24604, #14884, #12164, #17269, #11660, #32427, #1941, #27160, #27321, #4326, #14384, #30396, #3816, #6717, #19320, #29709, #7057, #11825, #19490, #22212, #29890, #19996, #16926, #17439, #9266, #19659, #30049, #4147, #22376, #32765, #26409, #30738, #33115, #17614, #20339, #16175, #12665, #10591, #7397, #31361, #13456, #23849, #524, #193, #13620, #21293, #13296, #17778, #25615, #18747, #3068, #28001, #5626, #2281, #15226, #10916, #8030, #28178, #4667, #31687, #3234, #4836, #23525, #31528, #29132, #20967, #18415, #16017, #28808, #8357, #5780, #5464, #15850, #26241, #2911, #33284, #348, #23688, #9780, #18582, #20164, #10749, #26564, #21129, #8197, #28967, #30561, #7223, #15051, #25446, #2121, #12503, #22892, #9951, #27410, #11739, #6630, #19073, #29300, #3397, #24186, #5951, #29972, #29806, #24520, #16341, #26735, #17016, #31848, #8682, #32351, #29462, #22126, #18905, #21790, #4070, #11083, #32516, #6114, #8511, #16510, #13791, #1352, #848, #21962, #6466, #11238, #24693, #21624, #9015, #32018, #16849, #26909, #24017, #3567, #16677, #681, #13957, #1018, #24350, #32182, #3896, #14292, #9189, #11413, #21464, #19579, #3738, #8842, #19242, #29637, #27242, #6284, #27074, #14127, #1177, #11573, #19404, #22465, #19744, #4746, #32856, #25187, #7484, #14633, #2029, #33375, #7140, #17360, #9519, #12416, #22632, #14458, #6798, #30478, #2200, #17524, #32681, #30819, #24854, #25030, #27913, #10049, #19906, #22811, #1517, #12582, #30305, #22300, #6972, #4235, #25532, #27568, #33202, #30652, #9689, #1682, #1855, #20426, #4583, #15137, #22975, #12075, #17869, #14970, #28265, #27746, #12245, #4409, #33020, #28084, #11914, #9348, #14794, #30140, #25358, #20083, #9865, #17185, #17696, #20248, #7319, #31153, #20755, #13548, #21253, #13092, #25873, #5422, #28766, #20930, #31646, #7654, #23482, #18209, #31323, #7820, #12922, #26200, #148, #4920, #30998, #7989, #10551, #28600, #15807, #18037, #18374, #15976, #2715, #15642, #2540, #2868, #5251, #8313, #26044, #13254, #23808, #10383, #23650, #10708, #23318, #5582, #18540, #309, #21087, #31490, #8158, #2370, #28922, #26369, #3029, #13414, #480, #18706, #10878, #15306, #25698, #12759, #23150, #33538, #10212, #20596, #28431, #5087, #15482, #24649, #32473, #21420, #13585, #11703, #808, #3523, #14250, #8801, #1315, #1140, #29597, #11037, #31806, #22088, #3196, #13746, #3692, #24142, #16804, #23978, #26866, #9141, #29093, #29758, #13916, #3355, #639, #19364, #11370, #5741, #8471, #24301, #8641, #21915, #11198, #26693, #11533, #24478, #32311, #6071, #8977, #18860, #27201, #32139, #29257, #16133, #26525, #5908, #16466, #21577, #27030, #19033, #16304, #31970, #29422, #3857, #970, #21750, #19198, #6247, #6423, #16634, #14083, #1983, #25318, #12374, #22770, #19699, #17145, #19867, #30607, #22420, #12543, #28042, #22934, #32644, #33163, #27708, #9826, #20207, #30440, #16969, #4703, #33329, #14421, #7272, #17654, #15093, #2160, #24990, #4369, #25488, #32979, #9644, #27365, #19538, #29932, #4032, #6586, #24814, #1477, #27865, #9307, #30093, #25143, #11872, #20040, #22257, #6760, #7100, #27531, #14592, #1641, #4193, #4539, #12032, #32811, #9477, #14751, #30263, #6925, #17317, #12205, #1809, #22592, #17480, #14930, #2670, #23273, #23442, #2827, #12714, #10001, #10166, #15597, #2497, #17819, #28564, #20548, #13052, #10345, #20888, #33670, #10669, #31449, #20385, #28220, #17999, #2993, #23108, #5212, #20716, #13211, #5047, #7615, #26161, #5379, #23610, #31116, #274, #33496, #8117, #107, #4878, #26327, #30777, #30953, #10509, #28390, #7947, #7778, #13372, #15439, #25835, #18498, #28883, #12880, #25999, #15266, #21047, #25658, #18169, #5539, #15766, #15929, #23769, #31286, #18329, #28723, #7439, #2326, #27166, #8936, #3821, #13544, #3649, #8599, #14044, #24440, #11327, #31605, #19326, #14213, #29051, #1104, #6205, #21875, #16767, #5867, #18996, #29714, #13875, #24259, #8273, #32269, #6377, #18660, #26986, #11497, #10838, #8765, #23937, #10994, #6033, #5704, #929, #436, #21212, #18821, #16092, #26652, #599, #26486, #21373, #32102, #16593, #31768, #3155, #8435, #19155, #29215, #16265, #3315, #13699, #24097, #26820, #765, #11163, #21538, #31928, #29385, #16424, #3483, #21712, #29551, #9444, #24781, #27665, #24949, #1769 ),
 .UNSPECIFIED., .F., .F. ) 
 B_SPLINE_CURVE_WITH_KNOTS ( ( 3, 2, 2, 2, 2, 2, 2, 2, 2, 2, 2, 2, 2, 2, 2, 2, 2, 2, 2, 2, 2, 2, 2, 2, 2, 2, 2, 2, 2, 2, 2, 2, 2, 2, 2, 2, 2, 2, 2, 2, 2, 2, 2, 2, 2, 2, 2, 2, 2, 2, 2, 2, 2, 2, 2, 2, 2, 2, 2, 2, 2, 2, 2, 2, 2, 2, 2, 2, 2, 2, 2, 2, 2, 2, 2, 2, 2, 2, 2, 2, 2, 2, 2, 2, 2, 2, 2, 2, 2, 2, 2, 2, 2, 2, 2, 2, 2, 2, 2, 2, 2, 2, 2, 2, 2, 2, 2, 2, 2, 2, 2, 2, 2, 2, 2, 2, 2, 2, 2, 2, 2, 2, 2, 2, 2, 2, 2, 2, 2, 2, 2, 2, 2, 2, 2, 2, 2, 2, 2, 2, 2, 2, 2, 2, 2, 2, 2, 2, 2, 2, 2, 2, 2, 2, 2, 2, 2, 2, 2, 2, 2, 2, 2, 2, 2, 2, 2, 2, 2, 2, 2, 2, 2, 2, 2, 2, 2, 2, 2, 2, 2, 2, 2, 2, 2, 2, 2, 2, 2, 2, 2, 2, 2, 2, 2, 2, 2, 2, 2, 2, 2, 2, 2, 2, 2, 2, 2, 2, 2, 2, 2, 2, 2, 2, 2, 2, 2, 2, 2, 2, 2, 2, 2, 2, 2, 2, 2, 2, 2, 2, 2, 2, 2, 2, 2, 2, 2, 2, 2, 2, 2, 2, 2, 2, 2, 2, 2, 2, 2, 2, 2, 2, 2, 2, 2, 2, 2, 2, 2, 2, 2, 2, 2, 2, 2, 2, 2, 2, 2, 2, 2, 2, 2, 2, 2, 2, 2, 2, 2, 2, 2, 2, 2, 2, 2, 2, 2, 2, 2, 2, 2, 2, 2, 2, 2, 2, 2, 2, 2, 2, 2, 2, 2, 2, 2, 2, 2, 2, 2, 2, 2, 2, 2, 2, 2, 2, 2, 2, 2, 2, 2, 2, 2, 2, 2, 2, 2, 2, 2, 2, 2, 2, 2, 2, 2, 2, 2, 2, 2, 2, 2, 2, 2, 2, 2, 2, 3 ),
 ( 0.000000000000000000, 0.002857142857142857140, 0.005714285714285714281, 0.008571428571428571855, 0.01142857142857142856, 0.01428571428571428527, 0.01714285714285714371, 0.02000000000000000042, 0.02285714285714285712, 0.02571428571428571383, 0.02857142857142857054, 0.03142857142857143071, 0.03428571428571428742, 0.03714285714285714413, 0.04000000000000000083, 0.04285714285714285754, 0.04571428571428571425, 0.04857142857142857095, 0.05142857142857142766, 0.05428571428571428437, 0.05714285714285714107, 0.05999999999999999778, 0.06285714285714286143, 0.06571428571428571119, 0.06857142857142857484, 0.07142857142857142461, 0.07428571428571428825, 0.07714285714285713802, 0.08000000000000000167, 0.08285714285714285143, 0.08571428571428571508, 0.08857142857142856485, 0.09142857142857142849, 0.09428571428571429214, 0.09714285714285714191, 0.1000000000000000056, 0.1028571428571428553, 0.1057142857142857190, 0.1085714285714285687, 0.1114285714285714324, 0.1142857142857142821, 0.1171428571428571458, 0.1199999999999999956, 0.1228571428571428592, 0.1257142857142857229, 0.1285714285714285587, 0.1314285714285714224, 0.1342857142857142860, 0.1371428571428571497, 0.1400000000000000133, 0.1428571428571428492, 0.1457142857142857129, 0.1485714285714285765, 0.1514285714285714401, 0.1542857142857142760, 0.1571428571428571397, 0.1600000000000000033, 0.1628571428571428670, 0.1657142857142857029, 0.1685714285714285665, 0.1714285714285714302, 0.1742857142857142938, 0.1771428571428571297, 0.1799999999999999933, 0.1828571428571428570, 0.1857142857142857206, 0.1885714285714285843, 0.1914285714285714202, 0.1942857142857142838, 0.1971428571428571475, 0.2000000000000000111, 0.2028571428571428470, 0.2057142857142857106, 0.2085714285714285743, 0.2114285714285714379, 0.2142857142857142738, 0.2171428571428571375, 0.2200000000000000011, 0.2228571428571428648, 0.2257142857142857006, 0.2285714285714285643, 0.2314285714285714279, 0.2342857142857142916, 0.2371428571428571552, 0.2399999999999999911, 0.2428571428571428548, 0.2457142857142857184, 0.2485714285714285821, 0.2514285714285714457, 0.2542857142857142816, 0.2571428571428571175, 0.2600000000000000089, 0.2628571428571428448, 0.2657142857142857362, 0.2685714285714285721, 0.2714285714285714080, 0.2742857142857142994, 0.2771428571428571352, 0.2800000000000000266, 0.2828571428571428625, 0.2857142857142856984, 0.2885714285714285898, 0.2914285714285714257, 0.2942857142857142616, 0.2971428571428571530, 0.2999999999999999889, 0.3028571428571428803, 0.3057142857142857162, 0.3085714285714285521, 0.3114285714285714435, 0.3142857142857142794, 0.3171428571428571153, 0.3200000000000000067, 0.3228571428571428426, 0.3257142857142857340, 0.3285714285714285698, 0.3314285714285714057, 0.3342857142857142971, 0.3371428571428571330, 0.3400000000000000244, 0.3428571428571428603, 0.3457142857142856962, 0.3485714285714285876, 0.3514285714285714235, 0.3542857142857142594, 0.3571428571428571508, 0.3599999999999999867, 0.3628571428571428781, 0.3657142857142857140, 0.3685714285714285499, 0.3714285714285714413, 0.3742857142857142771, 0.3771428571428571686, 0.3800000000000000044, 0.3828571428571428403, 0.3857142857142857317, 0.3885714285714285676, 0.3914285714285714035, 0.3942857142857142949, 0.3971428571428571308, 0.4000000000000000222, 0.4028571428571428581, 0.4057142857142856940, 0.4085714285714285854, 0.4114285714285714213, 0.4142857142857143127, 0.4171428571428571486, 0.4199999999999999845, 0.4228571428571428759, 0.4257142857142857117, 0.4285714285714285476, 0.4314285714285714390, 0.4342857142857142749, 0.4371428571428571663, 0.4400000000000000022, 0.4428571428571428381, 0.4457142857142857295, 0.4485714285714285654, 0.4514285714285714013, 0.4542857142857142927, 0.4571428571428571286, 0.4600000000000000200, 0.4628571428571428559, 0.4657142857142856918, 0.4685714285714285832, 0.4714285714285714191, 0.4742857142857143105, 0.4771428571428571463, 0.4799999999999999822, 0.4828571428571428736, 0.4857142857142857095, 0.4885714285714285454, 0.4914285714285714368, 0.4942857142857142727, 0.4971428571428571641, 0.5000000000000000000, 0.5028571428571428914, 0.5057142857142856718, 0.5085714285714285632, 0.5114285714285714546, 0.5142857142857142350, 0.5171428571428571264, 0.5200000000000000178, 0.5228571428571429092, 0.5257142857142856895, 0.5285714285714285809, 0.5314285714285714723, 0.5342857142857142527, 0.5371428571428571441, 0.5400000000000000355, 0.5428571428571428159, 0.5457142857142857073, 0.5485714285714285987, 0.5514285714285713791, 0.5542857142857142705, 0.5571428571428571619, 0.5600000000000000533, 0.5628571428571428337, 0.5657142857142857251, 0.5685714285714286165, 0.5714285714285713969, 0.5742857142857142883, 0.5771428571428571797, 0.5799999999999999600, 0.5828571428571428514, 0.5857142857142857428, 0.5885714285714285232, 0.5914285714285714146, 0.5942857142857143060, 0.5971428571428571974, 0.5999999999999999778, 0.6028571428571428692, 0.6057142857142857606, 0.6085714285714285410, 0.6114285714285714324, 0.6142857142857143238, 0.6171428571428571042, 0.6199999999999999956, 0.6228571428571428870, 0.6257142857142856673, 0.6285714285714285587, 0.6314285714285714501, 0.6342857142857142305, 0.6371428571428571219, 0.6400000000000000133, 0.6428571428571429047, 0.6457142857142856851, 0.6485714285714285765, 0.6514285714285714679, 0.6542857142857142483, 0.6571428571428571397, 0.6600000000000000311, 0.6628571428571428115, 0.6657142857142857029, 0.6685714285714285943, 0.6714285714285713746, 0.6742857142857142660, 0.6771428571428571574, 0.6800000000000000488, 0.6828571428571428292, 0.6857142857142857206, 0.6885714285714286120, 0.6914285714285713924, 0.6942857142857142838, 0.6971428571428571752, 0.6999999999999999556, 0.7028571428571428470, 0.7057142857142857384, 0.7085714285714285188, 0.7114285714285714102, 0.7142857142857143016, 0.7171428571428571930, 0.7199999999999999734, 0.7228571428571428648, 0.7257142857142857562, 0.7285714285714285365, 0.7314285714285714279, 0.7342857142857143193, 0.7371428571428570997, 0.7399999999999999911, 0.7428571428571428825, 0.7457142857142856629, 0.7485714285714285543, 0.7514285714285714457, 0.7542857142857143371, 0.7571428571428571175, 0.7600000000000000089, 0.7628571428571429003, 0.7657142857142856807, 0.7685714285714285721, 0.7714285714285714635, 0.7742857142857142438, 0.7771428571428571352, 0.7800000000000000266, 0.7828571428571428070, 0.7857142857142856984, 0.7885714285714285898, 0.7914285714285714812, 0.7942857142857142616, 0.7971428571428571530, 0.8000000000000000444, 0.8028571428571428248, 0.8057142857142857162, 0.8085714285714286076, 0.8114285714285713880, 0.8142857142857142794, 0.8171428571428571708, 0.8199999999999999512, 0.8228571428571428426, 0.8257142857142857340, 0.8285714285714286254, 0.8314285714285714057, 0.8342857142857142971, 0.8371428571428571885, 0.8399999999999999689, 0.8428571428571428603, 0.8457142857142857517, 0.8485714285714285321, 0.8514285714285714235, 0.8542857142857143149, 0.8571428571428570953, 0.8599999999999999867, 0.8628571428571428781, 0.8657142857142857695, 0.8685714285714285499, 0.8714285714285714413, 0.8742857142857143327, 0.8771428571428571130, 0.8800000000000000044, 0.8828571428571428958, 0.8857142857142856762, 0.8885714285714285676, 0.8914285714285714590, 0.8942857142857142394, 0.8971428571428571308, 0.9000000000000000222, 0.9028571428571428026, 0.9057142857142856940, 0.9085714285714285854, 0.9114285714285714768, 0.9142857142857142572, 0.9171428571428571486, 0.9200000000000000400, 0.9228571428571428203, 0.9257142857142857117, 0.9285714285714286031, 0.9314285714285713835, 0.9342857142857142749, 0.9371428571428571663, 0.9399999999999999467, 0.9428571428571428381, 0.9457142857142857295, 0.9485714285714286209, 0.9514285714285714013, 0.9542857142857142927, 0.9571428571428571841, 0.9599999999999999645, 0.9628571428571428559, 0.9657142857142857473, 0.9685714285714285277, 0.9714285714285714191, 0.9742857142857143105, 0.9771428571428570908, 0.9799999999999999822, 0.9828571428571428736, 0.9857142857142857650, 0.9860665758260036551 ),
 .UNSPECIFIED. ) 
 CURVE ( )  GEOMETRIC_REPRESENTATION_ITEM ( )  RATIONAL_B_SPLINE_CURVE ( ( 1.000000000000000000, 0.9510565162951535312, 1.000000000000000000, 0.9510565162951535312, 1.000000000000000000, 0.9510565162951535312, 1.000000000000000000, 0.9510565162951535312, 1.000000000000000000, 0.9510565162951535312, 1.000000000000000000, 0.9510565162951535312, 1.000000000000000000, 0.9510565162951535312, 1.000000000000000000, 0.9510565162951535312, 1.000000000000000000, 0.9510565162951535312, 1.000000000000000000, 0.9510565162951535312, 1.000000000000000000, 0.9510565162951535312, 1.000000000000000000, 0.9510565162951535312, 1.000000000000000000, 0.9510565162951535312, 1.000000000000000000, 0.9510565162951535312, 1.000000000000000000, 0.9510565162951535312, 1.000000000000000000, 0.9510565162951535312, 1.000000000000000000, 0.9510565162951535312, 1.000000000000000000, 0.9510565162951535312, 1.000000000000000000, 0.9510565162951535312, 1.000000000000000000, 0.9510565162951535312, 1.000000000000000000, 0.9510565162951535312, 1.000000000000000000, 0.9510565162951535312, 1.000000000000000000, 0.9510565162951535312, 1.000000000000000000, 0.9510565162951535312, 1.000000000000000000, 0.9510565162951535312, 1.000000000000000000, 0.9510565162951535312, 1.000000000000000000, 0.9510565162951535312, 1.000000000000000000, 0.9510565162951535312, 1.000000000000000000, 0.9510565162951535312, 1.000000000000000000, 0.9510565162951535312, 1.000000000000000000, 0.9510565162951535312, 1.000000000000000000, 0.9510565162951535312, 1.000000000000000000, 0.9510565162951535312, 1.000000000000000000, 0.9510565162951535312, 1.000000000000000000, 0.9510565162951535312, 1.000000000000000000, 0.9510565162951535312, 1.000000000000000000, 0.9510565162951535312, 1.000000000000000000, 0.9510565162951535312, 1.000000000000000000, 0.9510565162951535312, 1.000000000000000000, 0.9510565162951535312, 1.000000000000000000, 0.9510565162951535312, 1.000000000000000000, 0.9510565162951535312, 1.000000000000000000, 0.9510565162951535312, 1.000000000000000000, 0.9510565162951535312, 1.000000000000000000, 0.9510565162951535312, 1.000000000000000000, 0.9510565162951535312, 1.000000000000000000, 0.9510565162951535312, 1.000000000000000000, 0.9510565162951535312, 1.000000000000000000, 0.9510565162951535312, 1.000000000000000000, 0.9510565162951535312, 1.000000000000000000, 0.9510565162951535312, 1.000000000000000000, 0.9510565162951535312, 1.000000000000000000, 0.9510565162951535312, 1.000000000000000000, 0.9510565162951535312, 1.000000000000000000, 0.9510565162951535312, 1.000000000000000000, 0.9510565162951535312, 1.000000000000000000, 0.9510565162951535312, 1.000000000000000000, 0.9510565162951535312, 1.000000000000000000, 0.9510565162951535312, 1.000000000000000000, 0.9510565162951535312, 1.000000000000000000, 0.9510565162951535312, 1.000000000000000000, 0.9510565162951535312, 1.000000000000000000, 0.9510565162951535312, 1.000000000000000000, 0.9510565162951535312, 1.000000000000000000, 0.9510565162951535312, 1.000000000000000000, 0.9510565162951535312, 1.000000000000000000, 0.9510565162951535312, 1.000000000000000000, 0.9510565162951535312, 1.000000000000000000, 0.9510565162951535312, 1.000000000000000000, 0.9510565162951535312, 1.000000000000000000, 0.9510565162951535312, 1.000000000000000000, 0.9510565162951535312, 1.000000000000000000, 0.9510565162951535312, 1.000000000000000000, 0.9510565162951535312, 1.000000000000000000, 0.9510565162951535312, 1.000000000000000000, 0.9510565162951535312, 1.000000000000000000, 0.9510565162951535312, 1.000000000000000000, 0.9510565162951535312, 1.000000000000000000, 0.9510565162951535312, 1.000000000000000000, 0.9510565162951535312, 1.000000000000000000, 0.9510565162951535312, 1.000000000000000000, 0.9510565162951535312, 1.000000000000000000, 0.9510565162951535312, 1.000000000000000000, 0.9510565162951535312, 1.000000000000000000, 0.9510565162951535312, 1.000000000000000000, 0.9510565162951535312, 1.000000000000000000, 0.9510565162951535312, 1.000000000000000000, 0.9510565162951535312, 1.000000000000000000, 0.9510565162951535312, 1.000000000000000000, 0.9510565162951535312, 1.000000000000000000, 0.9510565162951535312, 1.000000000000000000, 0.9510565162951535312, 1.000000000000000000, 0.9510565162951535312, 1.000000000000000000, 0.9510565162951535312, 1.000000000000000000, 0.9510565162951535312, 1.000000000000000000, 0.9510565162951535312, 1.000000000000000000, 0.9510565162951535312, 1.000000000000000000, 0.9510565162951535312, 1.000000000000000000, 0.9510565162951535312, 1.000000000000000000, 0.9510565162951535312, 1.000000000000000000, 0.9510565162951535312, 1.000000000000000000, 0.9510565162951535312, 1.000000000000000000, 0.9510565162951535312, 1.000000000000000000, 0.9510565162951535312, 1.000000000000000000, 0.9510565162951535312, 1.000000000000000000, 0.9510565162951535312, 1.000000000000000000, 0.9510565162951535312, 1.000000000000000000, 0.9510565162951535312, 1.000000000000000000, 0.9510565162951535312, 1.000000000000000000, 0.9510565162951535312, 1.000000000000000000, 0.9510565162951535312, 1.000000000000000000, 0.9510565162951535312, 1.000000000000000000, 0.9510565162951535312, 1.000000000000000000, 0.9510565162951535312, 1.000000000000000000, 0.9510565162951535312, 1.000000000000000000, 0.9510565162951535312, 1.000000000000000000, 0.9510565162951535312, 1.000000000000000000, 0.9510565162951535312, 1.000000000000000000, 0.9510565162951535312, 1.000000000000000000, 0.9510565162951535312, 1.000000000000000000, 0.9510565162951535312, 1.000000000000000000, 0.9510565162951535312, 1.000000000000000000, 0.9510565162951535312, 1.000000000000000000, 0.9510565162951535312, 1.000000000000000000, 0.9510565162951535312, 1.000000000000000000, 0.9510565162951535312, 1.000000000000000000, 0.9510565162951535312, 1.000000000000000000, 0.9510565162951535312, 1.000000000000000000, 0.9510565162951535312, 1.000000000000000000, 0.9510565162951535312, 1.000000000000000000, 0.9510565162951535312, 1.000000000000000000, 0.9510565162951535312, 1.000000000000000000, 0.9510565162951535312, 1.000000000000000000, 0.9510565162951535312, 1.000000000000000000, 0.9510565162951535312, 1.000000000000000000, 0.9510565162951535312, 1.000000000000000000, 0.9510565162951535312, 1.000000000000000000, 0.9510565162951535312, 1.000000000000000000, 0.9510565162951535312, 1.000000000000000000, 0.9510565162951535312, 1.000000000000000000, 0.9510565162951535312, 1.000000000000000000, 0.9510565162951535312, 1.000000000000000000, 0.9510565162951535312, 1.000000000000000000, 0.9510565162951535312, 1.000000000000000000, 0.9510565162951535312, 1.000000000000000000, 0.9510565162951535312, 1.000000000000000000, 0.9510565162951535312, 1.000000000000000000, 0.9510565162951535312, 1.000000000000000000, 0.9510565162951535312, 1.000000000000000000, 0.9510565162951535312, 1.000000000000000000, 0.9510565162951535312, 1.000000000000000000, 0.9510565162951535312, 1.000000000000000000, 0.9510565162951535312, 1.000000000000000000, 0.9510565162951535312, 1.000000000000000000, 0.9510565162951535312, 1.000000000000000000, 0.9510565162951535312, 1.000000000000000000, 0.9510565162951535312, 1.000000000000000000, 0.9510565162951535312, 1.000000000000000000, 0.9510565162951535312, 1.000000000000000000, 0.9510565162951535312, 1.000000000000000000, 0.9510565162951535312, 1.000000000000000000, 0.9510565162951535312, 1.000000000000000000, 0.9510565162951535312, 1.000000000000000000, 0.9510565162951535312, 1.000000000000000000, 0.9510565162951535312, 1.000000000000000000, 0.9510565162951535312, 1.000000000000000000, 0.9510565162951535312, 1.000000000000000000, 0.9510565162951535312, 1.000000000000000000, 0.9510565162951535312, 1.000000000000000000, 0.9510565162951535312, 1.000000000000000000, 0.9510565162951535312, 1.000000000000000000, 0.9510565162951535312, 1.000000000000000000, 0.9510565162951535312, 1.000000000000000000, 0.9510565162951535312, 1.000000000000000000, 0.9510565162951535312, 1.000000000000000000, 0.9510565162951535312, 1.000000000000000000, 0.9510565162951535312, 1.000000000000000000, 0.9510565162951535312, 1.000000000000000000, 0.9510565162951535312, 1.000000000000000000, 0.9510565162951535312, 1.000000000000000000, 0.9510565162951535312, 1.000000000000000000, 0.9510565162951535312, 1.000000000000000000, 0.9510565162951535312, 1.000000000000000000, 0.9510565162951535312, 1.000000000000000000, 0.9510565162951535312, 1.000000000000000000, 0.9510565162951535312, 1.000000000000000000, 0.9510565162951535312, 1.000000000000000000, 0.9510565162951535312, 1.000000000000000000, 0.9510565162951535312, 1.000000000000000000, 0.9510565162951535312, 1.000000000000000000, 0.9510565162951535312, 1.000000000000000000, 0.9510565162951535312, 1.000000000000000000, 0.9510565162951535312, 1.000000000000000000, 0.9510565162951535312, 1.000000000000000000, 0.9510565162951535312, 1.000000000000000000, 0.9510565162951535312, 1.000000000000000000, 0.9510565162951535312, 1.000000000000000000, 0.9510565162951535312, 1.000000000000000000, 0.9510565162951535312, 1.000000000000000000, 0.9510565162951535312, 1.000000000000000000, 0.9510565162951535312, 1.000000000000000000, 0.9510565162951535312, 1.000000000000000000, 0.9510565162951535312, 1.000000000000000000, 0.9510565162951535312, 1.000000000000000000, 0.9510565162951535312, 1.000000000000000000, 0.9510565162951535312, 1.000000000000000000, 0.9510565162951535312, 1.000000000000000000, 0.9510565162951535312, 1.000000000000000000, 0.9510565162951535312, 1.000000000000000000, 0.9510565162951535312, 1.000000000000000000, 0.9510565162951535312, 1.000000000000000000, 0.9510565162951535312, 1.000000000000000000, 0.9510565162951535312, 1.000000000000000000, 0.9510565162951535312, 1.000000000000000000, 0.9510565162951535312, 1.000000000000000000, 0.9510565162951535312, 1.000000000000000000, 0.9510565162951535312, 1.000000000000000000, 0.9510565162951535312, 1.000000000000000000, 0.9510565162951535312, 1.000000000000000000, 0.9510565162951535312, 1.000000000000000000, 0.9510565162951535312, 1.000000000000000000, 0.9510565162951535312, 1.000000000000000000, 0.9510565162951535312, 1.000000000000000000, 0.9510565162951535312, 1.000000000000000000, 0.9510565162951535312, 1.000000000000000000, 0.9510565162951535312, 1.000000000000000000, 0.9510565162951535312, 1.000000000000000000, 0.9510565162951535312, 1.000000000000000000, 0.9510565162951535312, 1.000000000000000000, 0.9510565162951535312, 1.000000000000000000, 0.9510565162951535312, 1.000000000000000000, 0.9510565162951535312, 1.000000000000000000, 0.9510565162951535312, 1.000000000000000000, 0.9510565162951535312, 1.000000000000000000, 0.9510565162951535312, 1.000000000000000000, 0.9510565162951535312, 1.000000000000000000, 0.9510565162951535312, 1.000000000000000000, 0.9510565162951535312, 1.000000000000000000, 0.9510565162951535312, 1.000000000000000000, 0.9510565162951535312, 1.000000000000000000, 0.9510565162951535312, 1.000000000000000000, 0.9510565162951535312, 1.000000000000000000, 0.9510565162951535312, 1.000000000000000000, 0.9510565162951535312, 1.000000000000000000, 0.9510565162951535312, 1.000000000000000000, 0.9510565162951535312, 1.000000000000000000, 0.9510565162951535312, 1.000000000000000000, 0.9510565162951535312, 1.000000000000000000, 0.9510565162951535312, 1.000000000000000000, 0.9510565162951535312, 1.000000000000000000, 0.9510565162951535312, 1.000000000000000000, 0.9510565162951535312, 1.000000000000000000, 0.9510565162951535312, 1.000000000000000000, 0.9510565162951535312, 1.000000000000000000, 0.9510565162951535312, 1.000000000000000000, 0.9510565162951535312, 1.000000000000000000, 0.9510565162951535312, 1.000000000000000000, 0.9510565162951535312, 1.000000000000000000, 0.9510565162951535312, 1.000000000000000000, 0.9510565162951535312, 1.000000000000000000, 0.9510565162951535312, 1.000000000000000000, 0.9510565162951535312, 1.000000000000000000, 0.9510565162951535312, 1.000000000000000000, 0.9510565162951535312, 1.000000000000000000, 0.9510565162951535312, 1.000000000000000000, 0.9510565162951535312, 1.000000000000000000, 0.9510565162951535312, 1.000000000000000000, 0.9510565162951535312, 1.000000000000000000, 0.9510565162951535312, 1.000000000000000000, 0.9510565162951535312, 1.000000000000000000, 0.9510565162951535312, 1.000000000000000000, 0.9510565162951535312, 1.000000000000000000, 0.9510565162951535312, 1.000000000000000000, 0.9510565162951535312, 1.000000000000000000, 0.9510565162951535312, 1.000000000000000000, 0.9510565162951535312, 1.000000000000000000, 0.9510565162951535312, 1.000000000000000000, 0.9510565162951535312, 1.000000000000000000, 0.9510565162951535312, 1.000000000000000000, 0.9510565162951535312, 1.000000000000000000, 0.9510565162951535312, 1.000000000000000000, 0.9510565162951535312, 1.000000000000000000, 0.9510565162951535312, 1.000000000000000000, 0.9510565162951535312, 1.000000000000000000, 0.9510565162951535312, 1.000000000000000000, 0.9510565162951535312, 1.000000000000000000, 0.9510565162951535312, 1.000000000000000000, 0.9510565162951535312, 1.000000000000000000, 0.9510565162951535312, 1.000000000000000000, 0.9510565162951535312, 1.000000000000000000, 0.9510565162951535312, 1.000000000000000000, 0.9510565162951535312, 1.000000000000000000, 0.9510565162951535312, 1.000000000000000000, 0.9510565162951535312, 1.000000000000000000, 0.9510565162951535312, 1.000000000000000000, 0.9510565162951535312, 1.000000000000000000, 0.9510565162951535312, 1.000000000000000000, 0.9510565162951535312, 1.000000000000000000, 0.9510565162951535312, 1.000000000000000000, 0.9510565162951535312, 1.000000000000000000, 0.9510565162951535312, 1.000000000000000000, 0.9510565162951535312, 1.000000000000000000, 0.9510565162951535312, 1.000000000000000000, 0.9510565162951535312, 1.000000000000000000, 0.9510565162951535312, 1.000000000000000000, 0.9510565162951535312, 1.000000000000000000, 0.9510565162951535312, 1.000000000000000000, 0.9510565162951535312, 1.000000000000000000, 0.9510565162951535312, 1.000000000000000000, 0.9510565162951535312, 1.000000000000000000, 0.9510565162951535312, 1.000000000000000000, 0.9510565162951535312, 1.000000000000000000, 0.9510565162951535312, 1.000000000000000000, 0.9510565162951535312, 1.000000000000000000, 0.9510565162951535312, 1.000000000000000000, 0.9510565162951535312, 1.000000000000000000, 0.9510565162951535312, 1.000000000000000000, 0.9510565162951535312, 1.000000000000000000, 0.9510565162951535312, 1.000000000000000000, 0.9510565162951535312, 1.000000000000000000, 0.9510565162951535312, 1.000000000000000000, 0.9510565162951535312, 1.000000000000000000, 0.9510565162951535312, 1.000000000000000000, 0.9510565162951535312, 1.000000000000000000, 0.9510565162951535312, 1.000000000000000000, 0.9510565162951535312, 1.000000000000000000, 0.9510565162951535312, 1.000000000000000000, 0.9510565162951535312, 1.000000000000000000, 0.9510565162951535312, 1.000000000000000000, 0.9510565162951535312, 1.000000000000000000, 0.9510565162951535312, 1.000000000000000000, 0.9510565162951535312, 1.000000000000000000, 0.9510565162951535312, 1.000000000000000000, 0.9510565162951535312, 1.000000000000000000, 0.9510565162951535312, 1.000000000000000000, 0.9510565162951535312, 1.000000000000000000, 0.9510565162951535312, 1.000000000000000000, 0.9510565162951535312, 1.000000000000000000, 0.9510565162951535312, 1.000000000000000000, 0.9510565162951535312, 1.000000000000000000, 0.9510565162951535312, 1.000000000000000000, 0.9510565162951535312, 1.000000000000000000, 0.9510565162951535312, 1.000000000000000000, 0.9510565162951535312, 1.000000000000000000, 0.9510565162951535312, 1.000000000000000000, 1.000000000000000000, 1.000000000000000000 ) ) 
 REPRESENTATION_ITEM ( '' )  );
#10905 = CARTESIAN_POINT ( 'NONE',  ( -10.00000000000000711, 207.0476921513413515, 39.50113791807856956 ) ) ;
#10906 = CARTESIAN_POINT ( 'NONE',  ( 87.07499999726880446, 141.7447067706911810, -9.630534252274385310 ) ) ;
#10907 = APPLICATION_PROTOCOL_DEFINITION ( 'draft international standard', 'automotive_design', 1998, #31172 ) ;
#10908 = CARTESIAN_POINT ( 'NONE',  ( 6.444103211790928043, 211.7408657792734061, 90.69886208192143329 ) ) ;
#10909 = CARTESIAN_POINT ( 'NONE',  ( 40.82499999726880446, 141.7447067706911810, -9.630534252274385310 ) ) ;
#10910 = PLANE ( 'NONE',  #13827 ) ;
#10911 = CARTESIAN_POINT ( 'NONE',  ( -98.16666666666678509, -61.33333333333321491, -13.66666666666659502 ) ) ;
#10912 = CARTESIAN_POINT ( 'NONE',  ( -0.05014649552807705357, 194.3824533091408000, 5.751137918078564226 ) ) ;
#10913 = CARTESIAN_POINT ( 'NONE',  ( 6.439685834477092641, -4.942299687812566233, -7.659344964963564983 ) ) ;
#10914 = CARTESIAN_POINT ( 'NONE',  ( 54.97499999726881015, 140.1801316387863778, -4.815267126137194431 ) ) ;
#10915 = CARTESIAN_POINT ( 'NONE',  ( -10.00000000000000711, 207.0476921513413515, 57.50113791807856956 ) ) ;
#10916 = CARTESIAN_POINT ( 'NONE',  ( 9.984503880673473830, 203.7031108863295401, 29.15113791807856458 ) ) ;
#10917 = DIRECTION ( 'NONE',  ( 0.000000000000000000, -1.000000000000000000, 9.859324684083082301E-16 ) ) ;
#10918 = CARTESIAN_POINT ( 'NONE',  ( 55.18867513459483121, 169.2658477444273331, -4.635254915624224203 ) ) ;
#10919 = DIRECTION ( 'NONE',  ( 0.000000000000000000, -1.000000000000000000, 1.100686371591861952E-15 ) ) ;
#10920 = VECTOR ( 'NONE', #27059, 1000.000000000000000 ) ;
#10921 = CARTESIAN_POINT ( 'NONE',  ( 59.89999999453763024, 150.2886644046228639, -14.50000000000000888 ) ) ;
#10922 = VERTEX_POINT ( 'NONE', #21402 ) ;
#10923 = CARTESIAN_POINT ( 'NONE',  ( 9.680171189290831535, 199.9079932115568852, 38.30113791807856671 ) ) ;
#10924 = DIRECTION ( 'NONE',  ( -0.5526942671207061286, -0.1536855300543007730, -0.8190908404712107238 ) ) ;
#10925 = EDGE_CURVE ( 'NONE', #22734, #31784, #32179, .T. ) ;
#10926 = CARTESIAN_POINT ( 'NONE',  ( -3.044812012439970683, 197.4746971517856196, 25.89886208192143613 ) ) ;
#10927 = DIRECTION ( 'NONE',  ( -1.000000000000000000, 0.000000000000000000, -0.000000000000000000 ) ) ;
#10928 = ORIENTED_EDGE ( 'NONE', *, *, #30829, .F. ) ;
#10929 = CARTESIAN_POINT ( 'NONE',  ( 0.05014649552810505201, 217.5146222423826714, 82.25113791807858377 ) ) ;
#10930 = ORIENTED_EDGE ( 'NONE', *, *, #5398, .T. ) ;
#10931 = CARTESIAN_POINT ( 'NONE',  ( 50.21132485994281325, 170.7719333635740497, -7.904646289410545231E-15 ) ) ;
#10932 = DIRECTION ( 'NONE',  ( 0.000000000000000000, 0.000000000000000000, 1.000000000000000000 ) ) ;
#10933 = ORIENTED_EDGE ( 'NONE', *, *, #20771, .T. ) ;
#10934 = CARTESIAN_POINT ( 'NONE',  ( -4.984841277089726574, 200.2242689037092305, 15.05113791807856849 ) ) ;
#10935 = DIRECTION ( 'NONE',  ( 0.000000000000000000, 0.000000000000000000, -1.000000000000000000 ) ) ;
#10936 = CARTESIAN_POINT ( 'NONE',  ( -7.375838497908014268, 196.7627149292498530, 101.0488620819214276 ) ) ;
#10937 = CARTESIAN_POINT ( 'NONE',  ( 46.57499999726881157, 145.8408176439707802, 12.60653300113718345 ) ) ;
#10938 = ORIENTED_EDGE ( 'NONE', *, *, #16594, .F. ) ;
#10939 = CARTESIAN_POINT ( 'NONE',  ( 49.42499999726879878, 168.2552932293087906, -9.630534252274385310 ) ) ;
#10940 = LINE ( 'NONE', #23876, #16445 ) ;
#10941 = CARTESIAN_POINT ( 'NONE',  ( -125.0000000000000000, 0.000000000000000000, -20.00000000000000000 ) ) ;
#10942 = CIRCLE ( 'NONE', #16365, 27.99999999999999645 ) ;
#10943 = CARTESIAN_POINT ( 'NONE',  ( -6.139770520408224463, 198.4640165459539389, 83.04886208192144181 ) ) ;
#10944 = CARTESIAN_POINT ( 'NONE',  ( 56.57499999726881157, 145.8408176439707802, 12.60653300113718345 ) ) ;
#10945 = CARTESIAN_POINT ( 'NONE',  ( 3.044812012440130555, 197.4746971517856764, 20.60113791807856742 ) ) ;
#10946 = DIRECTION ( 'NONE',  ( 0.000000000000000000, 0.7071067811865330288, -0.7071067811865621167 ) ) ;
#10947 = CARTESIAN_POINT ( 'NONE',  ( 72.90000000000000568, 168.7903194862797420, -4.480746418436745593 ) ) ;
#10948 = CARTESIAN_POINT ( 'NONE',  ( 99.30625411593993590, 155.0000000000000000, -12.00000000000001066 ) ) ;
#10949 = LINE ( 'NONE', #19110, #21308 ) ;
#10950 = CARTESIAN_POINT ( 'NONE',  ( 9.984503880673470277, 203.7031108863295401, 83.15113791807853261 ) ) ;
#10951 = CARTESIAN_POINT ( 'NONE',  ( 33.18867513459482410, 169.2658477444273331, -4.635254915624224203 ) ) ;
#10952 = CARTESIAN_POINT ( 'NONE',  ( 39.17499999726881299, 145.8408176439707802, -12.60653300113719588 ) ) ;
#10953 = CARTESIAN_POINT ( 'NONE',  ( -9.736236675708031640, 214.0148392665760753, 98.79886208192142760 ) ) ;
#10954 = CARTESIAN_POINT ( 'NONE',  ( 75.02499999726879309, 149.9369285172503510, -15.58253175000000823 ) ) ;
#10955 = ORIENTED_EDGE ( 'NONE', *, *, #33130, .F. ) ;
#10956 = CARTESIAN_POINT ( 'NONE',  ( 48.31132485994280756, 169.2658477444273331, 4.635254915624208216 ) ) ;
#10957 = CARTESIAN_POINT ( 'NONE',  ( 43.29999999453762172, 142.6655632788954620, 8.961492836873471646 ) ) ;
#10958 =( BOUNDED_CURVE ( )  B_SPLINE_CURVE ( 2, ( #836, #21451, #8345, #23837, #29286, #19060, #11225, #3554, #5767, #16161, #29450 ),
 .UNSPECIFIED., .F., .T. ) 
 B_SPLINE_CURVE_WITH_KNOTS ( ( 3, 2, 2, 2, 2, 3 ),
 ( 0.07142857142857124420, 0.07499999999999981681, 0.07857142857142838943, 0.08214285714285696205, 0.08571428571428553467, 0.08928571428571410729 ),
 .UNSPECIFIED. ) 
 CURVE ( )  GEOMETRIC_REPRESENTATION_ITEM ( )  RATIONAL_B_SPLINE_CURVE ( ( 1.000000000000002220, 0.9510565162951514218, 1.000000000000000000, 0.9510565162951534202, 1.000000000000000000, 0.9510565162951534202, 1.000000000000000000, 0.9510565162951534202, 1.000000000000000000, 0.9510565162951545304, 0.9999999999999988898 ) ) 
 REPRESENTATION_ITEM ( '' )  );
#10959 = CARTESIAN_POINT ( 'NONE',  ( 74.78867513459483973, 155.0000000000000000, -15.00000000000002487 ) ) ;
#10960 = EDGE_CURVE ( 'NONE', #19681, #7672, #27260, .T. ) ;
#10961 = CARTESIAN_POINT ( 'NONE',  ( 3.500000000000004885, -1.355464348821720177, -0.1381584212714541127 ) ) ;
#10962 = ORIENTED_EDGE ( 'NONE', *, *, #9936, .F. ) ;
#10963 = CARTESIAN_POINT ( 'NONE',  ( 3.135527875058981895, 197.5041725223112792, 97.59886208192143897 ) ) ;
#10964 = CARTESIAN_POINT ( 'NONE',  ( -3.662846001189865142, 195.5725841191952838, 28.89886208192143613 ) ) ;
#10965 = FACE_OUTER_BOUND ( 'NONE', #20645, .T. ) ;
#10966 = CARTESIAN_POINT ( 'NONE',  ( -10.00000000000000711, 207.0476921513413515, 48.50113791807856956 ) ) ;
#10967 = ORIENTED_EDGE ( 'NONE', *, *, #17958, .F. ) ;
#10968 = CARTESIAN_POINT ( 'NONE',  ( -10.10169002831358576, 228.2744804605295315, 105.4832055762869061 ) ) ;
#10969 = EDGE_CURVE ( 'NONE', #32873, #17505, #12113, .T. ) ;
#10970 = FACE_OUTER_BOUND ( 'NONE', #1122, .T. ) ;
#10971 = EDGE_LOOP ( 'NONE', ( #2054, #15401 ) ) ;
#10972 = CARTESIAN_POINT ( 'NONE',  ( -6.500168698208244500, 211.6636982574061676, 86.79886208192142760 ) ) ;
#10973 = CARTESIAN_POINT ( 'NONE',  ( 2.517493886308900919, 214.5937144450984420, 28.40113791807856813 ) ) ;
#10974 = CARTESIAN_POINT ( 'NONE',  ( 3.500000000000004885, -0.3414694520252361531, -2.899999999999997247 ) ) ;
#10975 = EDGE_LOOP ( 'NONE', ( #79, #686, #32246, #12680, #4091, #19254 ) ) ;
#10976 = CARTESIAN_POINT ( 'NONE',  ( 34.72499999726881015, 140.1801316387863778, -4.815267126137194431 ) ) ;
#10977 = CARTESIAN_POINT ( 'NONE',  ( 87.32499999726880446, 164.1591823560292198, -12.60653300113719766 ) ) ;
#10978 = DIRECTION ( 'NONE',  ( -1.000000000000000000, 0.000000000000000000, 0.000000000000000000 ) ) ;
#10979 = CARTESIAN_POINT ( 'NONE',  ( -2.426778023690262742, 214.6231898156240163, 94.10113791807857808 ) ) ;
#10980 = CIRCLE ( 'NONE', #30023, 2.500000000000000000 ) ;
#10981 = CARTESIAN_POINT ( 'NONE',  ( 0.000000000000000000, 0.000000000000000000, 0.000000000000000000 ) ) ;
#10982 = CARTESIAN_POINT ( 'NONE',  ( 55.90000000000000568, 141.2096805137202580, 4.480746418436733158 ) ) ;
#10983 = CARTESIAN_POINT ( 'NONE',  ( 7.984503880673422316, 209.6470497212048372, 72.84886208192143897 ) ) ;
#10984 = DIRECTION ( 'NONE',  ( 0.000000000000000000, -0.7071067811865411334, 0.7071067811865540120 ) ) ;
#10985 = EDGE_CURVE ( 'NONE', #33564, #10532, #30645, .T. ) ;
#10986 = CARTESIAN_POINT ( 'NONE',  ( 60.32499999726881157, 145.8408176439707802, 12.60653300113718345 ) ) ;
#10987 = CARTESIAN_POINT ( 'NONE',  ( 10.00000000000000711, 206.9523078486586201, 11.00113791807856600 ) ) ;
#10988 = CARTESIAN_POINT ( 'NONE',  ( 111.1125082318798007, 155.0000000000000000, -32.00000000000002842 ) ) ;
#10989 = CONICAL_SURFACE ( 'NONE', #3366, 6.500000000000000888, 0.8987552595851582282 ) ;
#10990 = CARTESIAN_POINT ( 'NONE',  ( 63.62499999726879452, 171.3844434931184253, -7.942151717890134290E-15 ) ) ;
#10991 = CARTESIAN_POINT ( 'NONE',  ( 79.07499999726880446, 141.7447067706911810, -9.630534252274385310 ) ) ;
#10992 = CARTESIAN_POINT ( 'NONE',  ( 7.375838497908181246, 196.7627149292499666, 74.45113791807855819 ) ) ;
#10993 = CARTESIAN_POINT ( 'NONE',  ( 48.81132485994281467, 150.1262045565064227, 15.00000000000001599 ) ) ;
#10994 = CARTESIAN_POINT ( 'NONE',  ( 0.05014649552810506589, 217.5146222423826714, 97.25113791807855534 ) ) ;
#10995 = EDGE_CURVE ( 'NONE', #12934, #9032, #16492, .T. ) ;
#10996 = CARTESIAN_POINT ( 'NONE',  ( 103.3032345859876102, 155.0000000000000000, 0.000000000000000000 ) ) ;
#10997 = ORIENTED_EDGE ( 'NONE', *, *, #19350, .F. ) ;
#10998 = CARTESIAN_POINT ( 'NONE',  ( -7.375838497908014268, 196.7627149292498530, 59.04886208192144181 ) ) ;
#10999 = CARTESIAN_POINT ( 'NONE',  ( -0.05014649552828402690, 217.5146222423826714, 63.24886208192144466 ) ) ;
#11000 = CARTESIAN_POINT ( 'NONE',  ( -11.98450388067341876, 203.0532714938636047, 2.348862081921434530 ) ) ;
#11001 = LINE ( 'NONE', #5874, #4498 ) ;
#11002 = CARTESIAN_POINT ( 'NONE',  ( 10.00000000000000711, 206.9523078486586201, 11.00113791807856600 ) ) ;
#11003 = CARTESIAN_POINT ( 'NONE',  ( 10.00000000000000711, 207.0476921513415220, 78.99886208192144466 ) ) ;
#11004 = EDGE_LOOP ( 'NONE', ( #1862, #28090, #68, #31998 ) ) ;
#11005 = ADVANCED_FACE ( 'NONE', ( #19985 ), #1258, .T. ) ;
#11006 = MECHANICAL_DESIGN_GEOMETRIC_PRESENTATION_REPRESENTATION (  '', ( #25276 ), #7835 ) ;
#11007 = CARTESIAN_POINT ( 'NONE',  ( 3.250000000000003109, -5.629165124598849879, 0.000000000000000000 ) ) ;
#11008 = VERTEX_POINT ( 'NONE', #25607 ) ;
#11009 = FILL_AREA_STYLE ('',( #10852 ) ) ;
#11010 = CARTESIAN_POINT ( 'NONE',  ( 6.444103211790928043, 211.7408657792734061, 63.69886208192144039 ) ) ;
#11011 = B_SPLINE_CURVE_WITH_KNOTS ( 'NONE', 3,
 ( #33578, #2578, #15845, #26234, #10257, #28469 ),
 .UNSPECIFIED., .F., .F.,
 ( 4, 2, 4 ),
 ( 2.380727409112127398E-07, 0.008032766472079759176, 0.01606529487141860474 ),
 .UNSPECIFIED. ) ;
#11012 = VERTEX_POINT ( 'NONE', #12152 ) ;
#11013 = CARTESIAN_POINT ( 'NONE',  ( 77.52499999726880731, 169.8198683612136222, -4.815267126137197984 ) ) ;
#11014 = EDGE_LOOP ( 'NONE', ( #26751, #21186, #8759, #32483 ) ) ;
#11015 = CARTESIAN_POINT ( 'NONE',  ( 2.000000000000000000, -0.8865213383406685965, 1.535500000000000531 ) ) ;
#11016 = CARTESIAN_POINT ( 'NONE',  ( 87.50000000000001421, 155.0000000000000000, -6.938893903907228378E-15 ) ) ;
#11017 = CONICAL_SURFACE ( 'NONE', #22980, 32.00000000000002842, 1.466076571675243523 ) ;
#11018 = UNCERTAINTY_MEASURE_WITH_UNIT (LENGTH_MEASURE( 1.000000000000000082E-05 ), #11061, 'distance_accuracy_value', 'NONE');
#11019 = CARTESIAN_POINT ( 'NONE',  ( 72.22499999726881015, 149.9369285172503510, 15.58253174999999580 ) ) ;
#11020 = EDGE_CURVE ( 'NONE', #16522, #15028, #9771, .T. ) ;
#11021 = CARTESIAN_POINT ( 'NONE',  ( -6.444103211791042618, 211.7408657792732356, 72.80113791807858092 ) ) ;
#11022 = CARTESIAN_POINT ( 'NONE',  ( -3.499999999999997780, -2.020725942163714262, -2.587392608830344720 ) ) ;
#11023 = SHAPE_REPRESENTATION_RELATIONSHIP ( 'NONE' , 'NONE' ,  #16299, #13278 ) ;
#11024 = CARTESIAN_POINT ( 'NONE',  ( 35.00000000000000000, 170.2462022514548323, -7.872454543227099337E-15 ) ) ;
#11025 = CARTESIAN_POINT ( 'NONE',  ( 4.903702542908435547, 213.8346818373419751, 48.54886208192144181 ) ) ;
#11026 = CARTESIAN_POINT ( 'NONE',  ( 8.062137200540920645, 201.0835637161417822, 80.30113791807858092 ) ) ;
#11027 = CARTESIAN_POINT ( 'NONE',  ( 3.135527875058820690, 216.4958274776887492, 64.40113791807857524 ) ) ;
#11028 = PRODUCT_DEFINITION_FORMATION_WITH_SPECIFIED_SOURCE ( 'ANY', '', #1532, .NOT_KNOWN. ) ;
#11029 = CARTESIAN_POINT ( 'NONE',  ( -66.50402289005056389, 121.5305141831588003, -17.99597710994943967 ) ) ;
#11030 = CARTESIAN_POINT ( 'NONE',  ( -4.903702542908602524, 213.8346818373418898, 21.95113791807856884 ) ) ;
#11031 = CARTESIAN_POINT ( 'NONE',  ( 72.71132485994280614, 155.0000000000000000, 15.00000000000001243 ) ) ;
#11032 = CARTESIAN_POINT ( 'NONE',  ( -6.878751942472531411, 3.924677726130923361, -6.573129608219089981 ) ) ;
#11033 = CARTESIAN_POINT ( 'NONE',  ( 45.82499999726881157, 168.2552932293087906, 9.630534252274372875 ) ) ;
#11034 = CARTESIAN_POINT ( 'NONE',  ( -0.05014649552807705357, 194.3824533091408000, 44.75113791807856956 ) ) ;
#11035 = LINE ( 'NONE', #31488, #3728 ) ;
#11036 = CARTESIAN_POINT ( 'NONE',  ( 8.118202686958039038, 212.8392687619912635, 94.70113791807857240 ) ) ;
#11037 = CARTESIAN_POINT ( 'NONE',  ( 3.044812012440130555, 197.4746971517856764, 65.60113791807857808 ) ) ;
#11038 = CARTESIAN_POINT ( 'NONE',  ( 3.753561863808876797, 195.6020594897209719, 37.59886208192143187 ) ) ;
#11039 = CARTESIAN_POINT ( 'NONE',  ( 6.220909254589680693, 198.5229672870052582, 40.44886208192143329 ) ) ;
#11040 = CARTESIAN_POINT ( 'NONE',  ( 80.69999999453764872, 167.3344367211045096, 8.961492836873468093 ) ) ;
#11041 = VECTOR ( 'NONE', #32802, 1000.000000000000000 ) ;
#11042 = CARTESIAN_POINT ( 'NONE',  ( 9.736236675707914401, 214.0148392665762458, 79.70113791807857240 ) ) ;
#11043 = CARTESIAN_POINT ( 'NONE',  ( -2.517493886308901807, 199.4062855549015012, 86.90113791807857524 ) ) ;
#11044 = AXIS2_PLACEMENT_3D ( 'NONE', #22230, #779, #19007 ) ;
#11045 = CARTESIAN_POINT ( 'NONE',  ( 10.01549611932659545, 203.7984951890123853, 52.14886208192142192 ) ) ;
#11046 = CARTESIAN_POINT ( 'NONE',  ( 2.385244779468109755E-15, 4.041451884327391220, -2.587392608830344720 ) ) ;
#11047 = ORIENTED_EDGE ( 'NONE', *, *, #11642, .F. ) ;
#11048 = CARTESIAN_POINT ( 'NONE',  ( -3.753561863808878130, 218.3979405102790281, 66.09886208192142476 ) ) ;
#11049 = B_SPLINE_CURVE_WITH_KNOTS ( 'NONE', 3,
 ( #15801, #23475, #23643, #303, #31484, #8151, #474, #7476, #24135, #27195, #10871, #21412, #3517, #6415, #29250, #19192, #14243, #11192 ),
 .UNSPECIFIED., .F., .F.,
 ( 4, 2, 2, 2, 2, 2, 2, 2, 4 ),
 ( 0.5000000000000000000, 0.5624999999999993339, 0.6249999999999986677, 0.6874999999999981126, 0.7499999999999974465, 0.8124999999999980016, 0.8749999999999986677, 0.9374999999999993339, 1.000000000000000000 ),
 .UNSPECIFIED. ) ;
#11050 = ORIENTED_EDGE ( 'NONE', *, *, #25161, .F. ) ;
#11051 = CARTESIAN_POINT ( 'NONE',  ( -4.984841277089891776, 213.7757310962905990, 32.94886208192144039 ) ) ;
#11052 = ORIENTED_EDGE ( 'NONE', *, *, #18559, .F. ) ;
#11053 = EDGE_CURVE ( 'NONE', #210, #17299, #15943, .T. ) ;
#11054 = EDGE_CURVE ( 'NONE', #18759, #12567, #28775, .T. ) ;
#11055 = CARTESIAN_POINT ( 'NONE',  ( 75.07499999726880446, 141.7447067706911810, -9.630534252274387086 ) ) ;
#11056 = CARTESIAN_POINT ( 'NONE',  ( 53.21132485994280614, 139.2280666364260071, -4.041636747397287284E-15 ) ) ;
#11057 = VECTOR ( 'NONE', #13458, 1000.000000000000000 ) ;
#11058 = PLANE ( 'NONE',  #7871 ) ;
#11059 = CARTESIAN_POINT ( 'NONE',  ( 2.426778023690261410, 199.3768101843759837, 50.60113791807857808 ) ) ;
#11060 = EDGE_CURVE ( 'NONE', #14849, #23405, #21919, .T. ) ;
#11061 =( LENGTH_UNIT ( ) NAMED_UNIT ( * ) SI_UNIT ( .MILLI., .METRE. ) );
#11062 = CARTESIAN_POINT ( 'NONE',  ( 10.00000000000000711, 207.0476921513415220, 30.99886208192143755 ) ) ;
#11063 = CARTESIAN_POINT ( 'NONE',  ( 72.27499999726880731, 160.0630714827496206, 15.58253174999999224 ) ) ;
#11064 = ORIENTED_EDGE ( 'NONE', *, *, #6797, .T. ) ;
#11065 = DIRECTION ( 'NONE',  ( 0.000000000000000000, 0.000000000000000000, 1.000000000000000000 ) ) ;
#11066 = AXIS2_PLACEMENT_3D ( 'NONE', #3932, #6317, #14330 ) ;
#11067 = CARTESIAN_POINT ( 'NONE',  ( -4.903702542908436435, 200.1653181626580249, 14.04886208192143471 ) ) ;
#11068 = AXIS2_PLACEMENT_3D ( 'NONE', #30028, #4643, #28151 ) ;
#11069 = CARTESIAN_POINT ( 'NONE',  ( -6.139770520408369237, 215.5359834540460042, 48.95113791807855108 ) ) ;
#11070 = CARTESIAN_POINT ( 'NONE',  ( 1.305263714129178743, -8.377797850839291627, -7.792447862505339273 ) ) ;
#11071 = CARTESIAN_POINT ( 'NONE',  ( 3.135527875058820690, 216.4958274776887492, 34.40113791807856813 ) ) ;
#11072 = CARTESIAN_POINT ( 'NONE',  ( 87.67499999726882720, 168.2552932293087906, -9.630534252274385310 ) ) ;
#11073 = CIRCLE ( 'NONE', #8348, 2.149999999999999023 ) ;
#11074 = APPLICATION_PROTOCOL_DEFINITION ( 'draft international standard', 'automotive_design', 1998, #24200 ) ;
#11075 = CARTESIAN_POINT ( 'NONE',  ( 6.444103211790928043, 211.7408657792734061, 87.69886208192144750 ) ) ;
#11076 = CARTESIAN_POINT ( 'NONE',  ( 36.22499999726881015, 149.9369285172503510, 15.58253174999999580 ) ) ;
#11077 = CARTESIAN_POINT ( 'NONE',  ( 67.50000000000000000, 155.0000000000000000, -7.500000000000022204 ) ) ;
#11078 = CARTESIAN_POINT ( 'NONE',  ( 110.1179863365115636, 155.0000000000000000, 0.000000000000000000 ) ) ;
#11079 = CARTESIAN_POINT ( 'NONE',  ( 11.98450388067348271, 203.0532714938637753, 23.15113791807856458 ) ) ;
#11080 = DIRECTION ( 'NONE',  ( 0.000000000000000000, 0.000000000000000000, -1.000000000000000000 ) ) ;
#11081 = CARTESIAN_POINT ( 'NONE',  ( 59.27499999726882152, 149.9369285172503510, -15.58253175000000823 ) ) ;
#11082 = CARTESIAN_POINT ( 'NONE',  ( -8.118202686958039038, 201.1607312380087080, 69.20113791807858661 ) ) ;
#11083 = CARTESIAN_POINT ( 'NONE',  ( 8.062137200540920645, 201.0835637161417822, 38.30113791807857382 ) ) ;
#11084 = DIRECTION ( 'NONE',  ( 0.000000000000000000, 0.000000000000000000, -1.000000000000000000 ) ) ;
#11085 = CIRCLE ( 'NONE', #22479, 3.499999999999996003 ) ;
#11086 = CARTESIAN_POINT ( 'NONE',  ( 5.000000000000000000, -2.342598717236903383, 4.057500000000001883 ) ) ;
#11087 = CARTESIAN_POINT ( 'NONE',  ( 6.220909254589680693, 198.5229672870052582, 10.44886208192143506 ) ) ;
#11088 = CARTESIAN_POINT ( 'NONE',  ( 62.19999999453763451, 163.5228861582408797, -11.73074641843674470 ) ) ;
#11089 = VERTEX_POINT ( 'NONE', #20153 ) ;
#11090 = CARTESIAN_POINT ( 'NONE',  ( 12.00000000000000711, 206.9523078486586485, 44.00113791807856956 ) ) ;
#11091 = CARTESIAN_POINT ( 'NONE',  ( 32.50000000000000000, 155.0000000000000000, -6.938893903907228378E-15 ) ) ;
#11092 = CARTESIAN_POINT ( 'NONE',  ( 3.044812012439969795, 216.5253028482143520, 18.39886208192143613 ) ) ;
#11093 = CARTESIAN_POINT ( 'NONE',  ( 70.88867513459481984, 159.8737954434938047, -14.99999999999988454 ) ) ;
#11094 = ORIENTED_EDGE ( 'NONE', *, *, #6628, .T. ) ;
#11095 = CARTESIAN_POINT ( 'NONE',  ( 3.044812012440130555, 197.4746971517856764, 77.60113791807857808 ) ) ;
#11096 = CIRCLE ( 'NONE', #1313, 5.200000000000002842 ) ;
#11097 = EDGE_LOOP ( 'NONE', ( #21265, #12398, #23330, #13643 ) ) ;
#11098 = VECTOR ( 'NONE', #4635, 1000.000000000000000 ) ;
#11099 = CARTESIAN_POINT ( 'NONE',  ( 50.41132485994280898, 167.7597621252805880, 9.270509831248428867 ) ) ;
#11100 = CARTESIAN_POINT ( 'NONE',  ( -5.619193549420757883, -4.261310591078458110, -5.875704392893551287 ) ) ;
#11101 = ORIENTED_EDGE ( 'NONE', *, *, #8289, .T. ) ;
#11102 = CARTESIAN_POINT ( 'NONE',  ( -7.984503880673488041, 209.6470497212046098, 18.65113791807856458 ) ) ;
#11103 =( BOUNDED_CURVE ( )  B_SPLINE_CURVE ( 2, ( #16932, #25282, #30403, #22732, #4672, #6722, #27328, #3992, #1436, #14389, #24611 ),
 .UNSPECIFIED., .F., .T. ) 
 B_SPLINE_CURVE_WITH_KNOTS ( ( 3, 2, 2, 2, 2, 3 ),
 ( 0.2678571428571425717, 0.2714285714285711304, 0.2749999999999996891, 0.2785714285714281924, 0.2821428571428568621, 0.2857142857142854209 ),
 .UNSPECIFIED. ) 
 CURVE ( )  GEOMETRIC_REPRESENTATION_ITEM ( )  RATIONAL_B_SPLINE_CURVE ( ( 1.000000000000003109, 0.9510565162951504226, 1.000000000000000000, 0.9510565162951534202, 1.000000000000000000, 0.9510565162951534202, 1.000000000000000000, 0.9510565162951534202, 1.000000000000000000, 0.9510565162951571949, 0.9999999999999962252 ) ) 
 REPRESENTATION_ITEM ( '' )  );
#11104 = CARTESIAN_POINT ( 'NONE',  ( -59.60884549136632415, 194.9369081818307166, 2.246623501397673639 ) ) ;
#11105 = CARTESIAN_POINT ( 'NONE',  ( -10.00000000000000711, 206.9523078486584495, 8.498862081921433997 ) ) ;
#11106 = CARTESIAN_POINT ( 'NONE',  ( 45.57499999726881157, 164.1591823560292198, -12.60653300113719766 ) ) ;
#11107 = VERTEX_POINT ( 'NONE', #30899 ) ;
#11108 = CARTESIAN_POINT ( 'NONE',  ( 51.42499999726879878, 168.2552932293087906, -9.630534252274385310 ) ) ;
#11109 = DIRECTION ( 'NONE',  ( 0.7071067811865454633, -0.000000000000000000, -0.7071067811865495711 ) ) ;
#11110 = PLANE ( 'NONE',  #11262 ) ;
#11111 = AXIS2_PLACEMENT_3D ( 'NONE', #21525, #14027, #8920 ) ;
#11112 = CARTESIAN_POINT ( 'NONE',  ( 4.000000000000000000, -3.518949890710769246, 3.686287386450715076E-15 ) ) ;
#11113 = CARTESIAN_POINT ( 'NONE',  ( -3.135527875058982783, 216.4958274776886924, 78.09886208192143897 ) ) ;
#11114 = CARTESIAN_POINT ( 'NONE',  ( 53.57499999726881157, 164.1591823560292198, -12.60653300113719766 ) ) ;
#11115 = CARTESIAN_POINT ( 'NONE',  ( 10.00000000000000711, 206.9523078486586201, 26.00113791807856956 ) ) ;
#11116 = DIRECTION ( 'NONE',  ( -1.000000000000000000, 0.000000000000000000, 0.000000000000000000 ) ) ;
#11117 = CARTESIAN_POINT ( 'NONE',  ( -3.753561863808878130, 218.3979405102790281, 84.09886208192143897 ) ) ;
#11118 =( GEOMETRIC_REPRESENTATION_CONTEXT ( 3 ) GLOBAL_UNCERTAINTY_ASSIGNED_CONTEXT ( ( #26349 ) ) GLOBAL_UNIT_ASSIGNED_CONTEXT ( ( #32551, #24893, #19946 ) ) REPRESENTATION_CONTEXT ( 'NONE', 'WORKASPACE' ) );
#11119 = CARTESIAN_POINT ( 'NONE',  ( 74.20000000000000284, 142.6655632788954620, -8.961492836873480528 ) ) ;
#11120 = CARTESIAN_POINT ( 'NONE',  ( -7.922281120364393914, -4.573931137438277617, -8.047472243342932430 ) ) ;
#11121 = CARTESIAN_POINT ( 'NONE',  ( -64.50000000000000000, 120.3589838486224579, -20.00000000000000000 ) ) ;
#11122 = CARTESIAN_POINT ( 'NONE',  ( -8.118202686958039038, 201.1607312380087080, 93.20113791807857240 ) ) ;
#11123 = DIRECTION ( 'NONE',  ( -0.000000000000000000, -0.000000000000000000, 1.000000000000000000 ) ) ;
#11124 = AXIS2_PLACEMENT_3D ( 'NONE', #13599, #31664, #8658 ) ;
#11125 = CARTESIAN_POINT ( 'NONE',  ( 35.87499999726881583, 171.3844434931184253, -7.942151717890132712E-15 ) ) ;
#11126 = CARTESIAN_POINT ( 'NONE',  ( -3.044812012440131443, 216.5253028482142952, 34.10113791807857808 ) ) ;
#11127 = CARTESIAN_POINT ( 'NONE',  ( 76.82499999726881867, 141.7447067706911810, -9.630534252274385310 ) ) ;
#11128 = ORIENTED_EDGE ( 'NONE', *, *, #24533, .T. ) ;
#11129 = DIRECTION ( 'NONE',  ( -0.2649168722799616349, 0.9642688156137669830, -0.002168413296787739895 ) ) ;
#11130 = CARTESIAN_POINT ( 'NONE',  ( 42.59999999453763309, 168.7903194862797420, 4.480746418436729606 ) ) ;
#11131 = CARTESIAN_POINT ( 'NONE',  ( -0.05014649552807705357, 194.3824533091408000, 8.751137918078567779 ) ) ;
#11132 = CARTESIAN_POINT ( 'NONE',  ( 8.399999999999998579, 0.000000000000000000, -4.400000000000001243 ) ) ;
#11133 = CARTESIAN_POINT ( 'NONE',  ( 1.249999999999999112, -7.938566201357367902, -7.198902722707431145 ) ) ;
#11134 = VERTEX_POINT ( 'NONE', #7047 ) ;
#11135 =( GEOMETRIC_REPRESENTATION_CONTEXT ( 3 ) GLOBAL_UNCERTAINTY_ASSIGNED_CONTEXT ( ( #13436 ) ) GLOBAL_UNIT_ASSIGNED_CONTEXT ( ( #19726, #6452, #3721 ) ) REPRESENTATION_CONTEXT ( 'NONE', 'WORKASPACE' ) );
#11136 = CARTESIAN_POINT ( 'NONE',  ( -9.984503880673420539, 203.7031108863293980, 92.34886208192142476 ) ) ;
#11137 = CARTESIAN_POINT ( 'NONE',  ( 9.736236675708031640, 199.9851607334238963, 28.29886208192143826 ) ) ;
#11138 = CARTESIAN_POINT ( 'NONE',  ( 95.70416941062676131, 155.0000000000000000, -32.00000000000005684 ) ) ;
#11139 = CARTESIAN_POINT ( 'NONE',  ( 10.00000000000000711, 206.9523078486586201, 53.00113791807857666 ) ) ;
#11140 = VERTEX_POINT ( 'NONE', #27484 ) ;
#11141 = CARTESIAN_POINT ( 'NONE',  ( 8.000000000000008882, 207.0476921513415220, 9.998862081921435774 ) ) ;
#11142 = CARTESIAN_POINT ( 'NONE',  ( 51.01132485994281751, 142.2402378747194405, 9.270509831248432420 ) ) ;
#11143 = ORIENTED_EDGE ( 'NONE', *, *, #31007, .F. ) ;
#11144 = CARTESIAN_POINT ( 'NONE',  ( -8.000000000000008882, 206.9523078486584780, 86.49886208192144466 ) ) ;
#11145 = CARTESIAN_POINT ( 'NONE',  ( 4.984841277089725686, 213.7757310962907411, 34.55113791807856671 ) ) ;
#11146 = CARTESIAN_POINT ( 'NONE',  ( 8.000000000000000000, 6.500000000000000000, 0.000000000000000000 ) ) ;
#11147 = ORIENTED_EDGE ( 'NONE', *, *, #9298, .T. ) ;
#11148 = DIRECTION ( 'NONE',  ( 0.000000000000000000, 0.000000000000000000, -1.000000000000000000 ) ) ;
#11149 = CARTESIAN_POINT ( 'NONE',  ( 36.97499999726881015, 140.1801316387863778, -4.815267126137194431 ) ) ;
#11150 = CARTESIAN_POINT ( 'NONE',  ( -6.500000000000001776, -2.602085213965210642E-15, -5.592027715088707218 ) ) ;
#11151 = CARTESIAN_POINT ( 'NONE',  ( 0.05014649552807626948, 215.4116977939061144, 100.2511379180785696 ) ) ;
#11152 = EDGE_CURVE ( 'NONE', #5826, #13463, #24285, .T. ) ;
#11153 = CARTESIAN_POINT ( 'NONE',  ( 132.3999999999999773, 48.99999999999998579, 7.263162560269298651E-13 ) ) ;
#11154 = CARTESIAN_POINT ( 'NONE',  ( 51.60000000000000853, 150.2886644046228639, 14.49999999999999645 ) ) ;
#11155 = CARTESIAN_POINT ( 'NONE',  ( -6.444103211790928043, 202.2591342207265939, 77.19886208192143329 ) ) ;
#11156 = CARTESIAN_POINT ( 'NONE',  ( 76.88867513459484826, 159.8737954434940036, -14.99999999999976907 ) ) ;
#11157 = CARTESIAN_POINT ( 'NONE',  ( 57.22499999726879594, 160.0630714827496206, -15.58253175000000823 ) ) ;
#11158 = CARTESIAN_POINT ( 'NONE',  ( -10.00000000000000711, 207.0476921513413515, 9.501137918078566003 ) ) ;
#11159 = CARTESIAN_POINT ( 'NONE',  ( -6.500000000000000888, -1.360915494584213459, -5.718331000733963165 ) ) ;
#11160 = CARTESIAN_POINT ( 'NONE',  ( 62.42499999726881299, 141.7447067706911810, 9.630534252274376428 ) ) ;
#11161 = CARTESIAN_POINT ( 'NONE',  ( 77.37499999726881583, 155.0000000000000000, -15.58253175000000823 ) ) ;
#11162 = CARTESIAN_POINT ( 'NONE',  ( -7.375838497908182134, 217.2372850707499765, 78.95113791807858661 ) ) ;
#11163 = CARTESIAN_POINT ( 'NONE',  ( 10.00000000000000711, 206.9523078486586201, 101.0011379180785696 ) ) ;
#11164 = CARTESIAN_POINT ( 'NONE',  ( 0.000000000000000000, 0.000000000000000000, 0.000000000000000000 ) ) ;
#11165 = ORIENTED_EDGE ( 'NONE', *, *, #23292, .T. ) ;
#11166 = CARTESIAN_POINT ( 'NONE',  ( -3.044812012439970683, 197.4746971517856196, 1.898862081921434353 ) ) ;
#11167 = CARTESIAN_POINT ( 'NONE',  ( 0.05014649552828288198, 194.3824533091408000, 64.74886208192143044 ) ) ;
#11168 = CARTESIAN_POINT ( 'NONE',  ( 8.062137200540822946, 212.9164362838583315, 69.69886208192144750 ) ) ;
#11169 = CARTESIAN_POINT ( 'NONE',  ( -9.736236675708031640, 214.0148392665760753, 8.798862081921434708 ) ) ;
#11170 = FACE_OUTER_BOUND ( 'NONE', #30022, .T. ) ;
#11171 = CARTESIAN_POINT ( 'NONE',  ( -3.044812012440131443, 216.5253028482142952, 25.10113791807856742 ) ) ;
#11172 = CARTESIAN_POINT ( 'NONE',  ( 9.984503880673420539, 210.2968891136705167, 84.84886208192143897 ) ) ;
#11173 = ORIENTED_EDGE ( 'NONE', *, *, #1797, .T. ) ;
#11174 = CARTESIAN_POINT ( 'NONE',  ( 63.31132485994281467, 140.7341522555726669, -4.635254915624220651 ) ) ;
#11175 = ORIENTED_EDGE ( 'NONE', *, *, #10432, .F. ) ;
#11176 = CARTESIAN_POINT ( 'NONE',  ( -8.015496119326597224, 209.5516654185217362, 62.64886208192143613 ) ) ;
#11177 = ORIENTED_EDGE ( 'NONE', *, *, #28713, .F. ) ;
#11178 = CARTESIAN_POINT ( 'NONE',  ( 76.22499999726881015, 149.9369285172503510, 15.58253174999999580 ) ) ;
#11179 = VERTEX_POINT ( 'NONE', #2108 ) ;
#11180 = LINE ( 'NONE', #21557, #8630 ) ;
#11181 = CARTESIAN_POINT ( 'NONE',  ( 72.62499999726880162, 138.6155565068815463, -3.929120461958505118E-15 ) ) ;
#11182 = CARTESIAN_POINT ( 'NONE',  ( 8.015496119326531499, 209.5516654185219636, 64.85113791807857808 ) ) ;
#11183 = EDGE_CURVE ( 'NONE', #12431, #6856, #20868, .T. ) ;
#11184 = DIRECTION ( 'NONE',  ( -1.000000000000000000, 0.000000000000000000, 0.000000000000000000 ) ) ;
#11185 = CARTESIAN_POINT ( 'NONE',  ( 34.50000000000000000, 155.0000000000000000, -14.50000000000000711 ) ) ;
#11186 = CARTESIAN_POINT ( 'NONE',  ( -2.517493886309087880, 214.5937144450984135, 45.09886208192144608 ) ) ;
#11187 = CARTESIAN_POINT ( 'NONE',  ( 6.139770520408368348, 198.4640165459539674, 77.45113791807854398 ) ) ;
#11188 = CARTESIAN_POINT ( 'NONE',  ( -6.139770520408369237, 215.5359834540460042, 63.95113791807857950 ) ) ;
#11189 = EDGE_CURVE ( 'NONE', #31748, #28486, #14873, .T. ) ;
#11190 = CARTESIAN_POINT ( 'NONE',  ( -65.50384660342780307, 120.9385549553365848, -18.99615339657220758 ) ) ;
#11191 = CARTESIAN_POINT ( 'NONE',  ( -0.05014649552807731031, 198.5883022060938572, 23.75113791807855890 ) ) ;
#11192 = CARTESIAN_POINT ( 'NONE',  ( 130.2499999999999716, 2.997323040913146538E-14, 35.00000599999999906 ) ) ;
#11193 = CARTESIAN_POINT ( 'NONE',  ( 60.68867513459482410, 150.1262045565064795, -15.00000000000007638 ) ) ;
#11194 = CARTESIAN_POINT ( 'NONE',  ( 45.12499999726880873, 155.0000000000000000, -15.58253175000000823 ) ) ;
#11195 = CARTESIAN_POINT ( 'NONE',  ( -9.680171189290831535, 214.0920067884431148, 51.80113791807857382 ) ) ;
#11196 = DIRECTION ( 'NONE',  ( 0.000000000000000000, -0.04769215134144196705, 0.9988620819214357738 ) ) ;
#11197 = CARTESIAN_POINT ( 'NONE',  ( -9.984503880673473830, 210.2968891136704315, 96.65113791807857524 ) ) ;
#11198 = CARTESIAN_POINT ( 'NONE',  ( -6.220909254589537696, 198.5229672870051445, 69.05113791807856671 ) ) ;
#11199 = CARTESIAN_POINT ( 'NONE',  ( -3.753561863808878130, 218.3979405102790281, 30.09886208192144252 ) ) ;
#11200 = CARTESIAN_POINT ( 'NONE',  ( -0.05014649552828402690, 217.5146222423826714, 39.24886208192143044 ) ) ;
#11201 = CARTESIAN_POINT ( 'NONE',  ( 88.49999999453763166, 170.2462022514548323, -7.872454543227099337E-15 ) ) ;
#11202 = CARTESIAN_POINT ( 'NONE',  ( 9.736236675707914401, 214.0148392665762458, 73.70113791807857240 ) ) ;
#11203 = CARTESIAN_POINT ( 'NONE',  ( -2.517493886308901807, 199.4062855549015012, 101.9011379180785895 ) ) ;
#11204 = EDGE_CURVE ( 'NONE', #27181, #18870, #33615, .T. ) ;
#11205 = CARTESIAN_POINT ( 'NONE',  ( 9.984503880673420539, 210.2968891136705167, 48.84886208192143187 ) ) ;
#11206 = DIRECTION ( 'NONE',  ( 0.000000000000000000, 1.000000000000000000, 0.000000000000000000 ) ) ;
#11207 = VERTEX_POINT ( 'NONE', #26275 ) ;
#11208 = CARTESIAN_POINT ( 'NONE',  ( 12.01549611932659367, 203.1486557965466773, 64.14886208192143613 ) ) ;
#11209 = EDGE_LOOP ( 'NONE', ( #2289, #25889, #17489, #22174 ) ) ;
#11210 = CARTESIAN_POINT ( 'NONE',  ( 7.984503880673422316, 209.6470497212048372, 33.84886208192144608 ) ) ;
#11211 = ADVANCED_FACE ( 'NONE', ( #28998 ), #28509, .F. ) ;
#11212 = VERTEX_POINT ( 'NONE', #3101 ) ;
#11213 = VECTOR ( 'NONE', #1938, 1000.000000000000000 ) ;
#11214 = CARTESIAN_POINT ( 'NONE',  ( 76.67499999726881299, 141.7447067706911810, 9.630534252274376428 ) ) ;
#11215 = DIRECTION ( 'NONE',  ( 1.000000000000000000, 0.000000000000000000, 0.000000000000000000 ) ) ;
#11216 = FACE_OUTER_BOUND ( 'NONE', #32702, .T. ) ;
#11217 = CARTESIAN_POINT ( 'NONE',  ( 6.444103211791042618, 202.2591342207267644, 56.30113791807857382 ) ) ;
#11218 = CARTESIAN_POINT ( 'NONE',  ( 6.139770520408223575, 215.5359834540460611, 36.54886208192142050 ) ) ;
#11219 = CARTESIAN_POINT ( 'NONE',  ( 69.57499999726881867, 164.1591823560292198, -12.60653300113719766 ) ) ;
#11220 = ORIENTED_EDGE ( 'NONE', *, *, #12277, .T. ) ;
#11221 = DIRECTION ( 'NONE',  ( 0.000000000000000000, 0.000000000000000000, 1.000000000000000000 ) ) ;
#11222 = CARTESIAN_POINT ( 'NONE',  ( 100.3117322205716420, 155.0000000000000000, 12.10452846326767506 ) ) ;
#11223 = CARTESIAN_POINT ( 'NONE',  ( -0.05014649552828365914, 215.4116977939061144, 12.24886208192143577 ) ) ;
#11224 = CARTESIAN_POINT ( 'NONE',  ( -10.01549611932653860, 203.7984951890123284, 48.35113791807855677 ) ) ;
#11225 = CARTESIAN_POINT ( 'NONE',  ( 83.18867513459483121, 169.2658477444273331, -4.635254915624224203 ) ) ;
#11226 = CARTESIAN_POINT ( 'NONE',  ( -8.118202686958039038, 201.1607312380087080, 33.20113791807857240 ) ) ;
#11227 = CARTESIAN_POINT ( 'NONE',  ( 84.77499999726880731, 140.1801316387863778, 4.815267126137185549 ) ) ;
#11228 = CARTESIAN_POINT ( 'NONE',  ( -8.015496119326597224, 209.5516654185217362, 98.64886208192146455 ) ) ;
#11229 = CARTESIAN_POINT ( 'NONE',  ( 38.42499999726879878, 141.7447067706911810, 9.630534252274376428 ) ) ;
#11230 = DIRECTION ( 'NONE',  ( 0.000000000000000000, -1.000000000000000000, 0.000000000000000000 ) ) ;
#11231 = CARTESIAN_POINT ( 'NONE',  ( 115.4999999999999858, 155.0000000000000000, -6.938893903907228378E-15 ) ) ;
#11232 = CARTESIAN_POINT ( 'NONE',  ( 12.01549611932652972, 210.8513442034534933, 16.85113791807856742 ) ) ;
#11233 = CARTESIAN_POINT ( 'NONE',  ( -52.50000000000002132, 155.0000000000000000, -40.00000000000000000 ) ) ;
#11234 = CARTESIAN_POINT ( 'NONE',  ( 63.87499999726881583, 171.3844434931184253, -7.942151717890132712E-15 ) ) ;
#11235 = EDGE_CURVE ( 'NONE', #31983, #31659, #2363, .T. ) ;
#11236 = CARTESIAN_POINT ( 'NONE',  ( -9.984503880673473830, 210.2968891136704315, 63.65113791807857524 ) ) ;
#11237 = EDGE_CURVE ( 'NONE', #18787, #4684, #18672, .T. ) ;
#11238 = CARTESIAN_POINT ( 'NONE',  ( -8.062137200540920645, 212.9164362838581894, 39.80113791807857382 ) ) ;
#11239 = TOROIDAL_SURFACE ( 'NONE', #9607, 3.299999999999999822, 0.2000000000000000111 ) ;
#11240 = DIRECTION ( 'NONE',  ( -0.000000000000000000, -0.000000000000000000, -1.000000000000000000 ) ) ;
#11241 = CLOSED_SHELL ( 'NONE', ( #7017, #11794, #16560, #28032, #31880, #27094, #24780, #14327, #4389, #29519, #4299, #1189, #1835, #3287, #32040, #19966, #16623, #17611, #2488, #3536, #10827, #11861, #22629, #16812, #4358, #29170, #28471, #255, #33179, #32462, #4919, #2724, #23128, #18553, #18048, #23740, #26182, #27715, #12938, #15012, #1872, #7231, #31939, #24110, #5110, #25367, #29791, #30597, #13674, #30019, #25165, #25779, #11665, #29561, #16242, #5301, #30778, #20136, #21393, #2689, #23564, #28065, #21192, #24974, #22991, #11423, #26249, #30629, #6187, #3755, #30202, #33263, #19062, #15787, #29881, #9795, #25796, #411, #23878, #4367, #5634, #26977, #24739, #31861, #22020, #19165, #18875, #28093, #22853, #15371, #33337, #5174, #988 ) ) ;
#11242 = CARTESIAN_POINT ( 'NONE',  ( 55.08867513459482268, 167.7597621252805880, -9.270509831248443078 ) ) ;
#11243 = CARTESIAN_POINT ( 'NONE',  ( -9.736236675707914401, 199.9851607334237542, 102.2011379180785866 ) ) ;
#11244 = CARTESIAN_POINT ( 'NONE',  ( -9.984503880673420539, 203.7031108863293980, 11.34886208192143364 ) ) ;
#11245 = CARTESIAN_POINT ( 'NONE',  ( 63.39999999453763024, 141.2096805137202580, 4.480746418436733158 ) ) ;
#11246 = ORIENTED_EDGE ( 'NONE', *, *, #11060, .T. ) ;
#11247 = CARTESIAN_POINT ( 'NONE',  ( 0.05014649552807549926, 219.6175466908591716, 46.25113791807856956 ) ) ;
#11248 = PRODUCT_RELATED_PRODUCT_CATEGORY ( 'part', '', ( #23052 ) ) ;
#11249 = EDGE_CURVE ( 'NONE', #8868, #20312, #31234, .T. ) ;
#11250 = CYLINDRICAL_SURFACE ( 'NONE', #5560, 1.000000000000000222 ) ;
#11251 = CARTESIAN_POINT ( 'NONE',  ( -3.044812012439970683, 197.4746971517856196, 19.89886208192143613 ) ) ;
#11252 = CARTESIAN_POINT ( 'NONE',  ( 58.81132485994281467, 150.1262045565064795, 15.00000000000006395 ) ) ;
#11253 = CIRCLE ( 'NONE', #12321, 3.500000000000000444 ) ;
#11254 = ORIENTED_EDGE ( 'NONE', *, *, #622, .F. ) ;
#11255 = CARTESIAN_POINT ( 'NONE',  ( 10.00000000000000711, 206.9523078486586201, 77.00113791807858377 ) ) ;
#11256 = EDGE_CURVE ( 'NONE', #608, #6290, #16609, .T. ) ;
#11257 = VERTEX_POINT ( 'NONE', #553 ) ;
#11258 = CARTESIAN_POINT ( 'NONE',  ( 49.81132485994280756, 159.8737954434936057, -15.00000000000002665 ) ) ;
#11259 = DIRECTION ( 'NONE',  ( -1.000000000000000000, 0.000000000000000000, 0.000000000000000000 ) ) ;
#11260 = VERTEX_POINT ( 'NONE', #31068 ) ;
#11261 = CARTESIAN_POINT ( 'NONE',  ( -6.444103211791042618, 211.7408657792732356, 24.80113791807857027 ) ) ;
#11262 = AXIS2_PLACEMENT_3D ( 'NONE', #26432, #5807, #14153 ) ;
#11263 = CARTESIAN_POINT ( 'NONE',  ( -61.00005817115211926, 195.0000036356967712, -0.1622090645192997005 ) ) ;
#11264 = STYLED_ITEM ( 'NONE', ( #3702 ), #23704 ) ;
#11265 = CARTESIAN_POINT ( 'NONE',  ( -8.118202686958138514, 212.8392687619910930, 2.798862081921434708 ) ) ;
#11266 = CARTESIAN_POINT ( 'NONE',  ( 51.77499999726881441, 169.8198683612136222, -4.815267126137197984 ) ) ;
#11267 = ORIENTED_EDGE ( 'NONE', *, *, #29550, .T. ) ;
#11268 = CARTESIAN_POINT ( 'NONE',  ( 60.12499999726880873, 155.0000000000000000, 15.58253174999999402 ) ) ;
#11269 = DIRECTION ( 'NONE',  ( -1.000000000000000000, 0.000000000000000000, 0.000000000000000000 ) ) ;
#11270 = CARTESIAN_POINT ( 'NONE',  ( 61.48867513459482836, 167.7597621252805880, 9.270509831248428867 ) ) ;
#11271 = CONICAL_SURFACE ( 'NONE', #33574, 27.50000000000000355, 1.047197551196595411 ) ;
#11272 = DIRECTION ( 'NONE',  ( 1.000000000000000000, 0.000000000000000000, 0.000000000000000000 ) ) ;
#11273 = CARTESIAN_POINT ( 'NONE',  ( -8.118202686958138514, 212.8392687619910930, 86.79886208192142760 ) ) ;
#11274 = CARTESIAN_POINT ( 'NONE',  ( 58.77499999726881441, 140.1801316387863778, 4.815267126137185549 ) ) ;
#11275 = CARTESIAN_POINT ( 'NONE',  ( 3.044812012440130555, 197.4746971517856764, 26.60113791807856742 ) ) ;
#11276 = CARTESIAN_POINT ( 'NONE',  ( 73.38867513459481984, 169.2658477444273331, 4.635254915624208216 ) ) ;
#11277 = CARTESIAN_POINT ( 'NONE',  ( 12.01549611932659367, 203.1486557965466773, 79.14886208192143613 ) ) ;
#11278 = CARTESIAN_POINT ( 'NONE',  ( 74.80000000000001137, 167.3344367211045096, -8.961492836873482304 ) ) ;
#11279 = CARTESIAN_POINT ( 'NONE',  ( 65.18867513459481700, 169.2658477444273331, -4.635254915624224203 ) ) ;
#11280 = FACE_OUTER_BOUND ( 'NONE', #2511, .T. ) ;
#11281 = CARTESIAN_POINT ( 'NONE',  ( -3.135527875058821579, 197.5041725223112223, 92.90113791807857524 ) ) ;
#11282 = CARTESIAN_POINT ( 'NONE',  ( 6.818286579240217193, -1.325012739682874141, -6.208253321455268647 ) ) ;
#11283 = CARTESIAN_POINT ( 'NONE',  ( 36.27499999726880731, 160.0630714827496206, 15.58253174999999402 ) ) ;
#11284 = CARTESIAN_POINT ( 'NONE',  ( 10.00000000000000711, 206.9523078486586201, 35.00113791807856956 ) ) ;
#11285 = CARTESIAN_POINT ( 'NONE',  ( 76.52499999726880731, 140.1801316387863778, 4.815267126137185549 ) ) ;
#11286 = ORIENTED_EDGE ( 'NONE', *, *, #23556, .F. ) ;
#11287 = DIRECTION ( 'NONE',  ( 0.000000000000000000, 0.000000000000000000, 1.000000000000000000 ) ) ;
#11288 = CARTESIAN_POINT ( 'NONE',  ( 42.99999999453763166, 155.0000000000000000, 14.49999999999999467 ) ) ;
#11289 = CARTESIAN_POINT ( 'NONE',  ( -12.00000000000000711, 207.0476921513413515, 18.50113791807856956 ) ) ;
#11290 = CONICAL_SURFACE ( 'NONE', #31968, 31.00000000000000000, 1.466076571675243967 ) ;
#11291 = VECTOR ( 'NONE', #29908, 1000.000000000000000 ) ;
#11292 = DIRECTION ( 'NONE',  ( 1.000000000000000000, 0.000000000000000000, 0.000000000000000000 ) ) ;
#11293 = EDGE_LOOP ( 'NONE', ( #2388, #4943 ) ) ;
#11294 =( GEOMETRIC_REPRESENTATION_CONTEXT ( 3 ) GLOBAL_UNCERTAINTY_ASSIGNED_CONTEXT ( ( #11018 ) ) GLOBAL_UNIT_ASSIGNED_CONTEXT ( ( #11061, #29617, #21443 ) ) REPRESENTATION_CONTEXT ( 'NONE', 'WORKASPACE' ) );
#11295 = TOROIDAL_SURFACE ( 'NONE', #10690, 4.999999999999993783, 1.000000000000000222 ) ;
#11296 = CARTESIAN_POINT ( 'NONE',  ( -12.00000000000000711, 206.9523078486584780, 32.49886208192143044 ) ) ;
#11297 = CARTESIAN_POINT ( 'NONE',  ( 10.40000000000000036, 0.000000000000000000, -5.400000000000002132 ) ) ;
#11298 = CARTESIAN_POINT ( 'NONE',  ( 10.01549611932653860, 210.2015048109876716, 49.85113791807857808 ) ) ;
#11299 = ORIENTED_EDGE ( 'NONE', *, *, #28462, .T. ) ;
#11300 =( BOUNDED_CURVE ( )  B_SPLINE_CURVE ( 2, ( #15824, #3044, #8488, #13268, #21103, #21268, #5755, #21597, #10722 ),
 .UNSPECIFIED., .F., .T. ) 
 B_SPLINE_CURVE_WITH_KNOTS ( ( 3, 2, 2, 2, 3 ),
 ( 0.005159801592109723549, 0.007142857142857129624, 0.01071428571428571092, 0.01428571428571429047, 0.01785714285714287350 ),
 .UNSPECIFIED. ) 
 CURVE ( )  GEOMETRIC_REPRESENTATION_ITEM ( )  RATIONAL_B_SPLINE_CURVE ( ( 0.9758271243137095485, 0.9728238588305329060, 1.000000000000000000, 0.9510565162951534202, 1.000000000000000000, 0.9510565162951534202, 1.000000000000000000, 0.9510565162951523099, 1.000000000000001110 ) ) 
 REPRESENTATION_ITEM ( '' )  );
#11301 = CARTESIAN_POINT ( 'NONE',  ( 0.05014649552828262524, 198.5883022060938572, 10.74886208192143577 ) ) ;
#11302 = AXIS2_PLACEMENT_3D ( 'NONE', #5695, #13533, #15427 ) ;
#11303 = CARTESIAN_POINT ( 'NONE',  ( 50.81132485994280756, 150.1262045565064227, 15.00000000000001599 ) ) ;
#11304 = EDGE_LOOP ( 'NONE', ( #2341, #28612, #6308, #3584 ) ) ;
#11305 = CARTESIAN_POINT ( 'NONE',  ( -2.426778023690076225, 199.3768101843759553, 103.8988620819214361 ) ) ;
#11306 = CARTESIAN_POINT ( 'NONE',  ( 7.984503880673485376, 204.3529502787953902, 41.15113791807857524 ) ) ;
#11307 = CARTESIAN_POINT ( 'NONE',  ( 0.000000000000000000, -1.773042676681340524, 1.734723475976807094E-15 ) ) ;
#11308 = VERTEX_POINT ( 'NONE', #25778 ) ;
#11309 = CARTESIAN_POINT ( 'NONE',  ( 38.92499999726881299, 145.8408176439707802, -12.60653300113719588 ) ) ;
#11310 = AXIS2_PLACEMENT_3D ( 'NONE', #24923, #17088, #8746 ) ;
#11311 = CARTESIAN_POINT ( 'NONE',  ( 3.135527875058981895, 197.5041725223112792, 58.59886208192143897 ) ) ;
#11312 = CARTESIAN_POINT ( 'NONE',  ( 33.37499999726880873, 155.0000000000000000, -15.58253175000000823 ) ) ;
#11313 = PLANE ( 'NONE',  #32858 ) ;
#11314 = CARTESIAN_POINT ( 'NONE',  ( 0.05014649552807626948, 215.4116977939061144, 94.25113791807859798 ) ) ;
#11315 = CIRCLE ( 'NONE', #2110, 5.200000000000002842 ) ;
#11316 = CARTESIAN_POINT ( 'NONE',  ( 55.99999999999999289, 139.7537977485451393, -4.138211985947621020E-15 ) ) ;
#11317 = CARTESIAN_POINT ( 'NONE',  ( -8.000000000000008882, 206.9523078486584780, 68.49886208192144466 ) ) ;
#11318 = DIRECTION ( 'NONE',  ( 0.000000000000000000, 0.000000000000000000, -1.000000000000000000 ) ) ;
#11319 = CIRCLE ( 'NONE', #11880, 8.624472924841564136 ) ;
#11320 = CARTESIAN_POINT ( 'NONE',  ( 56.02499999726880731, 160.0630714827496206, 15.58253174999999402 ) ) ;
#11322 = EDGE_LOOP ( 'NONE', ( #21305, #24208, #33306, #17801, #1035, #7591, #22602 ) ) ;
#11321 = CARTESIAN_POINT ( 'NONE',  ( 3.135527875058820690, 216.4958274776887492, 7.401137918078566358 ) ) ;
#11323 = CARTESIAN_POINT ( 'NONE',  ( 36.91132485994280898, 146.1832212156128890, 12.13525491562421976 ) ) ;
#11324 = CARTESIAN_POINT ( 'NONE',  ( 63.22499999726881015, 160.0630714827496206, -15.58253175000000823 ) ) ;
#11325 = CARTESIAN_POINT ( 'NONE',  ( 78.57499999726881867, 145.8408176439707802, 12.60653300113718345 ) ) ;
#11326 = CARTESIAN_POINT ( 'NONE',  ( -12.01549611932652972, 203.1486557965464499, 78.35113791807857808 ) ) ;
#11327 = CARTESIAN_POINT ( 'NONE',  ( -8.062137200540920645, 212.9164362838581894, 93.80113791807858092 ) ) ;
#11328 = FACE_OUTER_BOUND ( 'NONE', #30582, .T. ) ;
#11329 = VERTEX_POINT ( 'NONE', #2784 ) ;
#11330 = CARTESIAN_POINT ( 'NONE',  ( -9.984503880673420539, 203.7031108863293980, 2.348862081921433198 ) ) ;
#11331 = CARTESIAN_POINT ( 'NONE',  ( 7.456977232089471386, 196.8216656703012006, 64.44886208192143329 ) ) ;
#11332 = CARTESIAN_POINT ( 'NONE',  ( -6.220909254589682469, 215.4770327129947134, 62.94886208192143329 ) ) ;
#11333 = CARTESIAN_POINT ( 'NONE',  ( 7.375838497908012492, 217.2372850707501186, 6.548862081921433820 ) ) ;
#11334 = CARTESIAN_POINT ( 'NONE',  ( 2.000000000000000000, -0.8865213383406721492, -1.535499999999998977 ) ) ;
#11335 = CIRCLE ( 'NONE', #9705, 4.250000000000000000 ) ;
#11336 = CARTESIAN_POINT ( 'NONE',  ( -8.118202686958039038, 201.1607312380087080, 24.20113791807856884 ) ) ;
#11337 = CARTESIAN_POINT ( 'NONE',  ( -10.00000000000000711, 206.9523078486584495, 86.49886208192144466 ) ) ;
#11338 = ADVANCED_FACE ( 'NONE', ( #2448 ), #7726, .F. ) ;
#11339 = AXIS2_PLACEMENT_3D ( 'NONE', #8992, #21933, #20057 ) ;
#11340 = ORIENTED_EDGE ( 'NONE', *, *, #9176, .T. ) ;
#11341 = CARTESIAN_POINT ( 'NONE',  ( 101.3062541159399075, 155.0000000000000000, 0.000000000000000000 ) ) ;
#11342 = ORIENTED_EDGE ( 'NONE', *, *, #31819, .T. ) ;
#11343 = FACE_OUTER_BOUND ( 'NONE', #28185, .T. ) ;
#11344 = CARTESIAN_POINT ( 'NONE',  ( 8.000000000000008882, 207.0476921513415220, 72.99886208192144466 ) ) ;
#11345 = EDGE_LOOP ( 'NONE', ( #27767, #21892, #27718, #9659 ) ) ;
#11346 = VECTOR ( 'NONE', #3026, 1000.000000000000000 ) ;
#11347 = CARTESIAN_POINT ( 'NONE',  ( 78.12499999726883004, 155.0000000000000000, 15.58253174999999402 ) ) ;
#11348 = ORIENTED_EDGE ( 'NONE', *, *, #28931, .T. ) ;
#11349 = CARTESIAN_POINT ( 'NONE',  ( 69.28867513459483973, 170.7719333635740497, -7.904646289410545231E-15 ) ) ;
#11350 = CARTESIAN_POINT ( 'NONE',  ( 70.82499999726883289, 141.7447067706911810, -9.630534252274385310 ) ) ;
#11351 = CARTESIAN_POINT ( 'NONE',  ( 6.500168698208129925, 211.6636982574063381, 70.70113791807857240 ) ) ;
#11352 = CARTESIAN_POINT ( 'NONE',  ( 57.81132485994280756, 159.8737954434936057, -15.00000000000002665 ) ) ;
#11353 =( NAMED_UNIT ( * ) SI_UNIT ( $, .STERADIAN. ) SOLID_ANGLE_UNIT ( ) );
#11354 = CARTESIAN_POINT ( 'NONE',  ( 37.29999999999999716, 163.5228861582408797, 11.73074641843673049 ) ) ;
#11355 = CARTESIAN_POINT ( 'NONE',  ( -6.500168698208244500, 211.6636982574061676, 44.79886208192144181 ) ) ;
#11356 = CIRCLE ( 'NONE', #23856, 2.149999999999984812 ) ;
#11357 = CARTESIAN_POINT ( 'NONE',  ( 6.220909254589536808, 215.4770327129947702, 82.55113791807858092 ) ) ;
#11358 = CARTESIAN_POINT ( 'NONE',  ( 6.220909254589536808, 215.4770327129947702, 67.55113791807853829 ) ) ;
#11359 = CIRCLE ( 'NONE', #30414, 7.500000000000001776 ) ;
#11360 = CARTESIAN_POINT ( 'NONE',  ( -7.375838497908014268, 196.7627149292498530, 23.04886208192143826 ) ) ;
#11361 = FACE_BOUND ( 'NONE', #16389, .T. ) ;
#11362 = CARTESIAN_POINT ( 'NONE',  ( -6.444103211791042618, 211.7408657792732356, 24.80113791807857027 ) ) ;
#11363 = CARTESIAN_POINT ( 'NONE',  ( 6.874999999999999112, 4.690970937165706900, -7.298562697733104621 ) ) ;
#11364 = CARTESIAN_POINT ( 'NONE',  ( -3.499999999999999556, -0.3414694520252377630, -3.134021904840910022E-17 ) ) ;
#11365 = CARTESIAN_POINT ( 'NONE',  ( 46.62499999726880873, 138.6155565068815747, -3.929120461958505118E-15 ) ) ;
#11366 = EDGE_CURVE ( 'NONE', #10401, #28279, #18447, .T. ) ;
#11367 = CARTESIAN_POINT ( 'NONE',  ( 9.680171189290831535, 199.9079932115568852, 47.30113791807856671 ) ) ;
#11368 = CARTESIAN_POINT ( 'NONE',  ( 7.500000000000000000, 3.160172554975063886, -7.231829826456836585 ) ) ;
#11369 = CARTESIAN_POINT ( 'NONE',  ( -10.00000000000000711, 207.0476921513413515, 96.50113791807856956 ) ) ;
#11370 = CARTESIAN_POINT ( 'NONE',  ( 9.984503880673473830, 203.7031108863295401, 68.15113791807857524 ) ) ;
#11371 = AXIS2_PLACEMENT_3D ( 'NONE', #32904, #9562, #23021 ) ;
#11372 = CARTESIAN_POINT ( 'NONE',  ( 9.736236675708031640, 199.9851607334238963, 34.29886208192143471 ) ) ;
#11373 = CARTESIAN_POINT ( 'NONE',  ( 9.984503880673420539, 210.2968891136705736, 39.84886208192142476 ) ) ;
#11374 = CARTESIAN_POINT ( 'NONE',  ( 87.69999999453764872, 142.6655632788954620, -8.961492836873480528 ) ) ;
#11375 = CARTESIAN_POINT ( 'NONE',  ( -3.753561863808691168, 195.6020594897209435, 74.90113791807856103 ) ) ;
#11376 = CARTESIAN_POINT ( 'NONE',  ( 4.903702542908601636, 200.1653181626581102, 98.45113791807858661 ) ) ;
#11377 = CARTESIAN_POINT ( 'NONE',  ( -9.984503880673420539, 203.7031108863293980, 59.34886208192141765 ) ) ;
#11378 = ADVANCED_FACE ( 'NONE', ( #12828 ), #33368, .F. ) ;
#11379 = EDGE_LOOP ( 'NONE', ( #32707, #14174, #31266, #32947, #33520 ) ) ;
#11380 = CARTESIAN_POINT ( 'NONE',  ( -9.736236675708031640, 214.0148392665760753, 59.79886208192143471 ) ) ;
#11381 = ORIENTED_EDGE ( 'NONE', *, *, #11235, .T. ) ;
#11382 = CARTESIAN_POINT ( 'NONE',  ( 68.97499999726881015, 140.1801316387863778, -4.815267126137194431 ) ) ;
#11383 = CARTESIAN_POINT ( 'NONE',  ( -8.000000000000008882, 206.9523078486584780, 29.49886208192143400 ) ) ;
#11384 = EDGE_CURVE ( 'NONE', #5152, #28610, #21159, .T. ) ;
#11385 = AXIS2_PLACEMENT_3D ( 'NONE', #21040, #8111, #5533 ) ;
#11386 = ORIENTED_EDGE ( 'NONE', *, *, #28885, .T. ) ;
#11387 = CARTESIAN_POINT ( 'NONE',  ( 75.17499999726881299, 145.8408176439707802, -12.60653300113719588 ) ) ;
#11388 = CARTESIAN_POINT ( 'NONE',  ( 91.60208470531341618, 155.0000000000000000, 0.000000000000000000 ) ) ;
#11389 = EDGE_CURVE ( 'NONE', #30073, #8400, #26833, .T. ) ;
#11390 = CARTESIAN_POINT ( 'NONE',  ( 5.000000000000000888, 0.000000000000000000, -25.03750572909317285 ) ) ;
#11391 = CARTESIAN_POINT ( 'NONE',  ( -8.000000000000008882, 207.0476921513413515, 51.50113791807856956 ) ) ;
#11392 =( NAMED_UNIT ( * ) SI_UNIT ( $, .STERADIAN. ) SOLID_ANGLE_UNIT ( ) );
#11393 = CARTESIAN_POINT ( 'NONE',  ( 8.118202686958138514, 201.1607312380088501, 37.29886208192143471 ) ) ;
#11394 = CARTESIAN_POINT ( 'NONE',  ( 69.77499999726880731, 169.8198683612136222, -4.815267126137197984 ) ) ;
#11395 = ORIENTED_EDGE ( 'NONE', *, *, #1334, .T. ) ;
#11396 = FACE_OUTER_BOUND ( 'NONE', #23916, .T. ) ;
#11397 = DIRECTION ( 'NONE',  ( 1.000000000000000000, 0.000000000000000000, 0.000000000000000000 ) ) ;
#11398 = LINE ( 'NONE', #14277, #10920 ) ;
#11399 = CARTESIAN_POINT ( 'NONE',  ( -4.984841277089891776, 213.7757310962905990, 11.94886208192143506 ) ) ;
#11400 = CARTESIAN_POINT ( 'NONE',  ( 3.044812012440130555, 197.4746971517856764, 47.60113791807857098 ) ) ;
#11401 = EDGE_CURVE ( 'NONE', #22486, #24793, #23219, .T. ) ;
#11402 = CARTESIAN_POINT ( 'NONE',  ( -6.139770520408369237, 215.5359834540460042, 36.95113791807857240 ) ) ;
#11403 = CARTESIAN_POINT ( 'NONE',  ( 85.27499999726879309, 149.9369285172503510, -15.58253175000000823 ) ) ;
#11404 = CARTESIAN_POINT ( 'NONE',  ( -2.426778023690076225, 199.3768101843759553, 103.8988620819214361 ) ) ;
#11405 = CARTESIAN_POINT ( 'NONE',  ( 38.52499999726881441, 140.1801316387863778, 4.815267126137185549 ) ) ;
#11406 = CARTESIAN_POINT ( 'NONE',  ( 81.38867513459483405, 169.2658477444273331, 4.635254915624208216 ) ) ;
#11407 = DIRECTION ( 'NONE',  ( -1.000000000000000000, -0.000000000000000000, -0.000000000000000000 ) ) ;
#11408 = CARTESIAN_POINT ( 'NONE',  ( 3.753561863808689836, 218.3979405102790565, 22.40113791807856813 ) ) ;
#11409 = AXIS2_PLACEMENT_3D ( 'NONE', #23527, #5954, #29134 ) ;
#11410 = CARTESIAN_POINT ( 'NONE',  ( 0.9763930676190096802, -8.096533237419681228, -7.213065638943101376 ) ) ;
#11411 = EDGE_CURVE ( 'NONE', #33215, #13027, #32815, .T. ) ;
#11412 = CARTESIAN_POINT ( 'NONE',  ( -9.984503880673473830, 210.2968891136704315, 66.65113791807857524 ) ) ;
#11413 = CARTESIAN_POINT ( 'NONE',  ( -10.00000000000000711, 207.0476921513413515, 42.50113791807856956 ) ) ;
#11414 = CARTESIAN_POINT ( 'NONE',  ( 8.640141755188686545, 206.6086104956403915, 111.6972426105882477 ) ) ;
#11415 = CARTESIAN_POINT ( 'NONE',  ( 115.4999999999999858, 155.0000000000000000, -112.0000000000000426 ) ) ;
#11416 = CARTESIAN_POINT ( 'NONE',  ( 3.662846001189864698, 218.4274158808046593, 6.398862081921435241 ) ) ;
#11417 = CARTESIAN_POINT ( 'NONE',  ( 10.01549611932659367, 203.7984951890124421, 13.14886208192143435 ) ) ;
#11418 = CARTESIAN_POINT ( 'NONE',  ( 64.59999999453764019, 168.7903194862797420, 4.480746418436729606 ) ) ;
#11419 = ORIENTED_EDGE ( 'NONE', *, *, #32456, .F. ) ;
#11420 = CARTESIAN_POINT ( 'NONE',  ( 3.753561863808689836, 218.3979405102790565, 46.40113791807856813 ) ) ;
#11421 = CARTESIAN_POINT ( 'NONE',  ( 2.426778023690261410, 199.3768101843759837, 68.60113791807857808 ) ) ;
#11422 = CARTESIAN_POINT ( 'NONE',  ( -0.05014649552828403384, 217.5146222423826714, 30.24886208192142689 ) ) ;
#11423 = ADVANCED_FACE ( 'NONE', ( #18612 ), #5492, .T. ) ;
#11424 = CARTESIAN_POINT ( 'NONE',  ( 75.81132485994281467, 159.8737954434936057, -15.00000000000002665 ) ) ;
#11425 = ORIENTED_EDGE ( 'NONE', *, *, #4938, .F. ) ;
#11426 = CARTESIAN_POINT ( 'NONE',  ( -8.118202686958039038, 201.1607312380087080, 81.20113791807857240 ) ) ;
#11427 = EDGE_LOOP ( 'NONE', ( #17978, #32147, #14905, #2935, #25416, #24673, #1731, #4347 ) ) ;
#11428 = CARTESIAN_POINT ( 'NONE',  ( 7.500000000000000000, -4.330127018922199866, -7.422398894150035176 ) ) ;
#11429 = CARTESIAN_POINT ( 'NONE',  ( 1.153701847711638750, 3.375361811986500538, -2.900000000000002132 ) ) ;
#11430 = ORIENTED_EDGE ( 'NONE', *, *, #29550, .F. ) ;
#11431 = CARTESIAN_POINT ( 'NONE',  ( 7.984503880673485376, 204.3529502787953902, 23.15113791807856458 ) ) ;
#11432 = ADVANCED_FACE ( 'NONE', ( #5982 ), #4544, .T. ) ;
#11433 = CARTESIAN_POINT ( 'NONE',  ( -27.50000000000000000, 15.87713240271469672, -2.456200930618631428 ) ) ;
#11434 = CARTESIAN_POINT ( 'NONE',  ( -6.220909254589682469, 215.4770327129946850, 5.948862081921435063 ) ) ;
#11435 = CARTESIAN_POINT ( 'NONE',  ( 49.67499999726880588, 168.2552932293087906, -9.630534252274387086 ) ) ;
#11436 = ORIENTED_EDGE ( 'NONE', *, *, #27207, .T. ) ;
#11437 = CARTESIAN_POINT ( 'NONE',  ( 55.82499999726880446, 168.2552932293087906, 9.630534252274372875 ) ) ;
#11438 = DIRECTION ( 'NONE',  ( 1.000000000000000000, 0.000000000000000000, 0.000000000000000000 ) ) ;
#11439 = DIRECTION ( 'NONE',  ( 0.000000000000000000, 0.000000000000000000, 1.000000000000000000 ) ) ;
#11440 = CARTESIAN_POINT ( 'NONE',  ( -22.98492866215539010, 18.48391005502964646, -1.088725517910800189 ) ) ;
#11441 = CARTESIAN_POINT ( 'NONE',  ( 6.139770520408223575, 215.5359834540460611, 93.54886208192139918 ) ) ;
#11442 = CARTESIAN_POINT ( 'NONE',  ( 59.47499999726879594, 160.0630714827496206, -15.58253175000000823 ) ) ;
#11443 = CARTESIAN_POINT ( 'NONE',  ( 6.220909254589536808, 215.4770327129947702, 19.55113791807856671 ) ) ;
#11444 = EDGE_CURVE ( 'NONE', #12552, #15275, #16543, .T. ) ;
#11445 = CARTESIAN_POINT ( 'NONE',  ( -3.662846001189865142, 195.5725841191952838, 79.89886208192143613 ) ) ;
#11446 = CARTESIAN_POINT ( 'NONE',  ( 74.60000000000000853, 159.7113355953771077, -14.50000000000000888 ) ) ;
#11447 = CARTESIAN_POINT ( 'NONE',  ( 62.71132485994281325, 155.0000000000000000, 15.00000000000001243 ) ) ;
#11448 = LINE ( 'NONE', #32386, #5525 ) ;
#11449 = CARTESIAN_POINT ( 'NONE',  ( -3.044812012440131443, 216.5253028482142952, 91.10113791807857808 ) ) ;
#11450 = CARTESIAN_POINT ( 'NONE',  ( 115.4999999999999858, 180.9145392013172682, 100.8678580070898931 ) ) ;
#11451 = CARTESIAN_POINT ( 'NONE',  ( 47.07499999726880446, 141.7447067706911810, -9.630534252274385310 ) ) ;
#11452 = CARTESIAN_POINT ( 'NONE',  ( 9.984503880673470277, 203.7031108863295401, 41.15113791807855392 ) ) ;
#11453 = CARTESIAN_POINT ( 'NONE',  ( 74.02499999726879309, 160.0630714827496206, 15.58253174999999402 ) ) ;
#11454 = VERTEX_POINT ( 'NONE', #24555 ) ;
#11455 = CARTESIAN_POINT ( 'NONE',  ( 107.0104235265664556, 155.0000000000000000, 11.99999999999998224 ) ) ;
#11456 = CARTESIAN_POINT ( 'NONE',  ( 47.09999999453762598, 150.2886644046228639, 14.49999999999999645 ) ) ;
#11457 = CARTESIAN_POINT ( 'NONE',  ( 12.00000000000000711, 206.9523078486586485, 17.00113791807856956 ) ) ;
#11458 = PRODUCT_DEFINITION_SHAPE ( 'NONE', 'NONE',  #33695 ) ;
#11459 = DIRECTION ( 'NONE',  ( 1.000000000000000000, -0.000000000000000000, -0.000000000000000000 ) ) ;
#11460 = CARTESIAN_POINT ( 'NONE',  ( 7.500000000000000000, -4.330127018922199866, -7.422398894150035176 ) ) ;
#11461 = ORIENTED_EDGE ( 'NONE', *, *, #33328, .T. ) ;
#11462 = CARTESIAN_POINT ( 'NONE',  ( -9.736236675708031640, 214.0148392665760753, 32.79886208192143471 ) ) ;
#11463 = CARTESIAN_POINT ( 'NONE',  ( 10.00000000000000711, 206.9523078486586201, -0.9988620819214343305 ) ) ;
#11464 = CARTESIAN_POINT ( 'NONE',  ( -9.984503880673473830, 210.2968891136704315, 54.65113791807858235 ) ) ;
#11465 = EDGE_LOOP ( 'NONE', ( #8036, #21352 ) ) ;
#11466 = CARTESIAN_POINT ( 'NONE',  ( 8.000000000000008882, 207.0476921513415220, 15.99886208192143577 ) ) ;
#11467 = AXIS2_PLACEMENT_3D ( 'NONE', #19947, #15006, #30346 ) ;
#11468 = UNCERTAINTY_MEASURE_WITH_UNIT (LENGTH_MEASURE( 1.000000000000000082E-05 ), #13039, 'distance_accuracy_value', 'NONE');
#11469 = CARTESIAN_POINT ( 'NONE',  ( -16.66875746037182537, -22.13055319862718662, -17.88577775926225755 ) ) ;
#11470 = AXIS2_PLACEMENT_3D ( 'NONE', #3380, #18887, #1164 ) ;
#11471 = ORIENTED_EDGE ( 'NONE', *, *, #12526, .F. ) ;
#11472 = CARTESIAN_POINT ( 'NONE',  ( 7.984503880673422316, 209.6470497212048372, 96.84886208192143897 ) ) ;
#11473 = EDGE_CURVE ( 'NONE', #11260, #20519, #8340, .T. ) ;
#11474 = EDGE_CURVE ( 'NONE', #8568, #19176, #29336, .T. ) ;
#11475 = CARTESIAN_POINT ( 'NONE',  ( -2.426778023690262742, 214.6231898156240163, 37.10113791807857098 ) ) ;
#11476 = DIRECTION ( 'NONE',  ( 0.000000000000000000, 0.000000000000000000, -1.000000000000000000 ) ) ;
#11477 = VERTEX_POINT ( 'NONE', #24045 ) ;
#11478 = CARTESIAN_POINT ( 'NONE',  ( 40.32499999726881157, 145.8408176439707802, 12.60653300113718345 ) ) ;
#11479 = CARTESIAN_POINT ( 'NONE',  ( -10.01549611932659722, 210.2015048109875011, 59.64886208192143613 ) ) ;
#11480 = CARTESIAN_POINT ( 'NONE',  ( 42.97499999726881015, 140.1801316387863778, -4.815267126137194431 ) ) ;
#11481 = CYLINDRICAL_SURFACE ( 'NONE', #31761, 15.50000000000001066 ) ;
#11482 = CARTESIAN_POINT ( 'NONE',  ( -8.000000000000008882, 207.0476921513413515, 93.50113791807858377 ) ) ;
#11483 = EDGE_CURVE ( 'NONE', #20312, #9970, #15324, .T. ) ;
#11484 = CARTESIAN_POINT ( 'NONE',  ( 57.10000000000000142, 168.7903194862797420, 4.480746418436729606 ) ) ;
#11485 = CARTESIAN_POINT ( 'NONE',  ( 63.18867513459480989, 169.2658477444273331, -4.635254915624224203 ) ) ;
#11486 = CARTESIAN_POINT ( 'NONE',  ( -8.015496119326597224, 209.5516654185217362, 68.64886208192142192 ) ) ;
#11487 = CARTESIAN_POINT ( 'NONE',  ( 65.78867513459482552, 155.0000000000000000, 15.00000000000001243 ) ) ;
#11488 = DIRECTION ( 'NONE',  ( 0.000000000000000000, 0.000000000000000000, 1.000000000000000000 ) ) ;
#11489 = CARTESIAN_POINT ( 'NONE',  ( 54.62499999726880162, 138.6155565068815463, -3.929120461958505118E-15 ) ) ;
#11491 = VERTEX_POINT ( 'NONE', #29667 ) ;
#11490 = CARTESIAN_POINT ( 'NONE',  ( -8.062137200540920645, 212.9164362838581894, 6.801137918078565825 ) ) ;
#11492 = CARTESIAN_POINT ( 'NONE',  ( -54.30000000000002558, -88.00000000000000000, -20.00000000000000000 ) ) ;
#11493 = AXIS2_PLACEMENT_3D ( 'NONE', #3184, #13575, #27316 ) ;
#11494 = CARTESIAN_POINT ( 'NONE',  ( 68.02499999726880731, 160.0630714827496206, 15.58253174999999224 ) ) ;
#11495 = CARTESIAN_POINT ( 'NONE',  ( 75.77499999726880731, 169.8198683612136222, -4.815267126137197984 ) ) ;
#11496 = CARTESIAN_POINT ( 'NONE',  ( -9.680171189290831535, 214.0920067884431148, 72.80113791807858092 ) ) ;
#11497 = CARTESIAN_POINT ( 'NONE',  ( -9.984503880673475606, 210.2968891136704315, 96.65113791807858945 ) ) ;
#11498 = PLANE ( 'NONE',  #18345 ) ;
#11499 = ORIENTED_EDGE ( 'NONE', *, *, #14170, .T. ) ;
#11500 = CARTESIAN_POINT ( 'NONE',  ( 3.044812012439969795, 216.5253028482143520, 3.398862081921434797 ) ) ;
#11501 = CARTESIAN_POINT ( 'NONE',  ( -9.680171189290716072, 199.9079932115567146, 62.19886208192144039 ) ) ;
#11502 = CARTESIAN_POINT ( 'NONE',  ( -3.135527875058982783, 216.4958274776886924, 69.09886208192143897 ) ) ;
#11503 = CARTESIAN_POINT ( 'NONE',  ( 9.680171189290716072, 214.0920067884432854, 3.698862081921433731 ) ) ;
#11504 = DIRECTION ( 'NONE',  ( -1.000000000000000000, 0.000000000000000000, 0.000000000000000000 ) ) ;
#11505 = CARTESIAN_POINT ( 'NONE',  ( -8.062137200540920645, 212.9164362838581894, 18.80113791807856671 ) ) ;
#11506 = CARTESIAN_POINT ( 'NONE',  ( 6.220909254589681581, 198.5229672870052582, 88.44886208192144750 ) ) ;
#11507 = EDGE_LOOP ( 'NONE', ( #24861, #15998, #25044, #30323 ) ) ;
#11508 = CARTESIAN_POINT ( 'NONE',  ( 62.91132485994280188, 146.1832212156128890, 12.13525491562421976 ) ) ;
#11509 = ORIENTED_EDGE ( 'NONE', *, *, #20368, .T. ) ;
#11510 = CARTESIAN_POINT ( 'NONE',  ( 124.9999999999999716, -73.00000000000002842, -30.00000000000000000 ) ) ;
#11511 = CARTESIAN_POINT ( 'NONE',  ( 6.500168698208244500, 202.3363017425938324, 67.29886208192144181 ) ) ;
#11512 = EDGE_LOOP ( 'NONE', ( #19876, #24314, #705, #29570, #15605 ) ) ;
#11513 = CARTESIAN_POINT ( 'NONE',  ( 86.92499999726881299, 145.8408176439707802, -12.60653300113719588 ) ) ;
#11514 = ORIENTED_EDGE ( 'NONE', *, *, #2063, .F. ) ;
#11515 = FACE_OUTER_BOUND ( 'NONE', #8480, .T. ) ;
#11516 = AXIS2_PLACEMENT_3D ( 'NONE', #12831, #24220, #29341 ) ;
#11517 = CARTESIAN_POINT ( 'NONE',  ( 78.02499999726879309, 160.0630714827496206, 15.58253174999999402 ) ) ;
#11518 = CARTESIAN_POINT ( 'NONE',  ( -6.444103211791042618, 211.7408657792732356, 69.80113791807856671 ) ) ;
#11519 = CARTESIAN_POINT ( 'NONE',  ( -3.499999999999999112, 0.3416723310689526172, -2.899999999999999467 ) ) ;
#11520 = CIRCLE ( 'NONE', #25679, 2.149999999999985256 ) ;
#11521 = CARTESIAN_POINT ( 'NONE',  ( 34.10000000000000142, 141.2096805137202580, -4.480746418436742040 ) ) ;
#11522 = CARTESIAN_POINT ( 'NONE',  ( 4.903702542908435547, 213.8346818373419751, 42.54886208192144181 ) ) ;
#11523 = CARTESIAN_POINT ( 'NONE',  ( -3.135527875058821579, 197.5041725223112223, 92.90113791807857524 ) ) ;
#11524 = CARTESIAN_POINT ( 'NONE',  ( -8.062137200540920645, 212.9164362838581894, 69.80113791807856671 ) ) ;
#11525 = CARTESIAN_POINT ( 'NONE',  ( -60.00000000000000000, -7.347880794884118356E-15, -20.00000000000001776 ) ) ;
#11526 = DIRECTION ( 'NONE',  ( 0.000000000000000000, 0.000000000000000000, 1.000000000000000000 ) ) ;
#11527 = DIRECTION ( 'NONE',  ( -1.000000000000000000, -0.000000000000000000, -0.000000000000000000 ) ) ;
#11528 = CARTESIAN_POINT ( 'NONE',  ( 50.02499999726880020, 160.0630714827496206, 15.58253174999999224 ) ) ;
#11529 =( BOUNDED_CURVE ( )  B_SPLINE_CURVE ( 2, ( #18489, #5369, #28871, #33657, #10826, #21201, #21362, #5529, #8261, #2984, #20878 ),
 .UNSPECIFIED., .F., .T. ) 
 B_SPLINE_CURVE_WITH_KNOTS ( ( 3, 2, 2, 2, 2, 3 ),
 ( 0.8928571428571429047, 0.8964285714285714635, 0.9000000000000000222, 0.9035714285714286920, 0.9071428571428572507, 0.9107142857142858094 ),
 .UNSPECIFIED. ) 
 CURVE ( )  GEOMETRIC_REPRESENTATION_ITEM ( )  RATIONAL_B_SPLINE_CURVE ( ( 1.000000000000000000, 0.9510565162951534202, 1.000000000000000000, 0.9510565162951534202, 1.000000000000000000, 0.9510565162951534202, 1.000000000000000000, 0.9510565162951534202, 1.000000000000000000, 0.9510565162951518658, 1.000000000000001554 ) ) 
 REPRESENTATION_ITEM ( '' )  );
#11530 = CARTESIAN_POINT ( 'NONE',  ( 0.05014649552807549926, 219.6175466908591716, 49.25113791807856956 ) ) ;
#11531 = CARTESIAN_POINT ( 'NONE',  ( 125.0000000000000000, 3.061616997868383121E-14, -20.00000000000000355 ) ) ;
#11532 = CARTESIAN_POINT ( 'NONE',  ( 10.00000000000000711, 206.9523078486586201, 95.00113791807856956 ) ) ;
#11533 = CARTESIAN_POINT ( 'NONE',  ( -10.01549611932653860, 203.7984951890123000, 69.35113791807857808 ) ) ;
#11534 = CARTESIAN_POINT ( 'NONE',  ( -7.375838497908014268, 196.7627149292498530, 32.04886208192143471 ) ) ;
#11535 = CARTESIAN_POINT ( 'NONE',  ( -3.044812012439970683, 197.4746971517856196, 40.89886208192143613 ) ) ;
#11536 = CARTESIAN_POINT ( 'NONE',  ( 86.59999999453762598, 168.7903194862797420, 4.480746418436729606 ) ) ;
#11537 = CARTESIAN_POINT ( 'NONE',  ( 7.456977232089302632, 217.1783343296989131, 76.55113791807858092 ) ) ;
#11538 = CARTESIAN_POINT ( 'NONE',  ( 4.984841277089725686, 213.7757310962907411, 94.55113791807855250 ) ) ;
#11539 = CARTESIAN_POINT ( 'NONE',  ( 6.220909254589681581, 198.5229672870052582, 55.44886208192141908 ) ) ;
#11540 = CARTESIAN_POINT ( 'NONE',  ( 1.306442393143578906, 8.377108146505383601, -7.792327460285857654 ) ) ;
#11541 = EDGE_LOOP ( 'NONE', ( #11419, #31297, #3660, #29620 ) ) ;
#11542 = CARTESIAN_POINT ( 'NONE',  ( 9.680171189290716072, 214.0920067884432854, 57.69886208192144039 ) ) ;
#11543 = VERTEX_POINT ( 'NONE', #18777 ) ;
#11544 = CARTESIAN_POINT ( 'NONE',  ( 73.77499999726882152, 169.8198683612136222, -4.815267126137197984 ) ) ;
#11545 = CARTESIAN_POINT ( 'NONE',  ( -8.015496119326597224, 209.5516654185217362, 41.64886208192143613 ) ) ;
#11546 = ORIENTED_EDGE ( 'NONE', *, *, #8965, .T. ) ;
#11547 = CARTESIAN_POINT ( 'NONE',  ( 85.47499999726881015, 160.0630714827496206, -15.58253175000000823 ) ) ;
#11548 = LINE ( 'NONE', #22276, #16219 ) ;
#11549 = LINE ( 'NONE', #24497, #26885 ) ;
#11550 = CARTESIAN_POINT ( 'NONE',  ( 4.984841277089725686, 213.7757310962907411, 49.55113791807858092 ) ) ;
#11551 = LINE ( 'NONE', #8995, #17786 ) ;
#11552 = CARTESIAN_POINT ( 'NONE',  ( -3.044812012439970683, 197.4746971517856196, 31.89886208192143613 ) ) ;
#11553 = CARTESIAN_POINT ( 'NONE',  ( 70.57499999726881867, 145.8408176439707802, 12.60653300113718345 ) ) ;
#11554 = ORIENTED_EDGE ( 'NONE', *, *, #29970, .T. ) ;
#11555 = PLANE ( 'NONE',  #6395 ) ;
#11556 = AXIS2_PLACEMENT_3D ( 'NONE', #25985, #15582, #16081 ) ;
#11557 = FILL_AREA_STYLE_COLOUR ( '', #2964 ) ;
#11558 = LINE ( 'NONE', #22113, #10699 ) ;
#11559 = LINE ( 'NONE', #29283, #19078 ) ;
#11560 = CARTESIAN_POINT ( 'NONE',  ( 2.426778023690075337, 214.6231898156240447, 12.39886208192143613 ) ) ;
#11561 = CARTESIAN_POINT ( 'NONE',  ( 6.139770520408368348, 198.4640165459539674, 59.45113791807855819 ) ) ;
#11562 = EDGE_CURVE ( 'NONE', #24712, #7575, #12971, .T. ) ;
#11563 = CARTESIAN_POINT ( 'NONE',  ( -6.139770520408369237, 215.5359834540460042, 39.95113791807857240 ) ) ;
#11564 = CARTESIAN_POINT ( 'NONE',  ( -98.16666666666678509, -61.33333333333321491, -13.66666666666659502 ) ) ;
#11565 = CARTESIAN_POINT ( 'NONE',  ( 6.444103211790928043, 211.7408657792734061, 99.69886208192144750 ) ) ;
#11566 = VECTOR ( 'NONE', #72, 1000.000000000000000 ) ;
#11567 = CARTESIAN_POINT ( 'NONE',  ( 46.42499999726880588, 141.7447067706911810, 9.630534252274376428 ) ) ;
#11568 = CARTESIAN_POINT ( 'NONE',  ( 35.98867513459482126, 146.1832212156128890, 12.13525491562421976 ) ) ;
#11569 = CARTESIAN_POINT ( 'NONE',  ( 110.1179863365115636, 155.0000000000000000, -32.10452846326764131 ) ) ;
#11570 = CARTESIAN_POINT ( 'NONE',  ( -0.05014649552807705357, 194.3824533091408000, 23.75113791807855890 ) ) ;
#11571 = CARTESIAN_POINT ( 'NONE',  ( -3.250000000000003997, -5.629165124598849879, 0.000000000000000000 ) ) ;
#11572 = CARTESIAN_POINT ( 'NONE',  ( 8.118202686958039038, 212.8392687619912635, 61.70113791807857240 ) ) ;
#11573 = CARTESIAN_POINT ( 'NONE',  ( 8.062137200540920645, 201.0835637161417822, 44.30113791807857382 ) ) ;
#11574 = CARTESIAN_POINT ( 'NONE',  ( 97.20416941062678973, 155.0000000000000000, 0.000000000000000000 ) ) ;
#11575 = CARTESIAN_POINT ( 'NONE',  ( -2.926493552096032680, -2.351840044243060923, -2.761158938895374337 ) ) ;
#11576 = CARTESIAN_POINT ( 'NONE',  ( 0.05014649552828288198, 194.3824533091408000, 7.748862081921433109 ) ) ;
#11577 = CARTESIAN_POINT ( 'NONE',  ( -10.00000000000000711, 206.9523078486584495, 5.498862081921434886 ) ) ;
#11578 = CARTESIAN_POINT ( 'NONE',  ( 63.99999999453763166, 155.0000000000000000, -14.50000000000000711 ) ) ;
#11579 = EDGE_LOOP ( 'NONE', ( #19660, #15278, #19292, #18626, #21013, #14385 ) ) ;
#11580 = CARTESIAN_POINT ( 'NONE',  ( -7.375838497908182134, 217.2372850707499765, 51.95113791807855819 ) ) ;
#11581 = CARTESIAN_POINT ( 'NONE',  ( -6.444103211791042618, 211.7408657792732356, 66.80113791807858092 ) ) ;
#11582 = DIRECTION ( 'NONE',  ( 0.000000000000000000, 0.000000000000000000, -1.000000000000000000 ) ) ;
#11583 = CARTESIAN_POINT ( 'NONE',  ( -8.062137200540822946, 201.0835637161416400, 29.19886208192143684 ) ) ;
#11584 = CARTESIAN_POINT ( 'NONE',  ( 32.50000000000000000, 155.0000000000000000, -6.938893903907228378E-15 ) ) ;
#11585 = ORIENTED_EDGE ( 'NONE', *, *, #26380, .T. ) ;
#11586 = CIRCLE ( 'NONE', #30635, 2.149999999999984812 ) ;
#11587 = CARTESIAN_POINT ( 'NONE',  ( -6.139770520408369237, 215.5359834540460042, 81.95113791807854398 ) ) ;
#11588 = ORIENTED_EDGE ( 'NONE', *, *, #28872, .F. ) ;
#11589 = LINE ( 'NONE', #6646, #448 ) ;
#11590 = CARTESIAN_POINT ( 'NONE',  ( -2.075968632161005800, -6.306992450858350807, -6.056431503346042078 ) ) ;
#11591 = ORIENTED_EDGE ( 'NONE', *, *, #24948, .T. ) ;
#11592 = CARTESIAN_POINT ( 'NONE',  ( -4.903702542908602524, 213.8346818373418898, 18.95113791807856529 ) ) ;
#11593 = EDGE_CURVE ( 'NONE', #5005, #2969, #728, .T. ) ;
#11594 = VECTOR ( 'NONE', #14899, 1000.000000000000000 ) ;
#11595 = LINE ( 'NONE', #3919, #14515 ) ;
#11596 = CARTESIAN_POINT ( 'NONE',  ( -12.05084501415679199, 219.7456114157811271, 104.9910338291041114 ) ) ;
#11597 = AXIS2_PLACEMENT_3D ( 'NONE', #33182, #6947, #4212 ) ;
#11598 = CARTESIAN_POINT ( 'NONE',  ( 49.57499999726881157, 164.1591823560292198, -12.60653300113719766 ) ) ;
#11599 = ORIENTED_EDGE ( 'NONE', *, *, #335, .T. ) ;
#11600 = CARTESIAN_POINT ( 'NONE',  ( 59.32499999726881157, 164.1591823560292198, -12.60653300113719766 ) ) ;
#11601 = CARTESIAN_POINT ( 'NONE',  ( -0.05014649552807731031, 198.5883022060938572, 47.75113791807856245 ) ) ;
#11602 = CARTESIAN_POINT ( 'NONE',  ( 4.000000000000000000, 3.518949890710768802, -4.770489558936219510E-15 ) ) ;
#11603 = CARTESIAN_POINT ( 'NONE',  ( 115.4999999999999858, 102.0000000000001990, 93.94869280115062793 ) ) ;
#11604 = CARTESIAN_POINT ( 'NONE',  ( 6.220909254589681581, 198.5229672870052582, 91.44886208192143329 ) ) ;
#11605 = CARTESIAN_POINT ( 'NONE',  ( 62.77499999726882152, 140.1801316387863778, 4.815267126137185549 ) ) ;
#11606 = CARTESIAN_POINT ( 'NONE',  ( -10.00000000000000711, 207.0476921513413515, 33.50113791807856956 ) ) ;
#11607 = CARTESIAN_POINT ( 'NONE',  ( 73.68867513459484542, 159.8737954434932647, 15.00000000000027001 ) ) ;
#11608 = EDGE_CURVE ( 'NONE', #18797, #24401, #25782, .T. ) ;
#11609 = CARTESIAN_POINT ( 'NONE',  ( 9.680171189290716072, 214.0920067884432854, 81.69886208192144750 ) ) ;
#11610 = AXIS2_PLACEMENT_3D ( 'NONE', #33649, #20701, #10329 ) ;
#11611 = CARTESIAN_POINT ( 'NONE',  ( 82.10000000000000853, 141.2096805137202580, -4.480746418436742040 ) ) ;
#11612 = LINE ( 'NONE', #18779, #30121 ) ;
#11613 = CYLINDRICAL_SURFACE ( 'NONE', #31649, 98.00000000000000000 ) ;
#11614 =( GEOMETRIC_REPRESENTATION_CONTEXT ( 3 ) GLOBAL_UNCERTAINTY_ASSIGNED_CONTEXT ( ( #19636 ) ) GLOBAL_UNIT_ASSIGNED_CONTEXT ( ( #22758, #7086, #9814 ) ) REPRESENTATION_CONTEXT ( 'NONE', 'WORKASPACE' ) );
#11615 = CARTESIAN_POINT ( 'NONE',  ( 8.118202686958039038, 212.8392687619912635, 97.70113791807857240 ) ) ;
#11616 = DIRECTION ( 'NONE',  ( 0.000000000000000000, 0.000000000000000000, 1.000000000000000000 ) ) ;
#11617 = CARTESIAN_POINT ( 'NONE',  ( 41.47499999726880304, 160.0630714827496206, -15.58253175000000823 ) ) ;
#11618 = CARTESIAN_POINT ( 'NONE',  ( -6.220909254589537696, 198.5229672870051161, 42.05113791807857382 ) ) ;
#11619 =( REPRESENTATION_RELATIONSHIP ('NONE','NONE', #25663, #22175 ) REPRESENTATION_RELATIONSHIP_WITH_TRANSFORMATION ( #27399 )SHAPE_REPRESENTATION_RELATIONSHIP( ) );
#11620 = CARTESIAN_POINT ( 'NONE',  ( 79.52499999726880731, 169.8198683612136222, -4.815267126137197984 ) ) ;
#11621 = EDGE_CURVE ( 'NONE', #14265, #33504, #28487, .T. ) ;
#11622 = ORIENTED_EDGE ( 'NONE', *, *, #32787, .T. ) ;
#11623 = CARTESIAN_POINT ( 'NONE',  ( -2.623433461001184686, 7.604994000793856124, -7.633824513837113912 ) ) ;
#11624 = CARTESIAN_POINT ( 'NONE',  ( 5.000000000000000000, -2.342598717236903383, 4.057500000000001883 ) ) ;
#11625 = AXIS2_PLACEMENT_3D ( 'NONE', #7172, #2062, #2229 ) ;
#11626 = CARTESIAN_POINT ( 'NONE',  ( 48.19999999453762740, 163.5228861582408797, -11.73074641843674470 ) ) ;
#11627 = CARTESIAN_POINT ( 'NONE',  ( 7.375838497908181246, 196.7627149292499666, 20.45113791807856529 ) ) ;
#11628 = CIRCLE ( 'NONE', #15974, 2.149999999999994138 ) ;
#11629 = CYLINDRICAL_SURFACE ( 'NONE', #3929, 8.000000000000000000 ) ;
#11630 = CIRCLE ( 'NONE', #6737, 12.00000000000000355 ) ;
#11631 = CARTESIAN_POINT ( 'NONE',  ( -66.50402289005056389, 121.5305141831588003, 17.99597710994943967 ) ) ;
#11632 = B_SPLINE_CURVE_WITH_KNOTS ( 'NONE', 3,
 ( #1467, #20031, #30431, #7091, #14580, #22761 ),
 .UNSPECIFIED., .F., .F.,
 ( 4, 2, 4 ),
 ( 0.000000000000000000, 0.0003352299596252128282, 0.0006704599192504256564 ),
 .UNSPECIFIED. ) ;
#11633 = ORIENTED_EDGE ( 'NONE', *, *, #14919, .T. ) ;
#11634 = CARTESIAN_POINT ( 'NONE',  ( -11.98450388067341876, 203.0532714938636047, 47.34886208192143897 ) ) ;
#11635 = CARTESIAN_POINT ( 'NONE',  ( -10.00000000000000711, 207.0476921513413515, 0.5011379180785656695 ) ) ;
#11636 = CARTESIAN_POINT ( 'NONE',  ( -10.01549611932653860, 203.7984951890123284, 54.35113791807856387 ) ) ;
#11637 = ADVANCED_FACE ( 'NONE', ( #713 ), #8877, .F. ) ;
#11638 = CARTESIAN_POINT ( 'NONE',  ( -4.984841277089891776, 213.7757310962905990, 11.94886208192143506 ) ) ;
#11639 = FACE_OUTER_BOUND ( 'NONE', #29563, .T. ) ;
#11640 = VERTEX_POINT ( 'NONE', #22159 ) ;
#11641 = CARTESIAN_POINT ( 'NONE',  ( -2.517493886309087880, 214.5937144450984135, 99.09886208192145318 ) ) ;
#11642 = EDGE_CURVE ( 'NONE', #19014, #26053, #30760, .T. ) ;
#11643 = DIRECTION ( 'NONE',  ( 1.000000000000000000, 0.000000000000000000, 0.000000000000000000 ) ) ;
#11644 = CARTESIAN_POINT ( 'NONE',  ( -0.05014649552807731031, 198.5883022060938572, 44.75113791807857666 ) ) ;
#11645 = DIRECTION ( 'NONE',  ( -0.2649168722799636333, 0.9642688156137663169, -0.002168413296789690158 ) ) ;
#11646 = EDGE_LOOP ( 'NONE', ( #4380, #10243, #22646 ) ) ;
#11647 = CARTESIAN_POINT ( 'NONE',  ( 36.32499999726881157, 145.8408176439707802, 12.60653300113718345 ) ) ;
#11648 = AXIS2_PLACEMENT_3D ( 'NONE', #3936, #22846, #11951 ) ;
#11649 = CARTESIAN_POINT ( 'NONE',  ( -10.01549611932659722, 210.2015048109875011, 62.64886208192143613 ) ) ;
#11650 = AXIS2_PLACEMENT_3D ( 'NONE', #29778, #16150, #3540 ) ;
#11651 = CARTESIAN_POINT ( 'NONE',  ( 41.07499999726881157, 141.7447067706911810, -9.630534252274385310 ) ) ;
#11652 = DIRECTION ( 'NONE',  ( 0.000000000000000000, 0.000000000000000000, -1.000000000000000000 ) ) ;
#11653 = CARTESIAN_POINT ( 'NONE',  ( 6.444103211791042618, 202.2591342207267644, 95.30113791807858092 ) ) ;
#11654 = CARTESIAN_POINT ( 'NONE',  ( 52.20000000000000284, 142.6655632788954620, -8.961492836873480528 ) ) ;
#11655 = CARTESIAN_POINT ( 'NONE',  ( 62.98867513459482836, 163.8167787843871110, -12.13525491562423397 ) ) ;
#11656 = CARTESIAN_POINT ( 'NONE',  ( -6.444103211790928043, 202.2591342207265939, 80.19886208192143329 ) ) ;
#11657 = CARTESIAN_POINT ( 'NONE',  ( -2.837346585668847787, 6.232092946297378866, -6.171287963165196899 ) ) ;
#11658 = DIRECTION ( 'NONE',  ( 0.000000000000000000, 1.000000000000000000, -3.227392513445244800E-15 ) ) ;
#11659 = CARTESIAN_POINT ( 'NONE',  ( 57.82499999726879736, 168.2552932293087906, 9.630534252274372875 ) ) ;
#11661 = ORIENTED_EDGE ( 'NONE', *, *, #27899, .F. ) ;
#11660 = CARTESIAN_POINT ( 'NONE',  ( -10.00000000000000711, 207.0476921513413515, 21.50113791807856956 ) ) ;
#11662 = DIRECTION ( 'NONE',  ( -0.000000000000000000, -0.000000000000000000, 1.000000000000000000 ) ) ;
#11663 = CARTESIAN_POINT ( 'NONE',  ( 83.67499999726884141, 168.2552932293087906, -9.630534252274385310 ) ) ;
#11664 = CARTESIAN_POINT ( 'NONE',  ( -3.753561863808691168, 195.6020594897209435, 83.90113791807856103 ) ) ;
#11665 = ADVANCED_FACE ( 'NONE', ( #4098 ), #32716, .T. ) ;
#11666 = ADVANCED_FACE ( 'NONE', ( #33232 ), #15001, .T. ) ;
#11667 = CARTESIAN_POINT ( 'NONE',  ( 127.5000000000000000, 155.0000000000000000, -100.0000000000000284 ) ) ;
#11668 = DIRECTION ( 'NONE',  ( -1.000000000000000000, -1.804112415015879625E-16, -0.000000000000000000 ) ) ;
#11669 = ORIENTED_EDGE ( 'NONE', *, *, #2897, .F. ) ;
#11670 = CARTESIAN_POINT ( 'NONE',  ( 9.736236675708031640, 199.9851607334238963, 64.29886208192144181 ) ) ;
#11671 = CARTESIAN_POINT ( 'NONE',  ( 10.00000000000000711, 207.0476921513415220, 75.99886208192144466 ) ) ;
#11672 = CARTESIAN_POINT ( 'NONE',  ( 9.680171189290716072, 214.0920067884432854, 12.69886208192143684 ) ) ;
#11673 = PLANE ( 'NONE',  #10499 ) ;
#11674 = CARTESIAN_POINT ( 'NONE',  ( -8.062137200540920645, 212.9164362838581894, 21.80113791807856671 ) ) ;
#11675 = EDGE_CURVE ( 'NONE', #17109, #317, #27906, .T. ) ;
#11676 = CARTESIAN_POINT ( 'NONE',  ( 6.220909254589681581, 198.5229672870052582, 91.44886208192143329 ) ) ;
#11677 = ORIENTED_EDGE ( 'NONE', *, *, #24757, .T. ) ;
#11678 = DIRECTION ( 'NONE',  ( -1.000000000000000000, 0.000000000000000000, 0.000000000000000000 ) ) ;
#11679 = ORIENTED_EDGE ( 'NONE', *, *, #2441, .F. ) ;
#11680 = CARTESIAN_POINT ( 'NONE',  ( 42.49999999999998579, 9.830099697201894772E-15, 20.00000000000000000 ) ) ;
#11681 = CARTESIAN_POINT ( 'NONE',  ( -2.517493886309087880, 214.5937144450984135, 75.09886208192142476 ) ) ;
#11682 = ADVANCED_FACE ( 'NONE', ( #19611 ), #9549, .F. ) ;
#11683 = EDGE_LOOP ( 'NONE', ( #6257, #15909, #33420, #27256, #3704, #28135, #4969 ) ) ;
#11684 = CARTESIAN_POINT ( 'NONE',  ( 85.02499999726880731, 149.9369285172503510, -15.58253175000000823 ) ) ;
#11685 = EDGE_LOOP ( 'NONE', ( #7801, #21064, #7706, #12262 ) ) ;
#11686 = CARTESIAN_POINT ( 'NONE',  ( 69.61132485994282604, 150.1262045565062806, -14.99999999999993072 ) ) ;
#11687 = PRESENTATION_LAYER_ASSIGNMENT (  '', '', ( #245 ) ) ;
#11688 = CARTESIAN_POINT ( 'NONE',  ( 74.42499999726881299, 141.7447067706911810, 9.630534252274376428 ) ) ;
#11689 = DIRECTION ( 'NONE',  ( 0.000000000000000000, 0.000000000000000000, -1.000000000000000000 ) ) ;
#11690 = CARTESIAN_POINT ( 'NONE',  ( 4.903702542908601636, 200.1653181626581102, 65.45113791807858661 ) ) ;
#11691 = CARTESIAN_POINT ( 'NONE',  ( -3.499999999999999112, 0.6879904500768373454, -2.869836757075878708 ) ) ;
#11692 =( NAMED_UNIT ( * ) SI_UNIT ( $, .STERADIAN. ) SOLID_ANGLE_UNIT ( ) );
#11693 = CARTESIAN_POINT ( 'NONE',  ( 34.30000000000000426, 146.4771138417591203, -11.73074641843674470 ) ) ;
#11694 = CARTESIAN_POINT ( 'NONE',  ( -4.984841277089891776, 213.7757310962905990, 41.94886208192144750 ) ) ;
#11695 = CARTESIAN_POINT ( 'NONE',  ( -3.044812012440131443, 216.5253028482142952, 76.10113791807856387 ) ) ;
#11696 = CARTESIAN_POINT ( 'NONE',  ( 78.00000000000001421, 0.000000000000000000, 0.000000000000000000 ) ) ;
#11697 = LINE ( 'NONE', #14922, #32026 ) ;
#11698 = CARTESIAN_POINT ( 'NONE',  ( 78.00000000000001421, 0.000000000000000000, 3.309499999999999886 ) ) ;
#11699 = CARTESIAN_POINT ( 'NONE',  ( 52.72499999726881015, 140.1801316387863778, -4.815267126137194431 ) ) ;
#11700 = CARTESIAN_POINT ( 'NONE',  ( 0.05014649552807549926, 219.6175466908591716, 58.25113791807856245 ) ) ;
#11701 = DIRECTION ( 'NONE',  ( 0.000000000000000000, 0.000000000000000000, -1.000000000000000000 ) ) ;
#11702 = CARTESIAN_POINT ( 'NONE',  ( -7.456977232089304408, 196.8216656703010301, 3.051137918078566269 ) ) ;
#11703 = CARTESIAN_POINT ( 'NONE',  ( 3.135527875058820690, 216.4958274776887492, 64.40113791807857524 ) ) ;
#11704 = CARTESIAN_POINT ( 'NONE',  ( -3.753561863808878130, 218.3979405102790281, 33.09886208192143187 ) ) ;
#11705 = CARTESIAN_POINT ( 'NONE',  ( 10.00000000000000711, 207.0476921513415220, 51.99886208192143755 ) ) ;
#11706 = CARTESIAN_POINT ( 'NONE',  ( 84.69999999453763451, 167.3344367211045096, 8.961492836873468093 ) ) ;
#11707 = CARTESIAN_POINT ( 'NONE',  ( -9.736236675707914401, 199.9851607334237542, 75.20113791807857240 ) ) ;
#11708 = CARTESIAN_POINT ( 'NONE',  ( -8.000000000000008882, 207.0476921513413515, 96.50113791807856956 ) ) ;
#11709 = CARTESIAN_POINT ( 'NONE',  ( 8.062137200540822946, 212.9164362838583315, 57.69886208192144039 ) ) ;
#11710 = DIRECTION ( 'NONE',  ( 0.000000000000000000, 0.000000000000000000, -1.000000000000000000 ) ) ;
#11711 = ORIENTED_EDGE ( 'NONE', *, *, #2875, .F. ) ;
#11712 = CARTESIAN_POINT ( 'NONE',  ( 11.98450388067341876, 210.9467285061363953, 63.84886208192143187 ) ) ;
#11713 = ORIENTED_EDGE ( 'NONE', *, *, #31268, .F. ) ;
#11714 = CARTESIAN_POINT ( 'NONE',  ( 74.77499999726880731, 140.1801316387863778, 4.815267126137185549 ) ) ;
#11715 = CARTESIAN_POINT ( 'NONE',  ( -6.500168698208244500, 211.6636982574061676, 38.79886208192143471 ) ) ;
#11716 = ORIENTED_EDGE ( 'NONE', *, *, #2237, .F. ) ;
#11717 = CARTESIAN_POINT ( 'NONE',  ( 82.37499999726881583, 155.0000000000000000, 15.58253174999999402 ) ) ;
#11718 = PLANE ( 'NONE',  #7543 ) ;
#11719 = CARTESIAN_POINT ( 'NONE',  ( 1.750000000000012879, 3.031088913245524097, 1.502314598737187430E-15 ) ) ;
#11720 = CARTESIAN_POINT ( 'NONE',  ( 4.984841277089725686, 213.7757310962907411, 52.55113791807858092 ) ) ;
#11721 = CARTESIAN_POINT ( 'NONE',  ( -5.000000000000000888, 6.123233995736767268E-16, -10.00000000000000000 ) ) ;
#11722 = CARTESIAN_POINT ( 'NONE',  ( -10.00000000000000711, 206.9523078486584495, 32.49886208192143044 ) ) ;
#11723 = CARTESIAN_POINT ( 'NONE',  ( 71.47499999726881015, 160.0630714827496206, -15.58253175000000823 ) ) ;
#11724 = ORIENTED_EDGE ( 'NONE', *, *, #25101, .F. ) ;
#11725 = DIRECTION ( 'NONE',  ( 0.000000000000000000, 0.000000000000000000, 1.000000000000000000 ) ) ;
#11726 = CARTESIAN_POINT ( 'NONE',  ( 110.1179863365115636, 155.0000000000000000, 0.000000000000000000 ) ) ;
#11727 =( BOUNDED_CURVE ( )  B_SPLINE_CURVE ( 2, ( #15389, #23890, #17956, #5497, #31561, #20836, #12834, #28346, #23724, #2789, #26442 ),
 .UNSPECIFIED., .F., .T. ) 
 B_SPLINE_CURVE_WITH_KNOTS ( ( 3, 2, 2, 2, 2, 3 ),
 ( 0.5357142857142856984, 0.5392857142857143682, 0.5428571428571428159, 0.5464285714285713746, 0.5499999999999998224, 0.5535714285714284921 ),
 .UNSPECIFIED. ) 
 CURVE ( )  GEOMETRIC_REPRESENTATION_ITEM ( )  RATIONAL_B_SPLINE_CURVE ( ( 0.9999999999999984457, 0.9510565162951549745, 1.000000000000000000, 0.9510565162951534202, 1.000000000000000000, 0.9510565162951534202, 1.000000000000000000, 0.9510565162951534202, 1.000000000000000000, 0.9510565162951549745, 0.9999999999999984457 ) ) 
 REPRESENTATION_ITEM ( '' )  );
#11728 = CARTESIAN_POINT ( 'NONE',  ( 6.500168698208244500, 202.3363017425938324, 13.29886208192143826 ) ) ;
#11729 = CARTESIAN_POINT ( 'NONE',  ( -8.062137200540920645, 212.9164362838581894, 57.80113791807857382 ) ) ;
#11730 = CARTESIAN_POINT ( 'NONE',  ( -10.00000000000000711, 207.0476921513413515, 48.50113791807856956 ) ) ;
#11731 = CARTESIAN_POINT ( 'NONE',  ( 38.11132485994280472, 169.2658477444273331, -4.635254915624224203 ) ) ;
#11732 = CARTESIAN_POINT ( 'NONE',  ( 2.517493886309087436, 199.4062855549015865, 100.5988620819214532 ) ) ;
#11733 = CARTESIAN_POINT ( 'NONE',  ( 44.02499999726881441, 160.0630714827496206, 15.58253174999999402 ) ) ;
#11734 = SURFACE_SIDE_STYLE ('',( #12070 ) ) ;
#11735 = CARTESIAN_POINT ( 'NONE',  ( 34.22499999726881015, 149.9369285172503510, 15.58253174999999580 ) ) ;
#11736 = CARTESIAN_POINT ( 'NONE',  ( 9.736236675707914401, 214.0148392665762458, 22.70113791807856529 ) ) ;
#11737 = LINE ( 'NONE', #12073, #456 ) ;
#11738 = CARTESIAN_POINT ( 'NONE',  ( -8.118202686958039038, 201.1607312380087080, 66.20113791807857240 ) ) ;
#11739 = CARTESIAN_POINT ( 'NONE',  ( 9.984503880673473830, 203.7031108863295401, 35.15113791807856103 ) ) ;
#11740 = LINE ( 'NONE', #16850, #25771 ) ;
#11741 = LINE ( 'NONE', #6632, #12509 ) ;
#11742 = CARTESIAN_POINT ( 'NONE',  ( -12.00000000000000711, 206.9523078486584780, 2.498862081921434442 ) ) ;
#11743 = CARTESIAN_POINT ( 'NONE',  ( 6.220909254589680693, 198.5229672870052582, 19.44886208192143329 ) ) ;
#11744 = CARTESIAN_POINT ( 'NONE',  ( 65.79999999453762882, 146.4771138417591203, -11.73074641843674470 ) ) ;
#11745 = ORIENTED_EDGE ( 'NONE', *, *, #16858, .F. ) ;
#11746 = CARTESIAN_POINT ( 'NONE',  ( -12.00000000000000711, 207.0476921513413515, 51.50113791807856956 ) ) ;
#11747 = CARTESIAN_POINT ( 'NONE',  ( 0.05014649552807626948, 215.4116977939061144, 73.25113791807858377 ) ) ;
#11748 = CARTESIAN_POINT ( 'NONE',  ( -8.118202686958138514, 212.8392687619910930, 29.79886208192143826 ) ) ;
#11749 = CARTESIAN_POINT ( 'NONE',  ( 94.70964751525852421, 155.0000000000000000, 0.000000000000000000 ) ) ;
#11750 = EDGE_LOOP ( 'NONE', ( #6035, #32497, #2425, #10019, #16643, #33461 ) ) ;
#11751 = B_SPLINE_CURVE_WITH_KNOTS ( 'NONE', 3,
 ( #23035, #25592, #33432, #9412, #6693, #2091 ),
 .UNSPECIFIED., .F., .F.,
 ( 4, 2, 4 ),
 ( 0.003841072314098362400, 0.005765657563962184665, 0.007690242813826007363 ),
 .UNSPECIFIED. ) ;
#11752 = CARTESIAN_POINT ( 'NONE',  ( -6.220909254589537696, 198.5229672870051161, 90.05113791807858092 ) ) ;
#11753 = ORIENTED_EDGE ( 'NONE', *, *, #22218, .T. ) ;
#11754 = EDGE_CURVE ( 'NONE', #8526, #20186, #25135, .T. ) ;
#11755 = CARTESIAN_POINT ( 'NONE',  ( 41.88867513459481984, 150.1262045565064227, 15.00000000000001599 ) ) ;
#11756 = DIRECTION ( 'NONE',  ( -0.000000000000000000, -0.000000000000000000, 1.000000000000000000 ) ) ;
#11757 = VERTEX_POINT ( 'NONE', #30003 ) ;
#11758 = CARTESIAN_POINT ( 'NONE',  ( -8.015496119326531499, 204.4483345814780364, 27.35113791807856742 ) ) ;
#11759 = CARTESIAN_POINT ( 'NONE',  ( 54.71132485994280614, 155.0000000000000000, 15.00000000000001243 ) ) ;
#11760 = CARTESIAN_POINT ( 'NONE',  ( 6.139770520408223575, 215.5359834540460611, 3.548862081921434708 ) ) ;
#11761 = CARTESIAN_POINT ( 'NONE',  ( 53.17499999726881299, 145.8408176439707802, -12.60653300113719588 ) ) ;
#11762 = ORIENTED_EDGE ( 'NONE', *, *, #36, .F. ) ;
#11763 = CARTESIAN_POINT ( 'NONE',  ( 2.426778023690261410, 199.3768101843759837, 50.60113791807857808 ) ) ;
#11764 = DIRECTION ( 'NONE',  ( -1.000000000000000000, -0.000000000000000000, -0.000000000000000000 ) ) ;
#11765 = PLANE ( 'NONE',  #22796 ) ;
#11766 = CARTESIAN_POINT ( 'NONE',  ( -9.984503880673420539, 203.7031108863293980, 95.34886208192142476 ) ) ;
#11767 = CARTESIAN_POINT ( 'NONE',  ( 57.77499999726881441, 169.8198683612136222, -4.815267126137197984 ) ) ;
#11768 = CARTESIAN_POINT ( 'NONE',  ( 10.01549611932653860, 210.2015048109876716, 34.85113791807856387 ) ) ;
#11769 = CARTESIAN_POINT ( 'NONE',  ( 47.78867513459482552, 155.0000000000000000, 15.00000000000001243 ) ) ;
#11770 = CARTESIAN_POINT ( 'NONE',  ( -9.736236675708031640, 214.0148392665760753, 83.79886208192144181 ) ) ;
#11771 = DIRECTION ( 'NONE',  ( 1.000000000000000000, 0.000000000000000000, 0.000000000000000000 ) ) ;
#11772 = CLOSED_SHELL ( 'NONE', ( #18079, #27087, #21142, #22058, #6682, #26397, #27829, #33652, #9786, #21999, #32866, #3507, #5211, #3964, #3067, #32908, #15630, #21251, #7414, #29482, #24072, #24988, #10359, #32698, #25918, #19539, #5554, #446, #16648, #10590, #18101, #24098, #9599 ) ) ;
#11773 = CARTESIAN_POINT ( 'NONE',  ( 80.69999999999998863, 163.5228861582408797, -11.73074641843674470 ) ) ;
#11774 = CARTESIAN_POINT ( 'NONE',  ( -52.50000000000002132, 155.0000000000000000, 6.999999999999944045 ) ) ;
#11775 = DIRECTION ( 'NONE',  ( 0.000000000000000000, 0.9963496021943381020, -0.08536668089591059605 ) ) ;
#11776 = CARTESIAN_POINT ( 'NONE',  ( -10.00000000000000711, 207.0476921513413515, 93.50113791807858377 ) ) ;
#11777 = CARTESIAN_POINT ( 'NONE',  ( 13.75000000000000888, -23.81569860407206463, 0.000000000000000000 ) ) ;
#11778 = CARTESIAN_POINT ( 'NONE',  ( 42.37499999726881583, 155.0000000000000000, 15.58253174999999402 ) ) ;
#11779 = CARTESIAN_POINT ( 'NONE',  ( -3.135527875058821579, 197.5041725223112223, 35.90113791807856813 ) ) ;
#11780 = B_SPLINE_CURVE_WITH_KNOTS ( 'NONE', 3,
 ( #1693, #22310, #6295, #3751, #25040, #16689, #29817, #17196 ),
 .UNSPECIFIED., .F., .F.,
 ( 4, 2, 2, 4 ),
 ( 2.459764730742321679E-07, 0.001920659145285711104, 0.002880865729692028403, 0.003841072314098346787 ),
 .UNSPECIFIED. ) ;
#11781 = AXIS2_PLACEMENT_3D ( 'NONE', #25343, #20068, #4218 ) ;
#11782 = CARTESIAN_POINT ( 'NONE',  ( 80.42499999726879878, 141.7447067706911810, 9.630534252274376428 ) ) ;
#11783 = DIRECTION ( 'NONE',  ( 0.000000000000000000, 0.000000000000000000, -1.000000000000000000 ) ) ;
#11784 = DIRECTION ( 'NONE',  ( 0.000000000000000000, 0.000000000000000000, 1.000000000000000000 ) ) ;
#11785 = CARTESIAN_POINT ( 'NONE',  ( 45.59999999453762598, 141.2096805137202580, -4.480746418436742040 ) ) ;
#11786 = ORIENTED_EDGE ( 'NONE', *, *, #744, .T. ) ;
#11787 = CARTESIAN_POINT ( 'NONE',  ( 7.456977232089302632, 217.1783343296989131, 16.55113791807857027 ) ) ;
#11788 = CARTESIAN_POINT ( 'NONE',  ( 66.31132485994281467, 169.2658477444273331, 4.635254915624208216 ) ) ;
#11789 = ORIENTED_EDGE ( 'NONE', *, *, #12023, .T. ) ;
#11790 = CARTESIAN_POINT ( 'NONE',  ( -3.662846001189865142, 195.5725841191952838, 40.89886208192143613 ) ) ;
#11791 = CARTESIAN_POINT ( 'NONE',  ( -9.984503880673473830, 210.2968891136704315, 0.6511379180785656917 ) ) ;
#11792 = CARTESIAN_POINT ( 'NONE',  ( 6.220909254589536808, 215.4770327129947702, 58.55113791807858092 ) ) ;
#11793 = CARTESIAN_POINT ( 'NONE',  ( -8.015496119326597224, 209.5516654185217362, 17.64886208192143968 ) ) ;
#11794 = ADVANCED_FACE ( 'NONE', ( #27445 ), #24888, .F. ) ;
#11795 = VECTOR ( 'NONE', #30104, 999.9999999999998863 ) ;
#11796 = STYLED_ITEM ( 'NONE', ( #23501 ), #619 ) ;
#11797 = UNCERTAINTY_MEASURE_WITH_UNIT (LENGTH_MEASURE( 1.000000000000000082E-05 ), #22406, 'distance_accuracy_value', 'NONE');
#11798 = DIRECTION ( 'NONE',  ( 0.000000000000000000, 0.000000000000000000, -1.000000000000000000 ) ) ;
#11799 = ORIENTED_EDGE ( 'NONE', *, *, #8695, .T. ) ;
#11800 = CARTESIAN_POINT ( 'NONE',  ( -4.984841277089891776, 213.7757310962905990, 101.9488620819214475 ) ) ;
#11801 = EDGE_CURVE ( 'NONE', #17505, #15312, #24728, .T. ) ;
#11802 = LINE ( 'NONE', #22191, #21394 ) ;
#11803 = CARTESIAN_POINT ( 'NONE',  ( -0.05014649552807731031, 198.5883022060938572, 35.75113791807857666 ) ) ;
#11804 = DIRECTION ( 'NONE',  ( -1.000000000000000000, 0.000000000000000000, 0.000000000000000000 ) ) ;
#11806 = EDGE_LOOP ( 'NONE', ( #29369, #7928, #25003, #31462 ) ) ;
#11805 = AXIS2_PLACEMENT_3D ( 'NONE', #9976, #20699, #23252 ) ;
#11807 = CARTESIAN_POINT ( 'NONE',  ( 36.72499999726881015, 140.1801316387863778, -4.815267126137194431 ) ) ;
#11808 = DIRECTION ( 'NONE',  ( 1.000000000000000000, 0.000000000000000000, 0.000000000000000000 ) ) ;
#11809 = ADVANCED_FACE ( 'NONE', ( #25565 ), #10005, .T. ) ;
#11810 = CARTESIAN_POINT ( 'NONE',  ( -10.01549611932653860, 203.7984951890123284, 0.3511379180785655363 ) ) ;
#11811 = CARTESIAN_POINT ( 'NONE',  ( 10.01549611932659545, 203.7984951890123853, 58.14886208192142192 ) ) ;
#11812 = CARTESIAN_POINT ( 'NONE',  ( 43.37499999726881583, 155.0000000000000000, -15.58253175000000823 ) ) ;
#11813 = FACE_BOUND ( 'NONE', #19756, .T. ) ;
#11814 = CARTESIAN_POINT ( 'NONE',  ( 8.062137200540920645, 201.0835637161417822, 5.301137918078566713 ) ) ;
#11815 = APPLICATION_CONTEXT ( 'automotive_design' ) ;
#11816 = CARTESIAN_POINT ( 'NONE',  ( 60.30000000000000426, 146.4771138417591203, -11.73074641843674470 ) ) ;
#11817 = CARTESIAN_POINT ( 'NONE',  ( 62.88867513459482694, 159.8737954434937478, -14.99999999999993072 ) ) ;
#11818 = CARTESIAN_POINT ( 'NONE',  ( 8.015496119326595448, 204.4483345814782638, 79.14886208192143613 ) ) ;
#11819 = VECTOR ( 'NONE', #27769, 1000.000000000000000 ) ;
#11820 = CARTESIAN_POINT ( 'NONE',  ( 76.98867513459481415, 163.8167787843871110, -12.13525491562423397 ) ) ;
#11821 = DIRECTION ( 'NONE',  ( -0.9998603841633338929, 0.01669062914075312987, 0.0007969188393214247284 ) ) ;
#11822 = EDGE_CURVE ( 'NONE', #32913, #5506, #7276, .T. ) ;
#11823 = CARTESIAN_POINT ( 'NONE',  ( 66.32499999726881867, 145.8408176439707802, 12.60653300113718345 ) ) ;
#11824 = CIRCLE ( 'NONE', #14542, 6.099999999999999645 ) ;
#11826 = VERTEX_POINT ( 'NONE', #1549 ) ;
#11825 = CARTESIAN_POINT ( 'NONE',  ( 6.139770520408367460, 198.4640165459539389, 23.45113791807856884 ) ) ;
#11827 = DIRECTION ( 'NONE',  ( -1.000000000000000000, 0.000000000000000000, 0.000000000000000000 ) ) ;
#11828 = MANIFOLD_SOLID_BREP ( 'Revolve1', #6889 ) ;
#11829 = CARTESIAN_POINT ( 'NONE',  ( 85.17499999726882720, 145.8408176439707802, -12.60653300113719588 ) ) ;
#11830 = CARTESIAN_POINT ( 'NONE',  ( 0.05014649552807549926, 219.6175466908591716, 88.25113791807856956 ) ) ;
#11831 = ADVANCED_FACE ( 'NONE', ( #8184 ), #6831, .F. ) ;
#11832 = DIRECTION ( 'NONE',  ( 0.000000000000000000, -0.7071067811865506814, -0.7071067811865442421 ) ) ;
#11833 = VECTOR ( 'NONE', #8426, 1000.000000000000000 ) ;
#11834 = ORIENTED_EDGE ( 'NONE', *, *, #8744, .F. ) ;
#11835 = CARTESIAN_POINT ( 'NONE',  ( -7.375838497908014268, 196.7627149292498530, 68.04886208192144181 ) ) ;
#11836 = CARTESIAN_POINT ( 'NONE',  ( -3.135527875058982783, 216.4958274776886924, 81.09886208192143897 ) ) ;
#11837 = CARTESIAN_POINT ( 'NONE',  ( 12.01549611932659367, 203.1486557965466773, 13.14886208192143613 ) ) ;
#11838 = FACE_OUTER_BOUND ( 'NONE', #30847, .T. ) ;
#11839 = CARTESIAN_POINT ( 'NONE',  ( 10.01549611932653860, 210.2015048109876716, 19.85113791807856387 ) ) ;
#11840 = CARTESIAN_POINT ( 'NONE',  ( -3.755786496842903988E-16, -7.505553499465146494, -6.064240316920404439 ) ) ;
#11841 = CARTESIAN_POINT ( 'NONE',  ( -3.135527875058982783, 216.4958274776886924, 87.09886208192143897 ) ) ;
#11842 = CARTESIAN_POINT ( 'NONE',  ( 63.71132485994279904, 155.0000000000000000, -15.00000000000002487 ) ) ;
#11843 = ORIENTED_EDGE ( 'NONE', *, *, #14170, .F. ) ;
#11844 = PLANE ( 'NONE',  #17296 ) ;
#11845 = CARTESIAN_POINT ( 'NONE',  ( -0.05014649552828365914, 215.4116977939061144, 75.24886208192143044 ) ) ;
#11846 = AXIS2_PLACEMENT_3D ( 'NONE', #6952, #14778, #22446 ) ;
#11847 = EDGE_LOOP ( 'NONE', ( #17875, #14273, #25885, #27730, #23547 ) ) ;
#11848 = B_SPLINE_CURVE_WITH_KNOTS ( 'NONE', 3,
 ( #27294, #17409, #3950, #9404 ),
 .UNSPECIFIED., .F., .F.,
 ( 4, 4 ),
 ( -0.0005136321342257200344, 1.626303258728256651E-18 ),
 .UNSPECIFIED. ) ;
#11849 = AXIS2_PLACEMENT_3D ( 'NONE', #3, #30839, #22826 ) ;
#11850 = CARTESIAN_POINT ( 'NONE',  ( 85.42499999726879878, 168.2552932293087906, -9.630534252274387086 ) ) ;
#11851 = ORIENTED_EDGE ( 'NONE', *, *, #10784, .T. ) ;
#11852 = CARTESIAN_POINT ( 'NONE',  ( 69.68867513459484542, 159.8737954434934352, 15.00000000000015277 ) ) ;
#11853 = CARTESIAN_POINT ( 'NONE',  ( 78.72499999726881015, 140.1801316387863778, -4.815267126137194431 ) ) ;
#11854 = DIRECTION ( 'NONE',  ( 1.000000000000000000, 0.000000000000000000, 0.000000000000000000 ) ) ;
#11855 = CARTESIAN_POINT ( 'NONE',  ( -6.500168698208129925, 202.3363017425936050, 81.20113791807858661 ) ) ;
#11856 = EDGE_CURVE ( 'NONE', #982, #27043, #21944, .T. ) ;
#11857 = DIRECTION ( 'NONE',  ( 1.000000000000000000, -0.000000000000000000, -0.000000000000000000 ) ) ;
#11858 = AXIS2_PLACEMENT_3D ( 'NONE', #1350, #32514, #20081 ) ;
#11859 = CARTESIAN_POINT ( 'NONE',  ( 39.10000000000000142, 168.7903194862797420, 4.480746418436729606 ) ) ;
#11860 = CARTESIAN_POINT ( 'NONE',  ( -8.000000000000008882, 206.9523078486584780, 53.49886208192144466 ) ) ;
#11861 = ADVANCED_FACE ( 'NONE', ( #31349 ), #23178, .T. ) ;
#11862 = CARTESIAN_POINT ( 'NONE',  ( -6.500000000000000000, 3.752776749732564809, -6.064240316920399110 ) ) ;
#11863 = CARTESIAN_POINT ( 'NONE',  ( 73.11132485994281183, 140.7341522555726669, 4.635254915624211769 ) ) ;
#11864 = LINE ( 'NONE', #11698, #20378 ) ;
#11865 = CARTESIAN_POINT ( 'NONE',  ( 54.02499999726880731, 160.0630714827496206, 15.58253174999999224 ) ) ;
#11866 = CARTESIAN_POINT ( 'NONE',  ( 65.47499999726881015, 160.0630714827496206, -15.58253175000000823 ) ) ;
#11867 = CARTESIAN_POINT ( 'NONE',  ( 3.662846001190051659, 195.5725841191953691, 59.60113791807857808 ) ) ;
#11868 = CARTESIAN_POINT ( 'NONE',  ( -122.3560003530527780, -4.587378538859857358, 35.00001199999999812 ) ) ;
#11869 = AXIS2_PLACEMENT_3D ( 'NONE', #8676, #5619, #26904 ) ;
#11870 = EDGE_CURVE ( 'NONE', #28642, #5515, #507, .T. ) ;
#11871 = CARTESIAN_POINT ( 'NONE',  ( 9.680171189290831535, 199.9079932115568852, 2.301137918078565825 ) ) ;
#11872 = CARTESIAN_POINT ( 'NONE',  ( 8.118202686958039038, 212.8392687619912635, 79.70113791807857240 ) ) ;
#11873 = CONICAL_SURFACE ( 'NONE', #10814, 18.00000000000000711, 0.9599310885968802554 ) ;
#11874 = CARTESIAN_POINT ( 'NONE',  ( 3.753561863808876797, 195.6020594897209719, 40.59886208192143187 ) ) ;
#11875 = CARTESIAN_POINT ( 'NONE',  ( 10.01549611932659367, 203.7984951890124421, 46.14886208192143613 ) ) ;
#11876 = CARTESIAN_POINT ( 'NONE',  ( 86.69999999453762030, 167.3344367211045096, 8.961492836873468093 ) ) ;
#11877 = CARTESIAN_POINT ( 'NONE',  ( 7.456977232089302632, 217.1783343296989131, 82.55113791807858092 ) ) ;
#11878 = CARTESIAN_POINT ( 'NONE',  ( 8.000000000000008882, 206.9523078486586485, 98.00113791807856956 ) ) ;
#11879 = CARTESIAN_POINT ( 'NONE',  ( 3.044812012439969795, 216.5253028482143520, 63.39886208192144323 ) ) ;
#11880 = AXIS2_PLACEMENT_3D ( 'NONE', #4407, #27566, #30476 ) ;
#11881 = EDGE_LOOP ( 'NONE', ( #15571, #15947, #28232, #29942 ) ) ;
#11882 = CARTESIAN_POINT ( 'NONE',  ( 7.456977232089471386, 196.8216656703012006, 70.44886208192144750 ) ) ;
#11883 = MANIFOLD_SOLID_BREP ( 'M10 Clearance Hole1', #26993 ) ;
#11884 = VERTEX_POINT ( 'NONE', #7852 ) ;
#11885 = CARTESIAN_POINT ( 'NONE',  ( 69.87499999726880162, 171.3844434931184253, -7.942151717890132712E-15 ) ) ;
#11886 = CARTESIAN_POINT ( 'NONE',  ( 6.444103211790928043, 211.7408657792734061, 42.69886208192144039 ) ) ;
#11887 = EDGE_LOOP ( 'NONE', ( #10436, #22916, #14391, #23705 ) ) ;
#11888 = CARTESIAN_POINT ( 'NONE',  ( 83.57499999726880446, 164.1591823560292198, -12.60653300113719766 ) ) ;
#11889 = DIRECTION ( 'NONE',  ( 1.000000000000000000, 0.000000000000000000, 0.000000000000000000 ) ) ;
#11890 = CARTESIAN_POINT ( 'NONE',  ( -9.335145149336232961, 207.8126765316083038, 102.7601261637465910 ) ) ;
#11891 = CARTESIAN_POINT ( 'NONE',  ( -2.426778023690262742, 214.6231898156240163, 61.10113791807857808 ) ) ;
#11892 = VECTOR ( 'NONE', #28425, 1000.000000000000000 ) ;
#11893 = CARTESIAN_POINT ( 'NONE',  ( 103.3032345859876102, 155.0000000000000000, 31.00000000000000000 ) ) ;
#11894 = EDGE_CURVE ( 'NONE', #26009, #32282, #32284, .T. ) ;
#11895 = AXIS2_PLACEMENT_3D ( 'NONE', #15951, #458, #16284 ) ;
#11896 = CARTESIAN_POINT ( 'NONE',  ( 6.220909254589681581, 198.5229672870052582, 40.44886208192141908 ) ) ;
#11897 = VERTEX_POINT ( 'NONE', #5450 ) ;
#11898 = CARTESIAN_POINT ( 'NONE',  ( 2.000000000000000000, 2.449293598294706414E-16, -2.874600000000001376 ) ) ;
#11899 = LINE ( 'NONE', #14618, #1984 ) ;
#11900 = CARTESIAN_POINT ( 'NONE',  ( 86.71132485994282035, 155.0000000000000000, 15.00000000000001243 ) ) ;
#11901 = CARTESIAN_POINT ( 'NONE',  ( -7.984503880673422316, 204.3529502787951628, 20.34886208192143542 ) ) ;
#11902 = CARTESIAN_POINT ( 'NONE',  ( 8.062137200540920645, 201.0835637161417822, 62.30113791807858092 ) ) ;
#11903 = EDGE_CURVE ( 'NONE', #17109, #7326, #25899, .T. ) ;
#11904 = CARTESIAN_POINT ( 'NONE',  ( -0.05014649552810635652, 196.4853777576173002, 44.75113791807858377 ) ) ;
#11905 = CARTESIAN_POINT ( 'NONE',  ( 71.61132485994279762, 150.1262045565062806, -14.99999999999993072 ) ) ;
#11906 = CIRCLE ( 'NONE', #27153, 32.00000000000002842 ) ;
#11907 = CARTESIAN_POINT ( 'NONE',  ( 8.118202686958039038, 212.8392687619912635, 22.70113791807856884 ) ) ;
#11908 = CARTESIAN_POINT ( 'NONE',  ( 8.015496119326595448, 204.4483345814782638, 97.14886208192146455 ) ) ;
#11909 = CARTESIAN_POINT ( 'NONE',  ( 46.82499999726880446, 141.7447067706911810, -9.630534252274385310 ) ) ;
#11910 = CARTESIAN_POINT ( 'NONE',  ( 87.50000000000000000, 154.3213600469173912, -15.33101506908378475 ) ) ;
#11911 = CARTESIAN_POINT ( 'NONE',  ( -7.456977232089304408, 196.8216656703010301, 27.05113791807857027 ) ) ;
#11912 = DIRECTION ( 'NONE',  ( 0.000000000000000000, 0.000000000000000000, 1.000000000000000000 ) ) ;
#11913 = CARTESIAN_POINT ( 'NONE',  ( -10.00000000000000711, 207.0476921513413515, 78.50113791807856956 ) ) ;
#11914 = CARTESIAN_POINT ( 'NONE',  ( 6.220909254589536808, 215.4770327129947987, 52.55113791807857382 ) ) ;
#11915 = LINE ( 'NONE', #6467, #9989 ) ;
#11916 = LINE ( 'NONE', #11415, #31545 ) ;
#11917 = CARTESIAN_POINT ( 'NONE',  ( -3.753561863808878130, 218.3979405102790281, 3.098862081921434530 ) ) ;
#11918 = CARTESIAN_POINT ( 'NONE',  ( 9.984503880673420539, 210.2968891136705736, 18.84886208192143542 ) ) ;
#11919 = CARTESIAN_POINT ( 'NONE',  ( 69.59999999453762598, 141.2096805137202580, -4.480746418436742040 ) ) ;
#11920 = ORIENTED_EDGE ( 'NONE', *, *, #10925, .F. ) ;
#11921 = CARTESIAN_POINT ( 'NONE',  ( -9.736236675707914401, 199.9851607334237542, 54.20113791807856529 ) ) ;
#11922 = VECTOR ( 'NONE', #23267, 1000.000000000000000 ) ;
#11923 = CARTESIAN_POINT ( 'NONE',  ( -8.015496119326531499, 204.4483345814780364, 66.35113791807857808 ) ) ;
#11924 = CARTESIAN_POINT ( 'NONE',  ( -10.01549611932659722, 210.2015048109875011, 29.64886208192143968 ) ) ;
#11925 = CARTESIAN_POINT ( 'NONE',  ( 76.41132485994280898, 167.7597621252805880, 9.270509831248428867 ) ) ;
#11926 = EDGE_LOOP ( 'NONE', ( #13475, #11786, #9251, #13878 ) ) ;
#11927 = AXIS2_PLACEMENT_3D ( 'NONE', #5275, #13116, #10247 ) ;
#11928 = DIRECTION ( 'NONE',  ( 0.000000000000000000, 0.000000000000000000, -1.000000000000000000 ) ) ;
#11929 = CARTESIAN_POINT ( 'NONE',  ( 3.044812012440130555, 197.4746971517856764, 89.60113791807857808 ) ) ;
#11930 = ORIENTED_EDGE ( 'NONE', *, *, #10323, .T. ) ;
#11931 = CARTESIAN_POINT ( 'NONE',  ( 87.50000000000000000, 160.9457742543943652, -14.40357817542362540 ) ) ;
#11932 = DIRECTION ( 'NONE',  ( 1.000000000000000000, 0.000000000000000000, 0.000000000000000000 ) ) ;
#11933 = ORIENTED_EDGE ( 'NONE', *, *, #14726, .T. ) ;
#11934 = CARTESIAN_POINT ( 'NONE',  ( -4.903702542908602524, 213.8346818373418898, 36.95113791807857950 ) ) ;
#11935 = FACE_OUTER_BOUND ( 'NONE', #27046, .T. ) ;
#11936 = CARTESIAN_POINT ( 'NONE',  ( -0.05014649552828403384, 217.5146222423826714, 15.24886208192143044 ) ) ;
#11937 = CARTESIAN_POINT ( 'NONE',  ( 50.77499999726880731, 140.1801316387863778, 4.815267126137185549 ) ) ;
#11938 = ORIENTED_EDGE ( 'NONE', *, *, #14952, .T. ) ;
#11939 = CARTESIAN_POINT ( 'NONE',  ( 8.015496119326531499, 209.5516654185219636, 46.85113791807857098 ) ) ;
#11940 = LINE ( 'NONE', #4093, #29230 ) ;
#11941 = DIRECTION ( 'NONE',  ( 0.000000000000000000, 0.000000000000000000, 1.000000000000000000 ) ) ;
#11942 = LINE ( 'NONE', #6826, #17919 ) ;
#11943 = AXIS2_PLACEMENT_3D ( 'NONE', #21674, #21171, #16383 ) ;
#11944 = CARTESIAN_POINT ( 'NONE',  ( -9.984503880673420539, 203.7031108863293980, 89.34886208192143897 ) ) ;
#11945 = CARTESIAN_POINT ( 'NONE',  ( 61.27499999726882152, 149.9369285172503510, -15.58253175000000823 ) ) ;
#11946 = CARTESIAN_POINT ( 'NONE',  ( -3.044812012440131443, 216.5253028482142952, 34.10113791807857808 ) ) ;
#11947 = CARTESIAN_POINT ( 'NONE',  ( -1.750000000000014211, 3.031088913245526317, 0.000000000000000000 ) ) ;
#11948 = CARTESIAN_POINT ( 'NONE',  ( 3.044812012440130555, 197.4746971517856764, 14.60113791807856565 ) ) ;
#11949 = CARTESIAN_POINT ( 'NONE',  ( 121.5000000000000000, 155.0000000000010800, 106.0000000000000142 ) ) ;
#11950 = CARTESIAN_POINT ( 'NONE',  ( 80.39999999999999147, 150.2886644046228639, -14.50000000000000888 ) ) ;
#11951 = DIRECTION ( 'NONE',  ( 1.000000000000000000, 0.000000000000000000, 0.000000000000000000 ) ) ;
#11952 = CARTESIAN_POINT ( 'NONE',  ( 2.346298152288388561, -2.686816014504594730, -1.834956978294293449E-14 ) ) ;
#11953 = CARTESIAN_POINT ( 'NONE',  ( -7.456977232089304408, 196.8216656703010301, 0.05113791807856556820 ) ) ;
#11954 = CARTESIAN_POINT ( 'NONE',  ( 42.97499999726881015, 140.1801316387863778, -4.815267126137194431 ) ) ;
#11955 = CARTESIAN_POINT ( 'NONE',  ( 3.135527875058820690, 216.4958274776887492, 43.40113791807856813 ) ) ;
#11956 = CARTESIAN_POINT ( 'NONE',  ( 86.12499999726881583, 155.0000000000000000, 15.58253174999999402 ) ) ;
#11957 = CARTESIAN_POINT ( 'NONE',  ( 45.78867513459482552, 155.0000000000000000, 15.00000000000001243 ) ) ;
#11958 = CARTESIAN_POINT ( 'NONE',  ( 46.89999999453763024, 159.7113355953771077, 14.49999999999999289 ) ) ;
#11959 = EDGE_LOOP ( 'NONE', ( #9405, #1783 ) ) ;
#11960 = CARTESIAN_POINT ( 'NONE',  ( -0.05014649552807705357, 194.3824533091408000, 20.75113791807856600 ) ) ;
#11961 = DIRECTION ( 'NONE',  ( 0.000000000000000000, 0.000000000000000000, -1.000000000000000000 ) ) ;
#11962 = CARTESIAN_POINT ( 'NONE',  ( 65.71132485994280614, 155.0000000000000000, -15.00000000000002487 ) ) ;
#11963 = ORIENTED_EDGE ( 'NONE', *, *, #24948, .F. ) ;
#11964 = CARTESIAN_POINT ( 'NONE',  ( -9.736236675708031640, 214.0148392665760753, 38.79886208192142050 ) ) ;
#11965 = CARTESIAN_POINT ( 'NONE',  ( 8.118202686958039038, 212.8392687619912635, 1.701137918078565736 ) ) ;
#11966 = CARTESIAN_POINT ( 'NONE',  ( 8.118202686958039038, 212.8392687619912635, 64.70113791807857240 ) ) ;
#11967 = CARTESIAN_POINT ( 'NONE',  ( 4.984841277089891776, 200.2242689037093726, 22.44886208192143329 ) ) ;
#11968 = CARTESIAN_POINT ( 'NONE',  ( 7.500000000000000000, 4.330127018922199866, -1.000000000000000888 ) ) ;
#11969 = ORIENTED_EDGE ( 'NONE', *, *, #16455, .F. ) ;
#11970 = CARTESIAN_POINT ( 'NONE',  ( 2.517493886309087436, 199.4062855549015865, 97.59886208192145318 ) ) ;
#11971 = FACE_OUTER_BOUND ( 'NONE', #199, .T. ) ;
#11972 = CARTESIAN_POINT ( 'NONE',  ( -11.98450388067341876, 203.0532714938636047, 89.34886208192143897 ) ) ;
#11973 = FACE_OUTER_BOUND ( 'NONE', #12216, .T. ) ;
#11974 = VERTEX_POINT ( 'NONE', #2569 ) ;
#11975 = CARTESIAN_POINT ( 'NONE',  ( 35.52499999726880731, 169.8198683612136222, -4.815267126137197984 ) ) ;
#11976 = PLANE ( 'NONE',  #2822 ) ;
#11977 = DIRECTION ( 'NONE',  ( 0.000000000000000000, -1.000000000000000000, 0.000000000000000000 ) ) ;
#11978 = CARTESIAN_POINT ( 'NONE',  ( 8.062137200540822946, 212.9164362838583315, 57.69886208192144039 ) ) ;
#11979 = CARTESIAN_POINT ( 'NONE',  ( 38.47499999726881015, 149.9369285172503510, 15.58253174999999580 ) ) ;
#11980 = DIRECTION ( 'NONE',  ( -0.000000000000000000, -0.000000000000000000, -1.000000000000000000 ) ) ;
#11981 = CARTESIAN_POINT ( 'NONE',  ( -8.118202686958039038, 201.1607312380087080, 0.2011379180785657361 ) ) ;
#11982 = CARTESIAN_POINT ( 'NONE',  ( 58.31132485994280046, 169.2658477444273331, 4.635254915624208216 ) ) ;
#11983 = CARTESIAN_POINT ( 'NONE',  ( 61.50000000000000000, 155.0000000000000000, 14.49999999999999467 ) ) ;
#11984 = CARTESIAN_POINT ( 'NONE',  ( 63.81132485994282888, 159.8737954434934920, -15.00000000000012434 ) ) ;
#11985 = CARTESIAN_POINT ( 'NONE',  ( 6.444103211790928043, 211.7408657792734061, 84.69886208192144750 ) ) ;
#11986 = LINE ( 'NONE', #12499, #9663 ) ;
#11987 = CARTESIAN_POINT ( 'NONE',  ( 99.30625411593993590, 155.0000000000000000, 12.00000000000001066 ) ) ;
#11988 = CARTESIAN_POINT ( 'NONE',  ( 7.456977232089471386, 196.8216656703012006, 88.44886208192144750 ) ) ;
#11989 = EDGE_CURVE ( 'NONE', #14208, #16104, #7479, .T. ) ;
#11990 = CARTESIAN_POINT ( 'NONE',  ( 64.32499999726881867, 145.8408176439707802, 12.60653300113718345 ) ) ;
#11992 = EDGE_LOOP ( 'NONE', ( #5753, #23591, #6133 ) ) ;
#11991 = CARTESIAN_POINT ( 'NONE',  ( 8.062137200540920645, 201.0835637161417822, 17.30113791807856671 ) ) ;
#11993 = DIRECTION ( 'NONE',  ( 0.000000000000000000, 0.000000000000000000, -1.000000000000000000 ) ) ;
#11994 = CARTESIAN_POINT ( 'NONE',  ( 82.77499999726880731, 140.1801316387863778, 4.815267126137185549 ) ) ;
#11995 = CARTESIAN_POINT ( 'NONE',  ( -12.00000000000000711, 207.0476921513413515, 87.50113791807856956 ) ) ;
#11996 = DIRECTION ( 'NONE',  ( -1.000000000000000000, -0.000000000000000000, -0.000000000000000000 ) ) ;
#11997 = ADVANCED_FACE ( 'NONE', ( #24174 ), #22517, .T. ) ;
#11998 = ORIENTED_EDGE ( 'NONE', *, *, #5437, .F. ) ;
#11999 = CARTESIAN_POINT ( 'NONE',  ( 11.98450388067341876, 210.9467285061363953, 66.84886208192143897 ) ) ;
#12000 = CARTESIAN_POINT ( 'NONE',  ( -9.984503880673420539, 203.7031108863293980, 80.34886208192143897 ) ) ;
#12001 = CARTESIAN_POINT ( 'NONE',  ( -9.736236675708031640, 214.0148392665760753, 17.79886208192143471 ) ) ;
#12002 = CARTESIAN_POINT ( 'NONE',  ( 58.50000000000001421, -88.00000000000000000, -30.00000000000000000 ) ) ;
#12003 = CARTESIAN_POINT ( 'NONE',  ( -6.220909254589537696, 198.5229672870051161, 36.05113791807857382 ) ) ;
#12004 = CARTESIAN_POINT ( 'NONE',  ( 65.78867513459482552, 155.0000000000000000, 15.00000000000001243 ) ) ;
#12005 = CARTESIAN_POINT ( 'NONE',  ( -8.118202686958138514, 212.8392687619910930, 95.79886208192144181 ) ) ;
#12006 = CARTESIAN_POINT ( 'NONE',  ( -52.50000000000002132, 155.0000000000000000, -6.999999999999957367 ) ) ;
#12007 = ORIENTED_EDGE ( 'NONE', *, *, #6868, .T. ) ;
#12008 = CYLINDRICAL_SURFACE ( 'NONE', #12948, 12.10452846326766441 ) ;
#12009 = CARTESIAN_POINT ( 'NONE',  ( -6.444103211790928043, 202.2591342207265939, 68.19886208192143329 ) ) ;
#12010 = ORIENTED_EDGE ( 'NONE', *, *, #1818, .T. ) ;
#12011 = CARTESIAN_POINT ( 'NONE',  ( 82.22499999726881015, 149.9369285172503510, 15.58253174999999580 ) ) ;
#12012 = ORIENTED_EDGE ( 'NONE', *, *, #344, .F. ) ;
#12013 = CARTESIAN_POINT ( 'NONE',  ( 69.08867513459482268, 167.7597621252805880, -9.270509831248443078 ) ) ;
#12014 = EDGE_CURVE ( 'NONE', #4979, #780, #12180, .T. ) ;
#12015 = CARTESIAN_POINT ( 'NONE',  ( 77.52499999726880731, 169.8198683612136222, -4.815267126137197984 ) ) ;
#12016 = CARTESIAN_POINT ( 'NONE',  ( -7.500000000000000888, 2.575910028905295857, -0.3641256808890092067 ) ) ;
#12017 = CARTESIAN_POINT ( 'NONE',  ( -4.984841277089726574, 200.2242689037092305, 81.05113791807856671 ) ) ;
#12018 = CARTESIAN_POINT ( 'NONE',  ( 87.50000000000000000, 170.2392927197263361, -2.713135339554590519 ) ) ;
#12019 = AXIS2_PLACEMENT_3D ( 'NONE', #2857, #32421, #9086 ) ;
#12020 = FILL_AREA_STYLE ('',( #32632 ) ) ;
#12021 = CARTESIAN_POINT ( 'NONE',  ( 41.89999999999999858, 141.2096805137202580, 4.480746418436733158 ) ) ;
#12022 = CARTESIAN_POINT ( 'NONE',  ( -6.444103211790928043, 202.2591342207265939, 56.19886208192144039 ) ) ;
#12023 = EDGE_CURVE ( 'NONE', #24797, #28445, #10958, .T. ) ;
#12024 = DIRECTION ( 'NONE',  ( 0.000000000000000000, 0.000000000000000000, -1.000000000000000000 ) ) ;
#12025 = DIRECTION ( 'NONE',  ( 0.000000000000000000, 0.000000000000000000, -1.000000000000000000 ) ) ;
#12026 = DIRECTION ( 'NONE',  ( 0.000000000000000000, 0.5000000000000009992, 0.8660254037844380415 ) ) ;
#12027 = CARTESIAN_POINT ( 'NONE',  ( 50.92499999726880588, 145.8408176439707802, -12.60653300113719588 ) ) ;
#12028 = CARTESIAN_POINT ( 'NONE',  ( 61.97499999726881015, 169.8198683612136222, 4.815267126137181997 ) ) ;
#12029 = CARTESIAN_POINT ( 'NONE',  ( 9.680171189290831535, 199.9079932115568852, 62.30113791807858092 ) ) ;
#12030 = DIRECTION ( 'NONE',  ( 0.000000000000000000, -1.000000000000000000, 0.000000000000000000 ) ) ;
#12031 = CARTESIAN_POINT ( 'NONE',  ( 11.98450388067348271, 203.0532714938637753, -0.8488620819214346414 ) ) ;
#12032 = CARTESIAN_POINT ( 'NONE',  ( -8.118202686958039038, 201.1607312380087080, 81.20113791807857240 ) ) ;
#12033 = EDGE_CURVE ( 'NONE', #9926, #21869, #16523, .T. ) ;
#12034 = CARTESIAN_POINT ( 'NONE',  ( 7.456977232089471386, 196.8216656703012006, 43.44886208192143329 ) ) ;
#12035 = CARTESIAN_POINT ( 'NONE',  ( 6.220909254589680693, 198.5229672870052582, 46.44886208192142618 ) ) ;
#12036 = LINE ( 'NONE', #27711, #19916 ) ;
#12037 =( BOUNDED_CURVE ( )  B_SPLINE_CURVE ( 2, ( #2362, #3022, #2862, #18203, #12753, #10702, #4913, #18030, #28759, #2533, #33532 ),
 .UNSPECIFIED., .F., .T. ) 
 B_SPLINE_CURVE_WITH_KNOTS ( ( 3, 2, 2, 2, 2, 3 ),
 ( 0.7321428571428569843, 0.7357142857142855430, 0.7392857142857141017, 0.7428571428571425495, 0.7464285714285712192, 0.7499999999999997780 ),
 .UNSPECIFIED. ) 
 CURVE ( )  GEOMETRIC_REPRESENTATION_ITEM ( )  RATIONAL_B_SPLINE_CURVE ( ( 1.000000000000001554, 0.9510565162951518658, 1.000000000000000000, 0.9510565162951534202, 1.000000000000000000, 0.9510565162951534202, 1.000000000000000000, 0.9510565162951534202, 1.000000000000000000, 0.9510565162951564178, 0.9999999999999970024 ) ) 
 REPRESENTATION_ITEM ( '' )  );
#12038 = CARTESIAN_POINT ( 'NONE',  ( -3.662846001190052991, 218.4274158808045740, 88.10113791807857808 ) ) ;
#12039 = CARTESIAN_POINT ( 'NONE',  ( -10.00000000000000711, 207.0476921513413515, 3.501137918078566003 ) ) ;
#12040 = CARTESIAN_POINT ( 'NONE',  ( 8.062137200540822946, 212.9164362838583315, 63.69886208192143329 ) ) ;
#12041 = DIRECTION ( 'NONE',  ( 0.000000000000000000, 0.000000000000000000, -1.000000000000000000 ) ) ;
#12042 = ORIENTED_EDGE ( 'NONE', *, *, #28275, .F. ) ;
#12043 = CARTESIAN_POINT ( 'NONE',  ( -12.01549611932659722, 210.8513442034533227, 71.64886208192143613 ) ) ;
#12044 = AXIS2_PLACEMENT_3D ( 'NONE', #22206, #32595, #9261 ) ;
#12045 = ORIENTED_EDGE ( 'NONE', *, *, #8702, .T. ) ;
#12046 = CARTESIAN_POINT ( 'NONE',  ( 71.97499999726881015, 169.8198683612136222, 4.815267126137181997 ) ) ;
#12047 = CARTESIAN_POINT ( 'NONE',  ( 2.517493886309087436, 199.4062855549015865, 43.59886208192144608 ) ) ;
#12048 = ORIENTED_EDGE ( 'NONE', *, *, #15823, .T. ) ;
#12049 = EDGE_CURVE ( 'NONE', #948, #11897, #18218, .T. ) ;
#12050 = CARTESIAN_POINT ( 'NONE',  ( 86.17499999726881299, 164.1591823560292198, 12.60653300113718167 ) ) ;
#12051 = CARTESIAN_POINT ( 'NONE',  ( 67.50000000000000000, 155.0000000000000000, 7.500000000000007994 ) ) ;
#12052 = CARTESIAN_POINT ( 'NONE',  ( 3.783380760145018981E-16, -7.895640089090872671, -6.564402953523720718 ) ) ;
#12053 = CARTESIAN_POINT ( 'NONE',  ( -7.984503880673488041, 209.6470497212046098, 63.65113791807855392 ) ) ;
#12054 = SURFACE_STYLE_FILL_AREA ( #20061 ) ;
#12055 = CARTESIAN_POINT ( 'NONE',  ( -0.05014649552828403384, 217.5146222423826714, 42.24886208192143755 ) ) ;
#12056 = ORIENTED_EDGE ( 'NONE', *, *, #2470, .F. ) ;
#12057 = LINE ( 'NONE', #19563, #25977 ) ;
#12058 =( NAMED_UNIT ( * ) PLANE_ANGLE_UNIT ( ) SI_UNIT ( $, .RADIAN. ) );
#12059 = CARTESIAN_POINT ( 'NONE',  ( 6.725979247667765115, -3.622307570260320020, -6.470294263593358686 ) ) ;
#12060 = CARTESIAN_POINT ( 'NONE',  ( -67.50000000000000000, -92.00000000000000000, 270.4495957273638282 ) ) ;
#12061 = CARTESIAN_POINT ( 'NONE',  ( 2.426778023690075337, 214.6231898156240447, 21.39886208192143613 ) ) ;
#12062 = CARTESIAN_POINT ( 'NONE',  ( 3.044812012440130555, 197.4746971517856764, 65.60113791807857808 ) ) ;
#12063 = CARTESIAN_POINT ( 'NONE',  ( 3.044812012440130555, 197.4746971517856764, 50.60113791807857808 ) ) ;
#12064 = CARTESIAN_POINT ( 'NONE',  ( 125.0000000000000000, 3.061616997868383121E-14, -35.00000000000000000 ) ) ;
#12065 = ITEM_DEFINED_TRANSFORMATION ( 'NONE', 'NONE', #14812,  #2404 ) ;
#12066 = CARTESIAN_POINT ( 'NONE',  ( 8.062137200540920645, 201.0835637161417822, 14.30113791807856671 ) ) ;
#12067 = AXIS2_PLACEMENT_3D ( 'NONE', #25905, #18410, #28802 ) ;
#12068 = CARTESIAN_POINT ( 'NONE',  ( 6.444103211791042618, 202.2591342207267644, 5.301137918078567601 ) ) ;
#12069 = CARTESIAN_POINT ( 'NONE',  ( 43.82499999726881157, 168.2552932293087906, 9.630534252274372875 ) ) ;
#12070 = SURFACE_STYLE_FILL_AREA ( #20078 ) ;
#12071 = CARTESIAN_POINT ( 'NONE',  ( 87.50000000000004263, 146.7973767059698957, -12.63337674179619974 ) ) ;
#12072 = CARTESIAN_POINT ( 'NONE',  ( -11.98450388067348804, 210.9467285061362247, 30.65113791807856458 ) ) ;
#12073 = CARTESIAN_POINT ( 'NONE',  ( 97.30927364589244632, 155.0000000000000000, 31.00000000000000000 ) ) ;
#12074 = CARTESIAN_POINT ( 'NONE',  ( 6.139770520408368348, 198.4640165459539674, 74.45113791807857240 ) ) ;
#12075 = CARTESIAN_POINT ( 'NONE',  ( -8.118202686958039038, 201.1607312380087080, 51.20113791807857240 ) ) ;
#12076 = DIRECTION ( 'NONE',  ( 0.000000000000000000, -0.4999999999999994449, 0.8660254037844389297 ) ) ;
#12077 = DIRECTION ( 'NONE',  ( 0.000000000000000000, -1.000000000000000000, 0.000000000000000000 ) ) ;
#12078 = CARTESIAN_POINT ( 'NONE',  ( -7.375838497908014268, 196.7627149292498530, 11.04886208192143648 ) ) ;
#12079 = CARTESIAN_POINT ( 'NONE',  ( -8.118202686958138514, 212.8392687619910930, 17.79886208192143826 ) ) ;
#12080 = CARTESIAN_POINT ( 'NONE',  ( 68.09999999453764019, 159.7113355953771077, -14.50000000000000888 ) ) ;
#12081 = AXIS2_PLACEMENT_3D ( 'NONE', #12145, #11808, #6701 ) ;
#12082 = ORIENTED_EDGE ( 'NONE', *, *, #5161, .F. ) ;
#12083 = CARTESIAN_POINT ( 'NONE',  ( 12.01549611932652972, 210.8513442034534933, 61.85113791807857098 ) ) ;
#12084 = CARTESIAN_POINT ( 'NONE',  ( 6.500168698208129925, 211.6636982574063381, 70.70113791807857240 ) ) ;
#12085 = EDGE_CURVE ( 'NONE', #11089, #27429, #17931, .T. ) ;
#12086 = CARTESIAN_POINT ( 'NONE',  ( -6.220909254589682469, 215.4770327129946850, 26.94886208192142618 ) ) ;
#12087 = EDGE_CURVE ( 'NONE', #7020, #3486, #8368, .T. ) ;
#12088 = CARTESIAN_POINT ( 'NONE',  ( -7.894787914004607998, -1.230850257101226302E-13, -7.591390474663425536 ) ) ;
#12089 = ORIENTED_EDGE ( 'NONE', *, *, #31845, .T. ) ;
#12090 = EDGE_LOOP ( 'NONE', ( #31404, #4515 ) ) ;
#12091 = ORIENTED_EDGE ( 'NONE', *, *, #15560, .T. ) ;
#12092 = ADVANCED_FACE ( 'NONE', ( #27478 ), #22362, .T. ) ;
#12093 = FACE_OUTER_BOUND ( 'NONE', #3629, .T. ) ;
#12094 = PRODUCT_DEFINITION_FORMATION_WITH_SPECIFIED_SOURCE ( 'ANY', '', #14029, .NOT_KNOWN. ) ;
#12095 = CYLINDRICAL_SURFACE ( 'NONE', #27967, 15.00000000000001776 ) ;
#12096 = ORIENTED_EDGE ( 'NONE', *, *, #7853, .F. ) ;
#12097 = CARTESIAN_POINT ( 'NONE',  ( -0.05014649552807731031, 198.5883022060938572, 29.75113791807856956 ) ) ;
#12098 = EDGE_CURVE ( 'NONE', #73, #23539, #16569, .T. ) ;
#12099 = FACE_OUTER_BOUND ( 'NONE', #23332, .T. ) ;
#12100 = CARTESIAN_POINT ( 'NONE',  ( -10.01549611932659722, 210.2015048109875011, 11.64886208192143258 ) ) ;
#12101 = CARTESIAN_POINT ( 'NONE',  ( 59.77499999726881441, 169.8198683612136222, -4.815267126137197984 ) ) ;
#12102 = EDGE_LOOP ( 'NONE', ( #1223, #10275, #2917, #28981, #16693 ) ) ;
#12103 = CARTESIAN_POINT ( 'NONE',  ( -6.500168698208129925, 202.3363017425936050, 54.20113791807857240 ) ) ;
#12104 = DIRECTION ( 'NONE',  ( 0.5000000000000041078, 0.8660254037844362651, -0.000000000000000000 ) ) ;
#12105 = AXIS2_PLACEMENT_3D ( 'NONE', #13817, #11438, #8870 ) ;
#12106 = CARTESIAN_POINT ( 'NONE',  ( 105.0000000000000142, 3.061616997868383121E-14, -20.00000000000000355 ) ) ;
#12107 = CARTESIAN_POINT ( 'NONE',  ( 8.062137200540822946, 212.9164362838583315, 102.6988620819214475 ) ) ;
#12108 = AXIS2_PLACEMENT_3D ( 'NONE', #24106, #23943, #16774 ) ;
#12109 = CARTESIAN_POINT ( 'NONE',  ( 63.37499999726880873, 155.0000000000000000, -15.58253175000000823 ) ) ;
#12110 = CARTESIAN_POINT ( 'NONE',  ( -3.135527875058821579, 197.5041725223112223, 29.90113791807856813 ) ) ;
#12111 = SURFACE_STYLE_USAGE ( .BOTH. , #14664 ) ;
#12112 = CARTESIAN_POINT ( 'NONE',  ( 8.062137200540920645, 201.0835637161417822, 17.30113791807856671 ) ) ;
#12113 = B_SPLINE_CURVE_WITH_KNOTS ( 'NONE', 3,
 ( #1932, #4317, #27648, #32931, #4140, #14702 ),
 .UNSPECIFIED., .F., .F.,
 ( 4, 2, 4 ),
 ( 0.005649496001316481157, 0.006672230966438324681, 0.007694965931560168206 ),
 .UNSPECIFIED. ) ;
#12114 = CARTESIAN_POINT ( 'NONE',  ( 121.5000000000000000, 80.04668119422662187, 74.95331880577468553 ) ) ;
#12115 = CARTESIAN_POINT ( 'NONE',  ( 81.20000000000000284, 167.3344367211045096, 8.961492836873468093 ) ) ;
#12116 = CARTESIAN_POINT ( 'NONE',  ( -58.33685448808505214, 194.9217985566783113, -2.500000000000000444 ) ) ;
#12117 = CARTESIAN_POINT ( 'NONE',  ( 0.000000000000000000, 0.000000000000000000, 0.000000000000000000 ) ) ;
#12118 = CARTESIAN_POINT ( 'NONE',  ( 9.984503880673470277, 203.7031108863295401, 101.1511379180785752 ) ) ;
#12119 = LINE ( 'NONE', #4280, #3146 ) ;
#12120 = CARTESIAN_POINT ( 'NONE',  ( 44.17499999726881299, 164.1591823560292198, 12.60653300113718167 ) ) ;
#12121 = CARTESIAN_POINT ( 'NONE',  ( -3.044812012440131443, 216.5253028482142952, 43.10113791807857808 ) ) ;
#12122 = CARTESIAN_POINT ( 'NONE',  ( 80.52499999726880731, 140.1801316387863778, 4.815267126137185549 ) ) ;
#12123 = CARTESIAN_POINT ( 'NONE',  ( -27.50000000000000000, 15.87713240271474824, -15.54379906938135214 ) ) ;
#12124 = FACE_OUTER_BOUND ( 'NONE', #21942, .T. ) ;
#12125 = CARTESIAN_POINT ( 'NONE',  ( 47.89999999453762314, 150.2886644046228639, -14.50000000000000888 ) ) ;
#12126 = ORIENTED_EDGE ( 'NONE', *, *, #19348, .F. ) ;
#12127 = CARTESIAN_POINT ( 'NONE',  ( 3.753561863808689836, 218.3979405102790565, 25.40113791807857169 ) ) ;
#12128 = DIRECTION ( 'NONE',  ( -1.000000000000000000, 0.000000000000000000, 0.000000000000000000 ) ) ;
#12129 = CARTESIAN_POINT ( 'NONE',  ( 6.220909254589681581, 198.5229672870052582, 4.448862081921432399 ) ) ;
#12130 = CARTESIAN_POINT ( 'NONE',  ( 66.21132485994282035, 170.7719333635740497, -7.904646289410545231E-15 ) ) ;
#12131 = ORIENTED_EDGE ( 'NONE', *, *, #24915, .T. ) ;
#12132 = VECTOR ( 'NONE', #2152, 1000.000000000000000 ) ;
#12133 = CARTESIAN_POINT ( 'NONE',  ( -8.062137200540920645, 212.9164362838581894, 0.8011379180785658249 ) ) ;
#12134 = CARTESIAN_POINT ( 'NONE',  ( 8.062137200540920645, 201.0835637161417822, 62.30113791807858092 ) ) ;
#12135 = CIRCLE ( 'NONE', #28459, 2.149999999999974598 ) ;
#12136 = CARTESIAN_POINT ( 'NONE',  ( 2.517493886309087436, 199.4062855549015865, 22.59886208192143542 ) ) ;
#12137 = DIRECTION ( 'NONE',  ( 1.000000000000000000, -0.000000000000000000, -0.000000000000000000 ) ) ;
#12138 = ORIENTED_EDGE ( 'NONE', *, *, #12853, .F. ) ;
#12139 = CARTESIAN_POINT ( 'NONE',  ( -0.05014649552807731031, 198.5883022060938572, 5.751137918078564226 ) ) ;
#12140 = FACE_BOUND ( 'NONE', #27823, .T. ) ;
#12141 = CARTESIAN_POINT ( 'NONE',  ( 7.456977232089471386, 196.8216656703012006, 85.44886208192144750 ) ) ;
#12142 = CARTESIAN_POINT ( 'NONE',  ( 35.47499999726880304, 160.0630714827496206, -15.58253175000000823 ) ) ;
#12143 = ORIENTED_EDGE ( 'NONE', *, *, #32617, .F. ) ;
#12144 = CARTESIAN_POINT ( 'NONE',  ( 44.52499999726881441, 140.1801316387863778, 4.815267126137185549 ) ) ;
#12145 = CARTESIAN_POINT ( 'NONE',  ( -64.50000000000000000, 155.0000000000000000, 6.938893903907228378E-15 ) ) ;
#12146 = CARTESIAN_POINT ( 'NONE',  ( -0.05014649552810635652, 196.4853777576173002, -0.2488620819214343305 ) ) ;
#12147 = CARTESIAN_POINT ( 'NONE',  ( 0.05014649552828275708, 196.4853777576173002, 67.74886208192140202 ) ) ;
#12148 = CARTESIAN_POINT ( 'NONE',  ( 41.27499999726880731, 149.9369285172503510, -15.58253175000000823 ) ) ;
#12149 = CARTESIAN_POINT ( 'NONE',  ( -31.74999999999995737, 9.797174393178825657E-16, -8.000000000000000000 ) ) ;
#12150 = CARTESIAN_POINT ( 'NONE',  ( -9.984503880673473830, 210.2968891136704315, 3.651137918078565026 ) ) ;
#12151 = PRODUCT_DEFINITION_SHAPE ( 'NONE', 'NONE',  #1908 ) ;
#12152 = CARTESIAN_POINT ( 'NONE',  ( -10.47863426674271814, 207.9189531262114770, 102.6635298682156758 ) ) ;
#12153 = VECTOR ( 'NONE', #8544, 1000.000000000000000 ) ;
#12154 = CARTESIAN_POINT ( 'NONE',  ( 62.50000000000000000, 155.0000000000000000, -14.50000000000000711 ) ) ;
#12155 = CARTESIAN_POINT ( 'NONE',  ( -8.118202686958039038, 201.1607312380087080, 90.20113791807857240 ) ) ;
#12156 = CARTESIAN_POINT ( 'NONE',  ( 125.0000000000000000, 25.00000000000004619, 20.00000000000000000 ) ) ;
#12157 = CARTESIAN_POINT ( 'NONE',  ( -2.517493886309087880, 214.5937144450984135, 87.09886208192143897 ) ) ;
#12158 = CARTESIAN_POINT ( 'NONE',  ( -1.269541193505925744E-15, 7.895640089090863789, -6.564402953523717166 ) ) ;
#12159 = VECTOR ( 'NONE', #16738, 1000.000000000000000 ) ;
#12160 = CARTESIAN_POINT ( 'NONE',  ( 42.49999999999999289, -103.0000000000000142, -20.00000000000000000 ) ) ;
#12161 = CARTESIAN_POINT ( 'NONE',  ( 7.456977232089471386, 196.8216656703012006, 85.44886208192144750 ) ) ;
#12162 = AXIS2_PLACEMENT_3D ( 'NONE', #24572, #19960, #22524 ) ;
#12163 = CARTESIAN_POINT ( 'NONE',  ( 62.12499999726880873, 155.0000000000000000, 15.58253174999999402 ) ) ;
#12165 = ORIENTED_EDGE ( 'NONE', *, *, #15906, .T. ) ;
#12164 = CARTESIAN_POINT ( 'NONE',  ( -8.118202686958039038, 201.1607312380087080, 21.20113791807856529 ) ) ;
#12166 = DIRECTION ( 'NONE',  ( 0.000000000000000000, -1.000000000000000000, 0.000000000000000000 ) ) ;
#12167 = CARTESIAN_POINT ( 'NONE',  ( 82.47499999726881015, 149.9369285172503510, 15.58253174999999580 ) ) ;
#12168 = CARTESIAN_POINT ( 'NONE',  ( 12.00000000000000711, 206.9523078486586485, 83.00113791807856956 ) ) ;
#12169 = DIRECTION ( 'NONE',  ( -1.000000000000000000, -0.000000000000000000, -0.000000000000000000 ) ) ;
#12170 = ORIENTED_EDGE ( 'NONE', *, *, #15990, .F. ) ;
#12171 = CARTESIAN_POINT ( 'NONE',  ( 12.00000000000000711, 207.0476921513415220, 66.99886208192144466 ) ) ;
#12172 = AXIS2_PLACEMENT_3D ( 'NONE', #26311, #24247, #5690 ) ;
#12173 = CARTESIAN_POINT ( 'NONE',  ( -10.00000000000000711, 206.9523078486584495, 74.49886208192144466 ) ) ;
#12174 = CARTESIAN_POINT ( 'NONE',  ( 9.680171189290716072, 214.0920067884432854, 15.69886208192143684 ) ) ;
#12175 = CARTESIAN_POINT ( 'NONE',  ( -27.50000000000001066, -2.682974265912532186, -18.00000000000001066 ) ) ;
#12176 = CARTESIAN_POINT ( 'NONE',  ( -8.062137200540920645, 212.9164362838581894, 36.80113791807856671 ) ) ;
#12177 = CARTESIAN_POINT ( 'NONE',  ( 2.385244779468109755E-15, 4.041451884327391220, -2.587392608830344720 ) ) ;
#12178 = CARTESIAN_POINT ( 'NONE',  ( 0.05014649552828275708, 196.4853777576173002, 94.74886208192141623 ) ) ;
#12179 = CARTESIAN_POINT ( 'NONE',  ( 6.725979247667768668, 3.622307570260308918, -6.470294263593358686 ) ) ;
#12180 = CIRCLE ( 'NONE', #27963, 3.047499999999999876 ) ;
#12181 = ORIENTED_EDGE ( 'NONE', *, *, #27992, .T. ) ;
#12182 = FACE_BOUND ( 'NONE', #8444, .T. ) ;
#12183 = CARTESIAN_POINT ( 'NONE',  ( 6.500168698208244500, 202.3363017425938324, 85.29886208192145602 ) ) ;
#12184 = ORIENTED_EDGE ( 'NONE', *, *, #19308, .T. ) ;
#12185 = EDGE_CURVE ( 'NONE', #7112, #29388, #27985, .T. ) ;
#12186 = CARTESIAN_POINT ( 'NONE',  ( 34.21132485994281325, 170.7719333635740497, -7.904646289410545231E-15 ) ) ;
#12187 = ORIENTED_EDGE ( 'NONE', *, *, #537, .T. ) ;
#12188 = CARTESIAN_POINT ( 'NONE',  ( 3.500000000000004885, 2.020725942163702715, -2.587392608830344720 ) ) ;
#12189 = CARTESIAN_POINT ( 'NONE',  ( 76.22499999726882436, 149.9369285172503510, 15.58253174999999580 ) ) ;
#12190 = DIRECTION ( 'NONE',  ( -1.000000000000000000, 0.000000000000000000, 0.000000000000000000 ) ) ;
#12191 =( BOUNDED_CURVE ( )  B_SPLINE_CURVE ( 2, ( #12312, #7207, #19647, #29874, #3970, #24763, #6533, #30544, #30379, #1746, #22708 ),
 .UNSPECIFIED., .F., .F. ) 
 B_SPLINE_CURVE_WITH_KNOTS ( ( 3, 2, 2, 2, 2, 3 ),
 ( 0.8571428571428570953, 0.8607142857142856540, 0.8642857142857142128, 0.8678571428571427715, 0.8714285714285714413, 0.8750000000000000000 ),
 .UNSPECIFIED. ) 
 CURVE ( )  GEOMETRIC_REPRESENTATION_ITEM ( )  RATIONAL_B_SPLINE_CURVE ( ( 1.000000000000000000, 0.9510565162951534202, 1.000000000000000000, 0.9510565162951534202, 1.000000000000000000, 0.9510565162951534202, 1.000000000000000000, 0.9510565162951534202, 1.000000000000000000, 0.9510565162951534202, 1.000000000000000000 ) ) 
 REPRESENTATION_ITEM ( '' )  );
#12192 = CARTESIAN_POINT ( 'NONE',  ( -2.426778023690262742, 214.6231898156240163, 82.10113791807857808 ) ) ;
#12193 = CARTESIAN_POINT ( 'NONE',  ( 87.50000000000005684, 169.5031880795791324, 4.588213833768849170 ) ) ;
#12194 = COLOUR_RGB ( '', 0.09019608, 0.27058824, 0.51372549) ;
#12195 = CARTESIAN_POINT ( 'NONE',  ( 44.19999999999999574, 142.6655632788954620, -8.961492836873480528 ) ) ;
#12196 = CARTESIAN_POINT ( 'NONE',  ( 2.426778023690075337, 214.6231898156240447, 57.39886208192144323 ) ) ;
#12197 = DIRECTION ( 'NONE',  ( 0.000000000000000000, 0.000000000000000000, 1.000000000000000000 ) ) ;
#12198 = CARTESIAN_POINT ( 'NONE',  ( 0.000000000000000000, 0.000000000000000000, -2.874600000000001376 ) ) ;
#12199 = DIRECTION ( 'NONE',  ( 0.000000000000000000, 0.000000000000000000, -1.000000000000000000 ) ) ;
#12200 = CARTESIAN_POINT ( 'NONE',  ( 49.62499999726880873, 171.3844434931184253, -7.942151717890134290E-15 ) ) ;
#12201 = CARTESIAN_POINT ( 'NONE',  ( 63.97499999726881725, 169.8198683612136222, 4.815267126137181997 ) ) ;
#12202 = CARTESIAN_POINT ( 'NONE',  ( -9.680171189290831535, 214.0920067884431148, 54.80113791807857382 ) ) ;
#12203 = CARTESIAN_POINT ( 'NONE',  ( 40.91132485994280188, 146.1832212156128890, 12.13525491562421976 ) ) ;
#12204 = CARTESIAN_POINT ( 'NONE',  ( -0.05014649552810635652, 196.4853777576173002, 101.7511379180785411 ) ) ;
#12205 = CARTESIAN_POINT ( 'NONE',  ( 0.05014649552810506589, 217.5146222423826714, 82.25113791807856956 ) ) ;
#12206 = CARTESIAN_POINT ( 'NONE',  ( 7.375838497908012492, 217.2372850707501186, 45.54886208192143471 ) ) ;
#12207 = CARTESIAN_POINT ( 'NONE',  ( -3.044812012439970683, 197.4746971517856196, 43.89886208192142902 ) ) ;
#12208 = CARTESIAN_POINT ( 'NONE',  ( -6.500000000000000000, 3.752776749732564809, -0.7999999999999969358 ) ) ;
#12209 = CARTESIAN_POINT ( 'NONE',  ( 9.680171189290831535, 199.9079932115568852, 86.30113791807858092 ) ) ;
#12210 = CARTESIAN_POINT ( 'NONE',  ( 92.60208470531341618, 155.0000000000000000, 0.000000000000000000 ) ) ;
#12211 = CARTESIAN_POINT ( 'NONE',  ( 0.05014649552810505201, 217.5146222423826714, 7.251137918078566003 ) ) ;
#12212 = CARTESIAN_POINT ( 'NONE',  ( 9.984503880673420539, 210.2968891136705167, 69.84886208192143897 ) ) ;
#12213 = LINE ( 'NONE', #25152, #14008 ) ;
#12214 = ORIENTED_EDGE ( 'NONE', *, *, #22076, .T. ) ;
#12215 = CARTESIAN_POINT ( 'NONE',  ( -3.753561863808878130, 218.3979405102790281, 75.09886208192142476 ) ) ;
#12216 = EDGE_LOOP ( 'NONE', ( #20726, #9842, #24662, #19932, #26745 ) ) ;
#12217 = CARTESIAN_POINT ( 'NONE',  ( 75.57499999726881867, 164.1591823560292198, -12.60653300113719766 ) ) ;
#12218 = CARTESIAN_POINT ( 'NONE',  ( 6.444103211790928043, 211.7408657792734061, 48.69886208192144750 ) ) ;
#12219 = ORIENTED_EDGE ( 'NONE', *, *, #19981, .T. ) ;
#12220 = EDGE_CURVE ( 'NONE', #24113, #14984, #9937, .T. ) ;
#12221 = CARTESIAN_POINT ( 'NONE',  ( 86.27499999726880731, 160.0630714827496206, 15.58253174999999224 ) ) ;
#12222 = DIRECTION ( 'NONE',  ( 1.000000000000000000, 0.000000000000000000, 0.000000000000000000 ) ) ;
#12223 = CARTESIAN_POINT ( 'NONE',  ( -58.50000000000002132, 209.9999999999999716, 0.000000000000000000 ) ) ;
#12224 = CARTESIAN_POINT ( 'NONE',  ( 54.12499999726881583, 155.0000000000000000, 15.58253174999999402 ) ) ;
#12225 = CARTESIAN_POINT ( 'NONE',  ( -3.250000000000004441, 5.629165124598849879, 0.000000000000000000 ) ) ;
#12226 = CARTESIAN_POINT ( 'NONE',  ( -3.135527875058982783, 216.4958274776886924, 42.09886208192143897 ) ) ;
#12227 = ORIENTED_EDGE ( 'NONE', *, *, #12276, .F. ) ;
#12228 = CARTESIAN_POINT ( 'NONE',  ( 44.71132485994280614, 155.0000000000000000, 15.00000000000001243 ) ) ;
#12229 = ADVANCED_FACE ( 'NONE', ( #6866 ), #21389, .T. ) ;
#12230 = DIRECTION ( 'NONE',  ( -0.000000000000000000, 0.000000000000000000, -1.000000000000000000 ) ) ;
#12231 = LINE ( 'NONE', #20069, #28358 ) ;
#12232 = CARTESIAN_POINT ( 'NONE',  ( 2.426778023690075337, 214.6231898156240447, 24.39886208192143258 ) ) ;
#12233 = CARTESIAN_POINT ( 'NONE',  ( -10.00000000000000711, 207.0476921513413515, 63.50113791807856956 ) ) ;
#12234 = CARTESIAN_POINT ( 'NONE',  ( 3.135527875058820690, 216.4958274776887492, 43.40113791807856813 ) ) ;
#12235 = ITEM_DEFINED_TRANSFORMATION ( 'NONE', 'NONE', #18642,  #2404 ) ;
#12236 = CARTESIAN_POINT ( 'NONE',  ( -9.984503880673473830, 210.2968891136704315, 18.65113791807856813 ) ) ;
#12237 = CARTESIAN_POINT ( 'NONE',  ( -6.444103211791042618, 211.7408657792732356, 6.801137918078567601 ) ) ;
#12238 = CARTESIAN_POINT ( 'NONE',  ( 44.62499999726880873, 138.6155565068815463, -3.929120461958505118E-15 ) ) ;
#12239 = CARTESIAN_POINT ( 'NONE',  ( 1.156317065392246990, -3.373851915354654007, -2.870065989602839984 ) ) ;
#12240 = CARTESIAN_POINT ( 'NONE',  ( 125.5000000000000000, 155.0000000000000000, 112.0000000000000711 ) ) ;
#12241 = CARTESIAN_POINT ( 'NONE',  ( -11.98450388067348804, 210.9467285061362247, 24.65113791807857169 ) ) ;
#12242 = DIRECTION ( 'NONE',  ( 0.9945218953682689600, 1.280104479605745523E-17, 0.1045284632676951458 ) ) ;
#12243 = EDGE_CURVE ( 'NONE', #16646, #9697, #31236, .T. ) ;
#12244 = CARTESIAN_POINT ( 'NONE',  ( 10.00000000000000711, 206.9523078486586201, 80.00113791807856956 ) ) ;
#12245 = CARTESIAN_POINT ( 'NONE',  ( -6.139770520408368348, 215.5359834540460042, 51.95113791807857240 ) ) ;
#12246 = CARTESIAN_POINT ( 'NONE',  ( -65.20000000000000284, -7.347880794884118356E-15, -19.30000000000003979 ) ) ;
#12247 = DIRECTION ( 'NONE',  ( 1.000000000000000000, 0.000000000000000000, 0.000000000000000000 ) ) ;
#12248 = CARTESIAN_POINT ( 'NONE',  ( 11.98450388067341876, 210.9467285061363953, 12.84886208192143719 ) ) ;
#12249 = CARTESIAN_POINT ( 'NONE',  ( -8.118202686958138514, 212.8392687619910930, 14.79886208192143648 ) ) ;
#12250 = CARTESIAN_POINT ( 'NONE',  ( 71.79999999453762882, 146.4771138417591203, -11.73074641843674470 ) ) ;
#12251 = EDGE_LOOP ( 'NONE', ( #12143, #10679 ) ) ;
#12252 = CARTESIAN_POINT ( 'NONE',  ( 9.680171189290831535, 199.9079932115568852, 56.30113791807857382 ) ) ;
#12253 = CARTESIAN_POINT ( 'NONE',  ( 8.015496119326531499, 209.5516654185219636, 79.85113791807857808 ) ) ;
#12254 = ADVANCED_FACE ( 'NONE', ( #26118, #2786 ), #13166, .F. ) ;
#12255 = CARTESIAN_POINT ( 'NONE',  ( -8.118202686958138514, 212.8392687619910930, 41.79886208192143471 ) ) ;
#12256 = FACE_OUTER_BOUND ( 'NONE', #28695, .T. ) ;
#12257 = ORIENTED_EDGE ( 'NONE', *, *, #25979, .F. ) ;
#12258 = ORIENTED_EDGE ( 'NONE', *, *, #12448, .F. ) ;
#12259 = ORIENTED_EDGE ( 'NONE', *, *, #16847, .T. ) ;
#12260 = CARTESIAN_POINT ( 'NONE',  ( -7.500000000000000000, 4.330127018922191873, -0.9999999999999970024 ) ) ;
#12261 = CARTESIAN_POINT ( 'NONE',  ( 0.000000000000000000, 0.000000000000000000, 0.000000000000000000 ) ) ;
#12262 = ORIENTED_EDGE ( 'NONE', *, *, #20440, .F. ) ;
#12263 = CARTESIAN_POINT ( 'NONE',  ( -4.903702542908602524, 213.8346818373418898, 33.95113791807857240 ) ) ;
#12264 = CARTESIAN_POINT ( 'NONE',  ( 65.71132485994280614, 155.0000000000000000, -15.00000000000002487 ) ) ;
#12265 = CARTESIAN_POINT ( 'NONE',  ( 10.00000000000000711, 207.0476921513415220, 12.99886208192143400 ) ) ;
#12266 = CARTESIAN_POINT ( 'NONE',  ( 56.17499999726881299, 164.1591823560292198, 12.60653300113718167 ) ) ;
#12267 = EDGE_LOOP ( 'NONE', ( #16031, #10054, #2931, #30752 ) ) ;
#12268 = CARTESIAN_POINT ( 'NONE',  ( 8.000000000000008882, 206.9523078486586485, 47.00113791807856956 ) ) ;
#12269 = CARTESIAN_POINT ( 'NONE',  ( 125.5000000000000000, 78.52640161467553526, 73.43303922622362734 ) ) ;
#12270 = SHAPE_REPRESENTATION_RELATIONSHIP ( 'NONE' , 'NONE' ,  #13706, #31568 ) ;
#12271 = CARTESIAN_POINT ( 'NONE',  ( 56.71132485994280614, 155.0000000000000000, 15.00000000000001243 ) ) ;
#12272 = CARTESIAN_POINT ( 'NONE',  ( -3.135527875058982783, 216.4958274776886924, 96.09886208192143897 ) ) ;
#12273 = CARTESIAN_POINT ( 'NONE',  ( 63.57499999726881867, 164.1591823560292198, -12.60653300113719766 ) ) ;
#12274 = CARTESIAN_POINT ( 'NONE',  ( 10.00000000000000711, 206.9523078486586201, 29.00113791807856956 ) ) ;
#12275 = DIRECTION ( 'NONE',  ( 0.000000000000000000, 0.000000000000000000, -1.000000000000000000 ) ) ;
#12276 = EDGE_CURVE ( 'NONE', #28362, #2597, #8065, .T. ) ;
#12277 = EDGE_CURVE ( 'NONE', #12741, #1999, #33658, .T. ) ;
#12278 = CARTESIAN_POINT ( 'NONE',  ( 8.118202686958039038, 212.8392687619912635, 13.70113791807856707 ) ) ;
#12279 = DIRECTION ( 'NONE',  ( 0.000000000000000000, 6.982962677686266711E-15, 1.000000000000000000 ) ) ;
#12280 = CARTESIAN_POINT ( 'NONE',  ( 77.20000000000001705, 167.3344367211045096, 8.961492836873468093 ) ) ;
#12281 = CARTESIAN_POINT ( 'NONE',  ( 32.50000000000000000, 155.0000000000000000, 15.00000000000001243 ) ) ;
#12282 = CARTESIAN_POINT ( 'NONE',  ( -1.013799215429234768E-15, 7.550813340387307449, -6.286444963328104762 ) ) ;
#12283 = CARTESIAN_POINT ( 'NONE',  ( 11.98450388067348271, 203.0532714938637753, -0.8488620819214346414 ) ) ;
#12284 = CARTESIAN_POINT ( 'NONE',  ( 48.68867513459482410, 150.1262045565065364, -15.00000000000012434 ) ) ;
#12285 = CARTESIAN_POINT ( 'NONE',  ( 51.47499999726881725, 160.0630714827496206, -15.58253175000000823 ) ) ;
#12286 = EDGE_CURVE ( 'NONE', #16646, #24872, #18943, .T. ) ;
#12287 = CARTESIAN_POINT ( 'NONE',  ( 10.01549611932653860, 210.2015048109876716, 49.85113791807857808 ) ) ;
#12288 = CARTESIAN_POINT ( 'NONE',  ( 81.12499999726881583, 155.0000000000000000, -15.58253175000000823 ) ) ;
#12289 = CARTESIAN_POINT ( 'NONE',  ( 52.61132485994279762, 159.8737954434937478, 14.99999999999991651 ) ) ;
#12290 = CARTESIAN_POINT ( 'NONE',  ( -5.000000000000000000, -5.773502691896264416, -7.063244554130003294 ) ) ;
#12291 = CARTESIAN_POINT ( 'NONE',  ( 52.49999999453762456, 170.2462022514548323, -7.872454543227099337E-15 ) ) ;
#12292 = VERTEX_POINT ( 'NONE', #24219 ) ;
#12293 = CARTESIAN_POINT ( 'NONE',  ( 7.456977232089302632, 217.1783343296989131, 31.55113791807857027 ) ) ;
#12294 = EDGE_CURVE ( 'NONE', #27576, #12292, #20456, .T. ) ;
#12295 = CARTESIAN_POINT ( 'NONE',  ( 4.922818201202977306, 207.4297999410988780, -9.402818167433192542 ) ) ;
#12296 = CARTESIAN_POINT ( 'NONE',  ( -10.01549611932659722, 210.2015048109875011, 2.648862081921434797 ) ) ;
#12297 = CARTESIAN_POINT ( 'NONE',  ( 125.0000000000000000, 3.061616997868383121E-14, 35.00200000000000244 ) ) ;
#12298 = ORIENTED_EDGE ( 'NONE', *, *, #3497, .F. ) ;
#12299 = CARTESIAN_POINT ( 'NONE',  ( 6.139770520408368348, 198.4640165459539674, -0.5488620819214343749 ) ) ;
#12300 = CARTESIAN_POINT ( 'NONE',  ( -8.118202686958039038, 201.1607312380087080, 66.20113791807857240 ) ) ;
#12301 = VERTEX_POINT ( 'NONE', #8719 ) ;
#12302 = CARTESIAN_POINT ( 'NONE',  ( -0.05014649552828365914, 215.4116977939061144, 24.24886208192144110 ) ) ;
#12303 = FACE_OUTER_BOUND ( 'NONE', #23236, .T. ) ;
#12304 = ORIENTED_EDGE ( 'NONE', *, *, #13315, .F. ) ;
#12305 = CARTESIAN_POINT ( 'NONE',  ( 4.903702542908601636, 200.1653181626581102, 2.451137918078566180 ) ) ;
#12306 = DIRECTION ( 'NONE',  ( 1.000000000000000000, 0.000000000000000000, 0.000000000000000000 ) ) ;
#12307 = CIRCLE ( 'NONE', #21020, 4.200000000000001954 ) ;
#12308 = CARTESIAN_POINT ( 'NONE',  ( -0.05014649552828442242, 219.6175466908591716, 84.24886208192143044 ) ) ;
#12309 = CARTESIAN_POINT ( 'NONE',  ( 38.77499999726881441, 140.1801316387863778, 4.815267126137185549 ) ) ;
#12310 = VERTEX_POINT ( 'NONE', #32057 ) ;
#12311 = CARTESIAN_POINT ( 'NONE',  ( 47.32499999726881867, 164.1591823560292198, -12.60653300113719766 ) ) ;
#12312 = CARTESIAN_POINT ( 'NONE',  ( 39.78867513459481842, 155.0000000000000000, 15.00000000000001243 ) ) ;
#12313 = CARTESIAN_POINT ( 'NONE',  ( 10.00000000000000711, 206.9523078486586201, 2.001137918078565558 ) ) ;
#12314 = CLOSED_SHELL ( 'NONE', ( #19715, #4562, #4152, #10644, #23936, #10761, #3324, #15148, #4744, #19588, #22933, #8879, #1476, #17501 ) ) ;
#12315 = CARTESIAN_POINT ( 'NONE',  ( -8.062137200540822946, 201.0835637161416400, 71.19886208192144750 ) ) ;
#12316 = CARTESIAN_POINT ( 'NONE',  ( 46.97499999726881015, 140.1801316387863778, -4.815267126137194431 ) ) ;
#12317 = CARTESIAN_POINT ( 'NONE',  ( 0.000000000000000000, 0.000000000000000000, -9.974600000000000577 ) ) ;
#12318 = CARTESIAN_POINT ( 'NONE',  ( -10.00000000000000711, 207.0476921513413515, 0.5011379180785656695 ) ) ;
#12319 = CARTESIAN_POINT ( 'NONE',  ( 58.41132485994281609, 167.7597621252805880, 9.270509831248428867 ) ) ;
#12320 = EDGE_CURVE ( 'NONE', #4513, #7333, #3917, .T. ) ;
#12321 = AXIS2_PLACEMENT_3D ( 'NONE', #10694, #15960, #28587 ) ;
#12322 = CARTESIAN_POINT ( 'NONE',  ( 59.30000000000000426, 163.5228861582408797, 11.73074641843673049 ) ) ;
#12323 = CARTESIAN_POINT ( 'NONE',  ( -6.220909254589537696, 198.5229672870051161, 90.05113791807858092 ) ) ;
#12324 = DIRECTION ( 'NONE',  ( 0.000000000000000000, 0.000000000000000000, -1.000000000000000000 ) ) ;
#12325 = CARTESIAN_POINT ( 'NONE',  ( -10.01549611932653860, 203.7984951890123284, 78.35113791807857808 ) ) ;
#12326 = CARTESIAN_POINT ( 'NONE',  ( -7.500000000000000000, -4.330127018922199866, -1.000000000000000888 ) ) ;
#12327 = CARTESIAN_POINT ( 'NONE',  ( 34.37499999726881583, 155.0000000000000000, 15.58253174999999402 ) ) ;
#12328 = CARTESIAN_POINT ( 'NONE',  ( -12.01549611932659722, 210.8513442034533227, 89.64886208192142192 ) ) ;
#12329 = CARTESIAN_POINT ( 'NONE',  ( 62.52499999726882152, 140.1801316387863778, 4.815267126137185549 ) ) ;
#12331 = ORIENTED_EDGE ( 'NONE', *, *, #3139, .F. ) ;
#12330 = CARTESIAN_POINT ( 'NONE',  ( 6.139770520408367460, 198.4640165459539389, 17.45113791807856174 ) ) ;
#12332 = CARTESIAN_POINT ( 'NONE',  ( 3.499999999999999556, 0.000000000000000000, -2.899999999999999911 ) ) ;
#12333 = CARTESIAN_POINT ( 'NONE',  ( 79.87499999726880162, 171.3844434931184253, -7.942151717890132712E-15 ) ) ;
#12334 = CARTESIAN_POINT ( 'NONE',  ( -12.01549611932652972, 203.1486557965464499, 90.35113791807857808 ) ) ;
#12335 = DIRECTION ( 'NONE',  ( -1.000000000000000000, 0.000000000000000000, 0.000000000000000000 ) ) ;
#12336 = STYLED_ITEM ( 'NONE', ( #14469 ), #23155 ) ;
#12337 = ORIENTED_EDGE ( 'NONE', *, *, #29099, .T. ) ;
#12338 = CARTESIAN_POINT ( 'NONE',  ( -3.662846001189865142, 195.5725841191952838, 73.89886208192143613 ) ) ;
#12339 = VECTOR ( 'NONE', #21938, 1000.000000000000000 ) ;
#12340 = CARTESIAN_POINT ( 'NONE',  ( 6.139770520408223575, 215.5359834540460611, 81.54886208192144181 ) ) ;
#12341 = CARTESIAN_POINT ( 'NONE',  ( 9.680171189290716072, 214.0920067884432854, 9.698862081921433287 ) ) ;
#12342 = CARTESIAN_POINT ( 'NONE',  ( -27.50000000000001066, -14.58598892539969860, -15.91652008647649197 ) ) ;
#12343 = CARTESIAN_POINT ( 'NONE',  ( -8.118202686958039038, 201.1607312380087080, 33.20113791807857240 ) ) ;
#12344 = CARTESIAN_POINT ( 'NONE',  ( -67.50000000000000000, 155.0000000000000000, 6.938893903907228378E-15 ) ) ;
#12345 = CARTESIAN_POINT ( 'NONE',  ( 10.01549611932659545, 203.7984951890123853, 97.14886208192145034 ) ) ;
#12346 = AXIS2_PLACEMENT_3D ( 'NONE', #748, #7929, #5849 ) ;
#12347 = CARTESIAN_POINT ( 'NONE',  ( 62.70000000000001705, -88.00000000000000000, -30.00000000000000000 ) ) ;
#12348 = ORIENTED_EDGE ( 'NONE', *, *, #32900, .F. ) ;
#12349 = FACE_OUTER_BOUND ( 'NONE', #16734, .T. ) ;
#12350 = CARTESIAN_POINT ( 'NONE',  ( 0.05014649552828262524, 198.5883022060938572, 76.74886208192144466 ) ) ;
#12351 = ORIENTED_EDGE ( 'NONE', *, *, #28082, .T. ) ;
#12352 = CARTESIAN_POINT ( 'NONE',  ( 33.71132485994280614, 155.0000000000000000, -15.00000000000002487 ) ) ;
#12353 = ORIENTED_EDGE ( 'NONE', *, *, #7308, .T. ) ;
#12354 = CARTESIAN_POINT ( 'NONE',  ( -54.79999999999999716, -6.711064459327494323E-15, 270.4495957273638282 ) ) ;
#12355 = AXIS2_PLACEMENT_3D ( 'NONE', #2828, #3822, #6206 ) ;
#12356 = CARTESIAN_POINT ( 'NONE',  ( 73.17499999726881299, 145.8408176439707802, -12.60653300113719588 ) ) ;
#12357 = CARTESIAN_POINT ( 'NONE',  ( 81.42499999726882720, 168.2552932293087906, -9.630534252274385310 ) ) ;
#12358 = FACE_OUTER_BOUND ( 'NONE', #2593, .T. ) ;
#12359 = CARTESIAN_POINT ( 'NONE',  ( -8.000000000000008882, 207.0476921513413515, 75.50113791807856956 ) ) ;
#12360 = PLANE ( 'NONE',  #26578 ) ;
#12361 = AXIS2_PLACEMENT_3D ( 'NONE', #27890, #9499, #1498 ) ;
#12362 = CARTESIAN_POINT ( 'NONE',  ( 43.50000000000000711, 155.0000000000000000, 14.49999999999999467 ) ) ;
#12363 = CARTESIAN_POINT ( 'NONE',  ( 7.984503880673422316, 209.6470497212048372, 57.84886208192144608 ) ) ;
#12364 = TOROIDAL_SURFACE ( 'NONE', #2606, 4.999999999999993783, 1.000000000000000222 ) ;
#12365 = CARTESIAN_POINT ( 'NONE',  ( -6.499999999999999112, -1.280811194704858158, -0.07768058122908438889 ) ) ;
#12366 = CARTESIAN_POINT ( 'NONE',  ( 3.250000000000003109, -5.629165124598849879, 0.000000000000000000 ) ) ;
#12367 = CARTESIAN_POINT ( 'NONE',  ( -121.7736297201317086, 4.198250922590448297, 35.00001199999999812 ) ) ;
#12368 = CARTESIAN_POINT ( 'NONE',  ( 59.82499999726880446, 168.2552932293087906, 9.630534252274372875 ) ) ;
#12369 = CARTESIAN_POINT ( 'NONE',  ( 64.87499999726881583, 138.6155565068815463, -3.929120461958505118E-15 ) ) ;
#12370 = CARTESIAN_POINT ( 'NONE',  ( -12.01549611932652972, 203.1486557965464499, 57.35113791807857098 ) ) ;
#12371 = CARTESIAN_POINT ( 'NONE',  ( -52.50000000000002132, 155.0000000000000000, 6.938893903907228378E-15 ) ) ;
#12372 = CARTESIAN_POINT ( 'NONE',  ( -11.98450388067348804, 210.9467285061362247, 3.651137918078566358 ) ) ;
#12373 = EDGE_CURVE ( 'NONE', #20431, #12687, #11612, .T. ) ;
#12374 = CARTESIAN_POINT ( 'NONE',  ( 8.118202686958039038, 212.8392687619912635, 73.70113791807857240 ) ) ;
#12375 = CARTESIAN_POINT ( 'NONE',  ( -3.662846001189865142, 195.5725841191952838, 46.89886208192143613 ) ) ;
#12376 = CARTESIAN_POINT ( 'NONE',  ( 6.139770520408223575, 215.5359834540460611, 45.54886208192144181 ) ) ;
#12377 = CARTESIAN_POINT ( 'NONE',  ( 12.01549611932652972, 210.8513442034534933, 85.85113791807857808 ) ) ;
#12378 = CARTESIAN_POINT ( 'NONE',  ( 68.01132485994283172, 167.7597621252805880, -9.270509831248443078 ) ) ;
#12379 = CIRCLE ( 'NONE', #16726, 1.535500000000000087 ) ;
#12380 = CARTESIAN_POINT ( 'NONE',  ( -6.220909254589537696, 198.5229672870051161, 0.05113791807856577637 ) ) ;
#12381 = CARTESIAN_POINT ( 'NONE',  ( 3.044812012439969795, 216.5253028482143520, 72.39886208192143613 ) ) ;
#12382 = AXIS2_PLACEMENT_3D ( 'NONE', #28230, #25667, #30271 ) ;
#12383 = CARTESIAN_POINT ( 'NONE',  ( -58.50000000000002132, 194.9217985566782829, -2.500000000000000000 ) ) ;
#12384 = ORIENTED_EDGE ( 'NONE', *, *, #17718, .F. ) ;
#12385 = CARTESIAN_POINT ( 'NONE',  ( 0.05014649552828288198, 194.3824533091408000, 73.74886208192144466 ) ) ;
#12386 = VERTEX_POINT ( 'NONE', #16213 ) ;
#12387 = CARTESIAN_POINT ( 'NONE',  ( 77.97499999726881015, 169.8198683612136222, 4.815267126137181997 ) ) ;
#12388 = CARTESIAN_POINT ( 'NONE',  ( 7.984503880673422316, 209.6470497212048372, 48.84886208192143897 ) ) ;
#12390 = ORIENTED_EDGE ( 'NONE', *, *, #21173, .F. ) ;
#12389 = AXIS2_PLACEMENT_3D ( 'NONE', #16749, #11652, #14700 ) ;
#12391 =( BOUNDED_SURFACE ( )  B_SPLINE_SURFACE ( 3, 2, ( 
 ( #14009, #12884, #24407 ),
 ( #13507, #24062, #21336 ),
 ( #29513, #32071, #8404 ),
 ( #6170, #31733, #23277 ),
 ( #13842, #566, #26955 ),
 ( #29352, #19291, #25838 ),
 ( #23901, #10801, #18791 ),
 ( #16561, #21175, #5673 ) ),
 .UNSPECIFIED., .F., .F., .T. ) 
 B_SPLINE_SURFACE_WITH_KNOTS ( ( 4, 2, 2, 4 ),
 ( 3, 3 ),
 ( 0.03861844051980971304, 0.04325213341840642572, 0.04556897986770477860, 0.04788582631700313841 ),
 ( 0.000000000000000000, 1.000000000000000000 ),
 .UNSPECIFIED. ) 
 GEOMETRIC_REPRESENTATION_ITEM ( )  RATIONAL_B_SPLINE_SURFACE ( (
 ( 1.000000000000000000, 0.8047781759831923454, 1.000000000000000000),
 ( 1.000000000000000000, 0.8123762462805160789, 1.000000000000000000),
 ( 1.000000000000000000, 0.8190659850616602844, 1.000000000000000000),
 ( 1.000000000000000000, 0.8191937571013702124, 1.000000000000000000),
 ( 1.000000000000000000, 0.8176092952780309453, 1.000000000000000000),
 ( 1.000000000000000000, 0.8122962088596628050, 1.000000000000000000),
 ( 1.000000000000000000, 0.8086311330827828936, 1.000000000000000000),
 ( 1.000000000000000000, 0.8047712282214327661, 1.000000000000000000) ) ) 
 REPRESENTATION_ITEM ( '' )  SURFACE ( )  );
#12392 = CONICAL_SURFACE ( 'NONE', #33086, 32.10452846326766974, 1.466076571675243523 ) ;
#12393 = CARTESIAN_POINT ( 'NONE',  ( 71.12499999726881583, 155.0000000000000000, -15.58253175000000823 ) ) ;
#12394 = CARTESIAN_POINT ( 'NONE',  ( 6.500000000000576428, -2.723981882618385697, -6.224051986860747121 ) ) ;
#12395 = CARTESIAN_POINT ( 'NONE',  ( -9.521242624480144912, 207.9188892840786878, 102.6634595774070533 ) ) ;
#12396 = CARTESIAN_POINT ( 'NONE',  ( 61.42499999726882010, 168.2552932293087906, -9.630534252274385310 ) ) ;
#12397 = CARTESIAN_POINT ( 'NONE',  ( -8.118202686958138514, 212.8392687619910930, 38.79886208192143471 ) ) ;
#12398 = ORIENTED_EDGE ( 'NONE', *, *, #20830, .T. ) ;
#12399 = CARTESIAN_POINT ( 'NONE',  ( 16.08713178458081217, 22.46635493911270132, -17.92845254598171678 ) ) ;
#12400 = CARTESIAN_POINT ( 'NONE',  ( 2.055025722541879318, -6.319083845363985930, -5.720331885005374595 ) ) ;
#12401 = CARTESIAN_POINT ( 'NONE',  ( 127.5000000000000000, 48.99999999999998579, -1.387778780781445676E-14 ) ) ;
#12402 = CARTESIAN_POINT ( 'NONE',  ( 0.05014649552828262524, 198.5883022060938572, 25.74886208192143755 ) ) ;
#12403 = AXIS2_PLACEMENT_3D ( 'NONE', #9185, #16843, #14965 ) ;
#12404 = CARTESIAN_POINT ( 'NONE',  ( -8.118202686958039038, 201.1607312380087080, 75.20113791807857240 ) ) ;
#12405 = CYLINDRICAL_SURFACE ( 'NONE', #21817, 15.00000000000001776 ) ;
#12406 = CARTESIAN_POINT ( 'NONE',  ( 6.220909254589536808, 215.4770327129947702, 43.55113791807857382 ) ) ;
#12407 = AXIS2_PLACEMENT_3D ( 'NONE', #17291, #15865, #2929 ) ;
#12408 = VECTOR ( 'NONE', #21401, 1000.000000000000114 ) ;
#12409 = CARTESIAN_POINT ( 'NONE',  ( -6.139770520408369237, 215.5359834540460042, 21.95113791807856884 ) ) ;
#12410 = CARTESIAN_POINT ( 'NONE',  ( -4.903702542908602524, 213.8346818373418898, 0.9511379180785658471 ) ) ;
#12411 = CARTESIAN_POINT ( 'NONE',  ( 0.2855619784720492826, -3.876582599186272571, -2.682579934988205128 ) ) ;
#12412 = CARTESIAN_POINT ( 'NONE',  ( 7.456977232089302632, 217.1783343296989131, 31.55113791807857027 ) ) ;
#12413 = FACE_OUTER_BOUND ( 'NONE', #1906, .T. ) ;
#12414 = CARTESIAN_POINT ( 'NONE',  ( 6.220909254589536808, 215.4770327129947702, 76.55113791807855250 ) ) ;
#12415 = EDGE_CURVE ( 'NONE', #21262, #29530, #228, .T. ) ;
#12416 = CARTESIAN_POINT ( 'NONE',  ( 3.135527875058820690, 216.4958274776887492, 46.40113791807857524 ) ) ;
#12417 = CIRCLE ( 'NONE', #1518, 32.00000000000000000 ) ;
#12418 = CARTESIAN_POINT ( 'NONE',  ( 111.1125082318798007, 155.0000000000000000, 0.000000000000000000 ) ) ;
#12419 = CARTESIAN_POINT ( 'NONE',  ( 35.08867513459482979, 167.7597621252805880, -9.270509831248443078 ) ) ;
#12420 = CARTESIAN_POINT ( 'NONE',  ( 9.680171189290716072, 214.0920067884432854, 12.69886208192143684 ) ) ;
#12421 = CARTESIAN_POINT ( 'NONE',  ( -6.139770520408224463, 198.4640165459539105, 23.04886208192143471 ) ) ;
#12422 = CARTESIAN_POINT ( 'NONE',  ( 76.39999999453762314, 168.7903194862797420, -4.480746418436745593 ) ) ;
#12423 = EDGE_LOOP ( 'NONE', ( #7627, #10479, #16911 ) ) ;
#12424 = CARTESIAN_POINT ( 'NONE',  ( -11.98450388067348804, 210.9467285061362247, 60.65113791807856813 ) ) ;
#12425 = EDGE_CURVE ( 'NONE', #13309, #33143, #29166, .T. ) ;
#12426 = CARTESIAN_POINT ( 'NONE',  ( -8.000000000000008882, 207.0476921513413515, 78.50113791807856956 ) ) ;
#12427 = CARTESIAN_POINT ( 'NONE',  ( -3.135527875058982783, 216.4958274776886924, 36.09886208192143897 ) ) ;
#12428 = LINE ( 'NONE', #25370, #2030 ) ;
#12429 = EDGE_LOOP ( 'NONE', ( #8362, #24236 ) ) ;
#12430 = EDGE_CURVE ( 'NONE', #4983, #5638, #32180, .T. ) ;
#12431 = VERTEX_POINT ( 'NONE', #23887 ) ;
#12432 = AXIS2_PLACEMENT_3D ( 'NONE', #23312, #7983, #30991 ) ;
#12433 = EDGE_LOOP ( 'NONE', ( #20263, #27660, #30330 ) ) ;
#12434 = VECTOR ( 'NONE', #26215, 1000.000000000000000 ) ;
#12435 = CARTESIAN_POINT ( 'NONE',  ( 50.98867513459482126, 163.8167787843871110, -12.13525491562423397 ) ) ;
#12436 = CARTESIAN_POINT ( 'NONE',  ( 5.699988423468465015, 4.591578518468247161, -6.344710093416081165 ) ) ;
#12437 = ORIENTED_EDGE ( 'NONE', *, *, #2730, .T. ) ;
#12438 = CARTESIAN_POINT ( 'NONE',  ( -8.015496119326531499, 204.4483345814780364, 36.35113791807857098 ) ) ;
#12439 = CARTESIAN_POINT ( 'NONE',  ( 84.81132485994280046, 150.1262045565062806, 14.99999999999992006 ) ) ;
#12440 = CARTESIAN_POINT ( 'NONE',  ( -3.044812012439970683, 197.4746971517856196, 13.89886208192143613 ) ) ;
#12441 = CARTESIAN_POINT ( 'NONE',  ( 57.07499999726880446, 141.7447067706911810, -9.630534252274387086 ) ) ;
#12443 = ORIENTED_EDGE ( 'NONE', *, *, #15577, .T. ) ;
#12442 = VECTOR ( 'NONE', #25696, 1000.000000000000000 ) ;
#12444 = CARTESIAN_POINT ( 'NONE',  ( 2.426778023690261410, 199.3768101843759837, 62.60113791807857808 ) ) ;
#12445 = CARTESIAN_POINT ( 'NONE',  ( -3.755786496842903988E-16, -7.505553499465146494, -6.064240316920404439 ) ) ;
#12446 = CARTESIAN_POINT ( 'NONE',  ( 57.71132485994280614, 155.0000000000000000, -15.00000000000002487 ) ) ;
#12447 = CARTESIAN_POINT ( 'NONE',  ( 0.05014649552828275708, 196.4853777576173002, 97.74886208192140202 ) ) ;
#12448 = EDGE_CURVE ( 'NONE', #21804, #889, #555, .T. ) ;
#12449 = CARTESIAN_POINT ( 'NONE',  ( 64.87499999726881583, 138.6155565068815463, -3.929120461958505118E-15 ) ) ;
#12450 = CARTESIAN_POINT ( 'NONE',  ( -3.135527875058821579, 197.5041725223112223, 41.90113791807856813 ) ) ;
#12451 = DIRECTION ( 'NONE',  ( 0.000000000000000000, 0.000000000000000000, -1.000000000000000000 ) ) ;
#12452 = CARTESIAN_POINT ( 'NONE',  ( -6.220909254589537696, 198.5229672870051161, 18.05113791807856671 ) ) ;
#12453 = CARTESIAN_POINT ( 'NONE',  ( 87.29999999999999716, 163.5228861582408797, 11.73074641843673049 ) ) ;
#12454 = DIRECTION ( 'NONE',  ( 0.000000000000000000, 0.000000000000000000, -1.000000000000000000 ) ) ;
#12455 = CARTESIAN_POINT ( 'NONE',  ( -9.898309971686792608, 228.3698647632124334, 103.4854814124440452 ) ) ;
#12456 = CONICAL_SURFACE ( 'NONE', #18995, 32.10452846326769816, 1.466076571675243079 ) ;
#12457 = DIRECTION ( 'NONE',  ( 0.000000000000000000, 0.000000000000000000, 1.000000000000000000 ) ) ;
#12458 = CARTESIAN_POINT ( 'NONE',  ( 53.17499999726881299, 145.8408176439707802, -12.60653300113719588 ) ) ;
#12459 = CARTESIAN_POINT ( 'NONE',  ( -3.135527875058821579, 197.5041725223112223, 50.90113791807856813 ) ) ;
#12460 = ADVANCED_FACE ( 'NONE', ( #27279 ), #13804, .T. ) ;
#12461 = CARTESIAN_POINT ( 'NONE',  ( 83.12499999726881583, 155.0000000000000000, -15.58253175000000823 ) ) ;
#12462 = CARTESIAN_POINT ( 'NONE',  ( 41.81132485994281467, 159.8737954434936057, -15.00000000000002665 ) ) ;
#12463 = FACE_OUTER_BOUND ( 'NONE', #32654, .T. ) ;
#12464 = CARTESIAN_POINT ( 'NONE',  ( 54.99999999453762456, 155.0000000000000000, 14.49999999999999467 ) ) ;
#12465 = ORIENTED_EDGE ( 'NONE', *, *, #10184, .F. ) ;
#12466 = CARTESIAN_POINT ( 'NONE',  ( -11.98450388067348804, 210.9467285061362247, 33.65113791807856813 ) ) ;
#12467 = DIRECTION ( 'NONE',  ( 0.000000000000000000, 0.000000000000000000, -1.000000000000000000 ) ) ;
#12468 = CARTESIAN_POINT ( 'NONE',  ( -8.062137200540822946, 201.0835637161416400, 8.198862081921435063 ) ) ;
#12469 = AXIS2_PLACEMENT_3D ( 'NONE', #4793, #17570, #14503 ) ;
#12470 = DIRECTION ( 'NONE',  ( 0.000000000000000000, 0.000000000000000000, -1.000000000000000000 ) ) ;
#12471 = VERTEX_POINT ( 'NONE', #17561 ) ;
#12472 = CARTESIAN_POINT ( 'NONE',  ( -3.135527875058821579, 197.5041725223112223, 8.901137918078566358 ) ) ;
#12473 = CARTESIAN_POINT ( 'NONE',  ( -6.220909254589537696, 198.5229672870051161, 60.05113791807855961 ) ) ;
#12474 = ORIENTED_EDGE ( 'NONE', *, *, #12848, .T. ) ;
#12475 = CARTESIAN_POINT ( 'NONE',  ( 6.500168698208244500, 202.3363017425938324, 19.29886208192143471 ) ) ;
#12476 = EDGE_CURVE ( 'NONE', #3282, #30277, #4623, .T. ) ;
#12477 = B_SPLINE_CURVE_WITH_KNOTS ( 'NONE', 3,
 ( #22673, #27954, #7355, #1553, #9554, #9904 ),
 .UNSPECIFIED., .F., .F.,
 ( 4, 2, 4 ),
 ( 2.380727409348927899E-07, 0.008032766472079795605, 0.01606529487141865678 ),
 .UNSPECIFIED. ) ;
#12478 = DIRECTION ( 'NONE',  ( -1.000000000000000000, 0.000000000000000000, 0.000000000000000000 ) ) ;
#12479 = EDGE_LOOP ( 'NONE', ( #15740, #31368, #13523, #32373 ) ) ;
#12480 = CARTESIAN_POINT ( 'NONE',  ( -8.015496119326531499, 204.4483345814780364, 6.351137918078565647 ) ) ;
#12481 = VECTOR ( 'NONE', #7698, 1000.000000000000000 ) ;
#12482 = EDGE_CURVE ( 'NONE', #33588, #18759, #12477, .T. ) ;
#12483 = FACE_OUTER_BOUND ( 'NONE', #21176, .T. ) ;
#12484 = CARTESIAN_POINT ( 'NONE',  ( -7.456977232089471386, 217.1783343296987709, 92.94886208192144750 ) ) ;
#12485 = CARTESIAN_POINT ( 'NONE',  ( 35.57499999726881157, 164.1591823560292198, -12.60653300113719766 ) ) ;
#12486 = ORIENTED_EDGE ( 'NONE', *, *, #12087, .T. ) ;
#12487 = CARTESIAN_POINT ( 'NONE',  ( 45.12499999726880873, 155.0000000000000000, -15.58253175000000823 ) ) ;
#12488 = CARTESIAN_POINT ( 'NONE',  ( 125.6872233929728111, 5.250000000000034639, 35.00001200000001234 ) ) ;
#12489 = CARTESIAN_POINT ( 'NONE',  ( 8.062137200540920645, 201.0835637161417822, 2.301137918078566269 ) ) ;
#12490 = CARTESIAN_POINT ( 'NONE',  ( -8.062137200540822946, 201.0835637161416400, 68.19886208192144750 ) ) ;
#12491 = CARTESIAN_POINT ( 'NONE',  ( 44.97499999726881015, 140.1801316387863778, -4.815267126137194431 ) ) ;
#12492 = CARTESIAN_POINT ( 'NONE',  ( -67.50001199999998391, 138.1095834939502822, 2.225267283893263226 ) ) ;
#12493 = CARTESIAN_POINT ( 'NONE',  ( 3.135527875058820690, 216.4958274776887492, 4.401137918078565470 ) ) ;
#12494 = CARTESIAN_POINT ( 'NONE',  ( -125.0000000000000000, 0.000000000000000000, -35.00000000000000000 ) ) ;
#12495 = CARTESIAN_POINT ( 'NONE',  ( 64.90000000000000568, 168.7903194862797420, -4.480746418436745593 ) ) ;
#12496 = CARTESIAN_POINT ( 'NONE',  ( -0.05014649552810635652, 196.4853777576173002, 86.75113791807858377 ) ) ;
#12497 = CARTESIAN_POINT ( 'NONE',  ( 64.21132485994282035, 170.7719333635740497, -7.904646289410545231E-15 ) ) ;
#12498 = CARTESIAN_POINT ( 'NONE',  ( -8.062137200540920645, 212.9164362838581894, 72.80113791807856671 ) ) ;
#12499 = CARTESIAN_POINT ( 'NONE',  ( 32.50000000000000000, 155.0000000000000000, 15.00000000000001243 ) ) ;
#12500 = CARTESIAN_POINT ( 'NONE',  ( 34.17499999726881299, 164.1591823560292198, 12.60653300113718167 ) ) ;
#12501 = CARTESIAN_POINT ( 'NONE',  ( -7.375838497908014268, 196.7627149292498530, 86.04886208192145602 ) ) ;
#12502 = CARTESIAN_POINT ( 'NONE',  ( 63.32499999726881867, 164.1591823560292198, -12.60653300113719766 ) ) ;
#12504 = ORIENTED_EDGE ( 'NONE', *, *, #21426, .F. ) ;
#12503 = CARTESIAN_POINT ( 'NONE',  ( 6.220909254589536808, 215.4770327129947987, 34.55113791807856671 ) ) ;
#12505 = CARTESIAN_POINT ( 'NONE',  ( 107.5000000000000000, 155.0000000000000000, -100.0000000000000000 ) ) ;
#12506 = MANIFOLD_SOLID_BREP ( 'Hex', #15589 ) ;
#12507 = CARTESIAN_POINT ( 'NONE',  ( 35.59999999453762598, 141.2096805137202580, -4.480746418436742040 ) ) ;
#12508 = CARTESIAN_POINT ( 'NONE',  ( 9.680171189290831535, 199.9079932115568852, 98.30113791807858092 ) ) ;
#12509 = VECTOR ( 'NONE', #32518, 1000.000000000000000 ) ;
#12510 = FACE_BOUND ( 'NONE', #10646, .T. ) ;
#12511 = VERTEX_POINT ( 'NONE', #11774 ) ;
#12512 = CARTESIAN_POINT ( 'NONE',  ( -10.00000000000000711, 206.9523078486584495, 86.49886208192144466 ) ) ;
#12513 = CARTESIAN_POINT ( 'NONE',  ( 11.98450388067341876, 210.9467285061363953, 27.84886208192143897 ) ) ;
#12514 = DIRECTION ( 'NONE',  ( -1.000000000000000000, 0.000000000000000000, -0.000000000000000000 ) ) ;
#12515 = CARTESIAN_POINT ( 'NONE',  ( -6.139770520408369237, 215.5359834540460042, 30.95113791807857240 ) ) ;
#12516 = CARTESIAN_POINT ( 'NONE',  ( 66.18867513459481700, 140.7341522555726669, 4.635254915624211769 ) ) ;
#12517 = CARTESIAN_POINT ( 'NONE',  ( -8.062137200540822946, 201.0835637161416400, 95.19886208192143329 ) ) ;
#12518 = EDGE_CURVE ( 'NONE', #20519, #11260, #19816, .T. ) ;
#12519 = EDGE_CURVE ( 'NONE', #10922, #9440, #10081, .T. ) ;
#12520 = CARTESIAN_POINT ( 'NONE',  ( 4.424031367836657402, 4.951337798342080099, -6.056431503344841261 ) ) ;
#12521 = ORIENTED_EDGE ( 'NONE', *, *, #22078, .T. ) ;
#12522 = CARTESIAN_POINT ( 'NONE',  ( 70.41132485994282320, 167.7597621252805880, 9.270509831248428867 ) ) ;
#12523 = CARTESIAN_POINT ( 'NONE',  ( -6.444103211790928043, 202.2591342207265939, 80.19886208192143329 ) ) ;
#12524 = EDGE_CURVE ( 'NONE', #3624, #2685, #27986, .T. ) ;
#12525 = ORIENTED_EDGE ( 'NONE', *, *, #5713, .F. ) ;
#12526 = EDGE_CURVE ( 'NONE', #23163, #610, #6368, .T. ) ;
#12527 = ORIENTED_EDGE ( 'NONE', *, *, #8965, .F. ) ;
#12528 = CARTESIAN_POINT ( 'NONE',  ( 80.81132485994281467, 150.1262045565062806, 14.99999999999992006 ) ) ;
#12529 = CARTESIAN_POINT ( 'NONE',  ( 80.32499999726880446, 145.8408176439707802, 12.60653300113718345 ) ) ;
#12530 = CARTESIAN_POINT ( 'NONE',  ( 0.000000000000000000, -1.759474945355388176, -3.047499999999998099 ) ) ;
#12531 = CARTESIAN_POINT ( 'NONE',  ( 4.984841277089725686, 213.7757310962907411, 76.55113791807858092 ) ) ;
#12532 = DIRECTION ( 'NONE',  ( 0.000000000000000000, 0.000000000000000000, -1.000000000000000000 ) ) ;
#12533 = CARTESIAN_POINT ( 'NONE',  ( 42.19999999999999574, 142.6655632788954620, -8.961492836873480528 ) ) ;
#12534 = CARTESIAN_POINT ( 'NONE',  ( -6.500168698208244500, 211.6636982574061676, 53.79886208192144892 ) ) ;
#12535 = CARTESIAN_POINT ( 'NONE',  ( 92.50248874961125978, 155.0000000000000000, 0.000000000000000000 ) ) ;
#12536 = DIRECTION ( 'NONE',  ( -1.000000000000000000, -0.000000000000000000, -0.000000000000000000 ) ) ;
#12537 = CARTESIAN_POINT ( 'NONE',  ( -130.2499999999999716, 0.6872233929727687984, 35.00001199999999102 ) ) ;
#12538 = CARTESIAN_POINT ( 'NONE',  ( 55.12499999726881583, 155.0000000000000000, -15.58253175000000823 ) ) ;
#12539 = CARTESIAN_POINT ( 'NONE',  ( 69.47499999726881015, 160.0630714827496206, -15.58253175000000823 ) ) ;
#12540 = CARTESIAN_POINT ( 'NONE',  ( -11.98450388067348804, 210.9467285061362247, 66.65113791807856103 ) ) ;
#12541 = CARTESIAN_POINT ( 'NONE',  ( 41.71132485994280614, 155.0000000000000000, -15.00000000000002487 ) ) ;
#12542 = CARTESIAN_POINT ( 'NONE',  ( -3.753561863808691168, 195.6020594897209435, 8.901137918078566358 ) ) ;
#12543 = CARTESIAN_POINT ( 'NONE',  ( -0.05014649552810635652, 196.4853777576173002, 74.75113791807858377 ) ) ;
#12544 = CARTESIAN_POINT ( 'NONE',  ( -3.662846001189865142, 195.5725841191952838, 40.89886208192143613 ) ) ;
#12545 = CARTESIAN_POINT ( 'NONE',  ( -8.062137200540822946, 201.0835637161416400, 53.19886208192143329 ) ) ;
#12546 = DIRECTION ( 'NONE',  ( 0.000000000000000000, 0.000000000000000000, 1.000000000000000000 ) ) ;
#12547 = CARTESIAN_POINT ( 'NONE',  ( 7.375838497908181246, 196.7627149292499666, 86.45113791807858661 ) ) ;
#12548 = CARTESIAN_POINT ( 'NONE',  ( 74.08867513459483689, 142.2402378747194405, 9.270509831248432420 ) ) ;
#12549 = CARTESIAN_POINT ( 'NONE',  ( -8.062137200540920645, 212.9164362838581894, 3.801137918078565825 ) ) ;
#12550 = CARTESIAN_POINT ( 'NONE',  ( 10.01549611932659545, 203.7984951890123853, 67.14886208192143613 ) ) ;
#12551 = CARTESIAN_POINT ( 'NONE',  ( 97.30927364589244632, 155.0000000000000000, 0.000000000000000000 ) ) ;
#12552 = VERTEX_POINT ( 'NONE', #7690 ) ;
#12553 = CARTESIAN_POINT ( 'NONE',  ( 11.98450388067341876, 210.9467285061363953, 72.84886208192143897 ) ) ;
#12554 = CARTESIAN_POINT ( 'NONE',  ( -10.00000000000000711, 207.0476921513413515, 87.50113791807858377 ) ) ;
#12555 = MANIFOLD_SOLID_BREP ( 'TorqueElement', #11772 ) ;
#12556 = EDGE_LOOP ( 'NONE', ( #12734, #15904 ) ) ;
#12557 = CARTESIAN_POINT ( 'NONE',  ( 80.07499999726879025, 168.2552932293087906, 9.630534252274372875 ) ) ;
#12558 = CARTESIAN_POINT ( 'NONE',  ( -2.426778023690076225, 199.3768101843759553, 49.89886208192144323 ) ) ;
#12559 = ORIENTED_EDGE ( 'NONE', *, *, #20142, .T. ) ;
#12560 = CARTESIAN_POINT ( 'NONE',  ( 71.32499999726881867, 164.1591823560292198, -12.60653300113719766 ) ) ;
#12561 = DIRECTION ( 'NONE',  ( -1.000000000000000000, 0.000000000000000000, 0.000000000000000000 ) ) ;
#12562 = CARTESIAN_POINT ( 'NONE',  ( -56.61573505521625549, 194.9660755786677555, 1.651105572388385401 ) ) ;
#12563 = AXIS2_PLACEMENT_3D ( 'NONE', #28623, #8013, #18399 ) ;
#12564 = CARTESIAN_POINT ( 'NONE',  ( 60.92499999726882010, 145.8408176439707802, -12.60653300113719588 ) ) ;
#12565 = LINE ( 'NONE', #15116, #15080 ) ;
#12566 = CARTESIAN_POINT ( 'NONE',  ( -10.00000000000000711, 206.9523078486584495, 53.49886208192143755 ) ) ;
#12567 = VERTEX_POINT ( 'NONE', #5457 ) ;
#12568 = FACE_OUTER_BOUND ( 'NONE', #27633, .T. ) ;
#12569 = DIRECTION ( 'NONE',  ( 0.000000000000000000, 0.7071067811865506814, 0.7071067811865442421 ) ) ;
#12570 = DIRECTION ( 'NONE',  ( -1.000000000000000000, -0.000000000000000000, -0.000000000000000000 ) ) ;
#12571 = CARTESIAN_POINT ( 'NONE',  ( -8.000000000000008882, 206.9523078486584780, 20.49886208192143755 ) ) ;
#12572 = CARTESIAN_POINT ( 'NONE',  ( -8.062137200540920645, 212.9164362838581894, 72.80113791807856671 ) ) ;
#12573 = DIRECTION ( 'NONE',  ( -1.000000000000000000, 4.625929269271484928E-16, 0.000000000000000000 ) ) ;
#12574 = CARTESIAN_POINT ( 'NONE',  ( -10.01549611932653860, 203.7984951890123284, 60.35113791807857808 ) ) ;
#12575 = CARTESIAN_POINT ( 'NONE',  ( -6.220909254589537696, 198.5229672870051161, 15.05113791807856671 ) ) ;
#12576 = CARTESIAN_POINT ( 'NONE',  ( -0.05014649552807731031, 198.5883022060938572, 8.751137918078567779 ) ) ;
#12577 = CARTESIAN_POINT ( 'NONE',  ( 1.452965002680450812, -3.202582148906760739, -1.877999099004871997E-14 ) ) ;
#12578 = CARTESIAN_POINT ( 'NONE',  ( 39.02499999726880731, 149.9369285172503510, -15.58253175000000823 ) ) ;
#12579 = CARTESIAN_POINT ( 'NONE',  ( -12.00000000000000711, 207.0476921513413515, 33.50113791807857666 ) ) ;
#12580 = DIRECTION ( 'NONE',  ( 0.000000000000000000, 0.000000000000000000, 1.000000000000000000 ) ) ;
#12581 = CARTESIAN_POINT ( 'NONE',  ( 6.139770520408368348, 198.4640165459539674, 86.45113791807854398 ) ) ;
#12582 = CARTESIAN_POINT ( 'NONE',  ( -8.062137200540920645, 212.9164362838581894, 48.80113791807857382 ) ) ;
#12583 = CARTESIAN_POINT ( 'NONE',  ( -3.500000000000001332, 2.020725942163708488, -2.587392608830344720 ) ) ;
#12584 = CARTESIAN_POINT ( 'NONE',  ( 3.662846001189864698, 218.4274158808046593, 9.398862081921436129 ) ) ;
#12585 = CARTESIAN_POINT ( 'NONE',  ( -3.044812012439970683, 197.4746971517856196, 28.89886208192143613 ) ) ;
#12586 = CARTESIAN_POINT ( 'NONE',  ( 75.49999999453763166, 139.7537977485451393, -4.138211985947621020E-15 ) ) ;
#12587 = EDGE_LOOP ( 'NONE', ( #4765, #6348, #27801, #25616 ) ) ;
#12588 = CARTESIAN_POINT ( 'NONE',  ( -0.05014649552807705357, 194.3824533091408000, 53.75113791807857666 ) ) ;
#12589 = CARTESIAN_POINT ( 'NONE',  ( -7.984503880673488041, 209.6470497212046098, 75.65113791807856103 ) ) ;
#12590 = CARTESIAN_POINT ( 'NONE',  ( 3.044812012439969795, 216.5253028482143520, 42.39886208192143613 ) ) ;
#12591 = CARTESIAN_POINT ( 'NONE',  ( 74.91132485994280898, 146.1832212156128890, 12.13525491562421976 ) ) ;
#12592 = ORIENTED_EDGE ( 'NONE', *, *, #5524, .T. ) ;
#12593 = CARTESIAN_POINT ( 'NONE',  ( 11.98450388067341876, 210.9467285061363953, 45.84886208192143187 ) ) ;
#12594 = ORIENTED_EDGE ( 'NONE', *, *, #33019, .F. ) ;
#12595 = ORIENTED_EDGE ( 'NONE', *, *, #27207, .F. ) ;
#12596 = B_SPLINE_CURVE_WITH_KNOTS ( 'NONE', 3,
 ( #25287, #1443, #2130, #4676, #20175, #30573 ),
 .UNSPECIFIED., .F., .F.,
 ( 4, 2, 4 ),
 ( 0.003981881017442828914, 0.005970145066490142871, 0.007958409115537457695 ),
 .UNSPECIFIED. ) ;
#12597 = CARTESIAN_POINT ( 'NONE',  ( 51.58867513459482268, 163.8167787843871110, 12.13525491562421621 ) ) ;
#12598 = CARTESIAN_POINT ( 'NONE',  ( -65.50384660342780307, 120.9385549553365706, 18.99615339657220758 ) ) ;
#12599 = ORIENTED_EDGE ( 'NONE', *, *, #17904, .F. ) ;
#12600 = CARTESIAN_POINT ( 'NONE',  ( -8.015496119326531499, 204.4483345814780364, 33.35113791807857098 ) ) ;
#12601 = CARTESIAN_POINT ( 'NONE',  ( 81.91132485994279477, 163.8167787843871110, -12.13525491562423397 ) ) ;
#12602 = EDGE_CURVE ( 'NONE', #13425, #10071, #23183, .T. ) ;
#12603 = CARTESIAN_POINT ( 'NONE',  ( -6.139770520408224463, 198.4640165459539389, 17.04886208192143826 ) ) ;
#12604 = CARTESIAN_POINT ( 'NONE',  ( 56.57499999726881157, 145.8408176439707802, 12.60653300113718345 ) ) ;
#12605 = ORIENTED_EDGE ( 'NONE', *, *, #29322, .T. ) ;
#12606 = CARTESIAN_POINT ( 'NONE',  ( -8.015496119326531499, 204.4483345814780364, 60.35113791807857098 ) ) ;
#12607 = FACE_OUTER_BOUND ( 'NONE', #31587, .T. ) ;
#12608 = CARTESIAN_POINT ( 'NONE',  ( 103.3032345859876102, 155.0000000000000000, 0.000000000000000000 ) ) ;
#12609 = CARTESIAN_POINT ( 'NONE',  ( 8.118202686958138514, 201.1607312380088501, 97.29886208192144181 ) ) ;
#12610 = CARTESIAN_POINT ( 'NONE',  ( 66.87499999726880162, 138.6155565068815463, -3.929120461958505118E-15 ) ) ;
#12611 = CARTESIAN_POINT ( 'NONE',  ( 10.01549611932653860, 210.2015048109876716, 43.85113791807854966 ) ) ;
#12612 = PRESENTATION_STYLE_ASSIGNMENT (( #2745 ) ) ;
#12613 = CARTESIAN_POINT ( 'NONE',  ( -3.135527875058821579, 197.5041725223112223, 14.90113791807856636 ) ) ;
#12614 = CARTESIAN_POINT ( 'NONE',  ( -58.50000000000002132, 209.9999999999999716, 0.000000000000000000 ) ) ;
#12615 = DIRECTION ( 'NONE',  ( 6.123233995736766036E-17, 0.000000000000000000, -1.000000000000000000 ) ) ;
#12616 = VECTOR ( 'NONE', #12648, 999.9999999999998863 ) ;
#12617 = CARTESIAN_POINT ( 'NONE',  ( 34.42499999726880588, 141.7447067706911810, 9.630534252274376428 ) ) ;
#12618 = CARTESIAN_POINT ( 'NONE',  ( -7.500000000000000000, 4.330127018922191873, -0.9999999999999970024 ) ) ;
#12619 = CYLINDRICAL_SURFACE ( 'NONE', #26677, 2.500000000000000000 ) ;
#12620 = CARTESIAN_POINT ( 'NONE',  ( -0.05014649552810635652, 196.4853777576173002, 101.7511379180785411 ) ) ;
#12621 = FACE_OUTER_BOUND ( 'NONE', #12479, .T. ) ;
#12622 = CARTESIAN_POINT ( 'NONE',  ( 51.87499999726880162, 171.3844434931184253, -7.942151717890132712E-15 ) ) ;
#12623 = CARTESIAN_POINT ( 'NONE',  ( -3.044812012440131443, 216.5253028482142952, 49.10113791807857808 ) ) ;
#12624 = FACE_OUTER_BOUND ( 'NONE', #84, .T. ) ;
#12625 = CARTESIAN_POINT ( 'NONE',  ( 52.01132485994281041, 167.7597621252805880, -9.270509831248443078 ) ) ;
#12626 = CARTESIAN_POINT ( 'NONE',  ( 60.63708498984762940, 155.0000000000000000, 6.938893903907228378E-15 ) ) ;
#12627 = CARTESIAN_POINT ( 'NONE',  ( 51.59999999453762598, 141.2096805137202580, -4.480746418436742040 ) ) ;
#12628 = ORIENTED_EDGE ( 'NONE', *, *, #23328, .T. ) ;
#12629 = CARTESIAN_POINT ( 'NONE',  ( 12.01549611932652972, 210.8513442034534933, 25.85113791807856742 ) ) ;
#12630 = CARTESIAN_POINT ( 'NONE',  ( 8.118202686958138514, 201.1607312380088501, 16.29886208192143471 ) ) ;
#12631 = CARTESIAN_POINT ( 'NONE',  ( 60.31132485994280756, 169.2658477444273331, 4.635254915624208216 ) ) ;
#12632 = VERTEX_POINT ( 'NONE', #31521 ) ;
#12633 = CARTESIAN_POINT ( 'NONE',  ( 6.220909254589536808, 215.4770327129947702, 10.55113791807856138 ) ) ;
#12634 = CARTESIAN_POINT ( 'NONE',  ( -9.984503880673473830, 210.2968891136704315, 75.65113791807858945 ) ) ;
#12635 = EDGE_CURVE ( 'NONE', #15658, #9623, #1308, .T. ) ;
#12636 = ORIENTED_EDGE ( 'NONE', *, *, #16565, .T. ) ;
#12637 = CARTESIAN_POINT ( 'NONE',  ( 8.015496119326595448, 204.4483345814782638, 25.14886208192143258 ) ) ;
#12638 = CARTESIAN_POINT ( 'NONE',  ( 49.78867513459482552, 155.0000000000000000, 15.00000000000001243 ) ) ;
#12639 = ORIENTED_EDGE ( 'NONE', *, *, #1465, .F. ) ;
#12640 = AXIS2_PLACEMENT_3D ( 'NONE', #13645, #26431, #5976 ) ;
#12641 = CARTESIAN_POINT ( 'NONE',  ( -2.426778023690262742, 214.6231898156240163, 4.101137918078565647 ) ) ;
#12642 = VECTOR ( 'NONE', #2637, 1000.000000000000000 ) ;
#12643 = EDGE_CURVE ( 'NONE', #25501, #11640, #2947, .T. ) ;
#12644 = CARTESIAN_POINT ( 'NONE',  ( 3.753561863808876797, 195.6020594897209719, 88.59886208192143897 ) ) ;
#12645 = CARTESIAN_POINT ( 'NONE',  ( 39.57499999726881157, 164.1591823560292198, -12.60653300113719766 ) ) ;
#12646 = ORIENTED_EDGE ( 'NONE', *, *, #2230, .F. ) ;
#12647 = CARTESIAN_POINT ( 'NONE',  ( 42.52499999726880731, 140.1801316387863778, 4.815267126137185549 ) ) ;
#12648 = DIRECTION ( 'NONE',  ( 0.000000000000000000, -0.5000000000000014433, -0.8660254037844379305 ) ) ;
#12649 = CARTESIAN_POINT ( 'NONE',  ( -6.220909254589537696, 198.5229672870051161, 9.051137918078561384 ) ) ;
#12650 = CARTESIAN_POINT ( 'NONE',  ( -3.135527875058982783, 216.4958274776886924, 69.09886208192143897 ) ) ;
#12651 = CARTESIAN_POINT ( 'NONE',  ( 47.57499999726881867, 164.1591823560292198, -12.60653300113719766 ) ) ;
#12652 = CARTESIAN_POINT ( 'NONE',  ( 78.71132485994280614, 155.0000000000000000, 15.00000000000001243 ) ) ;
#12653 = CARTESIAN_POINT ( 'NONE',  ( -6.220909254589537696, 198.5229672870051161, 15.05113791807856671 ) ) ;
#12654 = CARTESIAN_POINT ( 'NONE',  ( 100.2066581602377653, 155.0000000000000000, 0.000000000000000000 ) ) ;
#12655 = EDGE_CURVE ( 'NONE', #14777, #4510, #26701, .T. ) ;
#12656 = AXIS2_PLACEMENT_3D ( 'NONE', #586, #21358, #7764 ) ;
#12657 = CARTESIAN_POINT ( 'NONE',  ( 64.40000000000001990, 150.2886644046228639, -14.50000000000000888 ) ) ;
#12658 = CARTESIAN_POINT ( 'NONE',  ( 3.044812012440130555, 197.4746971517856764, 101.6011379180785781 ) ) ;
#12659 = CARTESIAN_POINT ( 'NONE',  ( 112.4999999999999858, 155.0000000000000000, -12.00000000000001066 ) ) ;
#12660 = CARTESIAN_POINT ( 'NONE',  ( -9.984503880673473830, 210.2968891136704315, 75.65113791807858945 ) ) ;
#12661 = DIRECTION ( 'NONE',  ( 0.000000000000000000, 0.000000000000000000, 1.000000000000000000 ) ) ;
#12662 = DIRECTION ( 'NONE',  ( 0.000000000000000000, 0.000000000000000000, -1.000000000000000000 ) ) ;
#12663 = CARTESIAN_POINT ( 'NONE',  ( 3.662846001189864698, 218.4274158808046593, 87.39886208192143613 ) ) ;
#12664 = CARTESIAN_POINT ( 'NONE',  ( 72.62499999726880162, 138.6155565068815463, -3.929120461958505118E-15 ) ) ;
#12666 = ORIENTED_EDGE ( 'NONE', *, *, #20956, .F. ) ;
#12665 = CARTESIAN_POINT ( 'NONE',  ( 8.062137200540920645, 201.0835637161417822, 26.30113791807856671 ) ) ;
#12667 = CARTESIAN_POINT ( 'NONE',  ( -58.82767890163440683, 194.9228235633793815, 2.483781759962022218 ) ) ;
#12668 = VECTOR ( 'NONE', #10635, 1000.000000000000000 ) ;
#12669 = CARTESIAN_POINT ( 'NONE',  ( 34.09999999453762598, 159.7113355953771077, -14.50000000000000888 ) ) ;
#12670 = CARTESIAN_POINT ( 'NONE',  ( -7.375838497908182134, 217.2372850707499765, 93.95113791807857240 ) ) ;
#12671 = AXIS2_PLACEMENT_3D ( 'NONE', #8734, #19126, #26785 ) ;
#12672 = EDGE_CURVE ( 'NONE', #11329, #17667, #15466, .T. ) ;
#12673 = CARTESIAN_POINT ( 'NONE',  ( 41.78867513459481842, 155.0000000000000000, 15.00000000000001243 ) ) ;
#12674 = VERTEX_POINT ( 'NONE', #31032 ) ;
#12675 = CARTESIAN_POINT ( 'NONE',  ( -8.062137200540822946, 201.0835637161416400, 86.19886208192144750 ) ) ;
#12676 = CARTESIAN_POINT ( 'NONE',  ( 11.98450388067341876, 210.9467285061363953, 24.84886208192143897 ) ) ;
#12677 = DIRECTION ( 'NONE',  ( 0.000000000000000000, 0.000000000000000000, -1.000000000000000000 ) ) ;
#12678 = CARTESIAN_POINT ( 'NONE',  ( 3.044812012440130555, 197.4746971517856764, 35.60113791807857098 ) ) ;
#12679 = EDGE_CURVE ( 'NONE', #25041, #5261, #3958, .T. ) ;
#12680 = ORIENTED_EDGE ( 'NONE', *, *, #10368, .F. ) ;
#12681 = CARTESIAN_POINT ( 'NONE',  ( -0.05014649552828403384, 217.5146222423826714, 96.24886208192144466 ) ) ;
#12682 = VECTOR ( 'NONE', #10426, 1000.000000000000114 ) ;
#12683 = LINE ( 'NONE', #33470, #32792 ) ;
#12684 = ORIENTED_EDGE ( 'NONE', *, *, #14249, .F. ) ;
#12685 = CARTESIAN_POINT ( 'NONE',  ( 70.61132485994282604, 159.8737954434936057, 15.00000000000001421 ) ) ;
#12686 = CARTESIAN_POINT ( 'NONE',  ( -2.517493886309087880, 214.5937144450984135, 78.09886208192142476 ) ) ;
#12687 = VERTEX_POINT ( 'NONE', #5287 ) ;
#12688 = DIRECTION ( 'NONE',  ( 0.000000000000000000, 0.000000000000000000, 1.000000000000000000 ) ) ;
#12689 = ORIENTED_EDGE ( 'NONE', *, *, #21809, .F. ) ;
#12690 = DIRECTION ( 'NONE',  ( 0.000000000000000000, 0.000000000000000000, 1.000000000000000000 ) ) ;
#12691 = CARTESIAN_POINT ( 'NONE',  ( 0.05014649552807626948, 215.4116977939061144, 58.25113791807857666 ) ) ;
#12692 = AXIS2_PLACEMENT_3D ( 'NONE', #13237, #956, #10862 ) ;
#12693 = AXIS2_PLACEMENT_3D ( 'NONE', #16232, #8242, #16393 ) ;
#12694 = CARTESIAN_POINT ( 'NONE',  ( 84.12499999726881583, 155.0000000000000000, 15.58253174999999402 ) ) ;
#12695 = FACE_OUTER_BOUND ( 'NONE', #26016, .T. ) ;
#12696 = CARTESIAN_POINT ( 'NONE',  ( -7.984503880673488041, 209.6470497212046098, 90.65113791807857524 ) ) ;
#12697 = FACE_OUTER_BOUND ( 'NONE', #10183, .T. ) ;
#12698 = AXIS2_PLACEMENT_3D ( 'NONE', #14439, #19884, #30458 ) ;
#12699 = CARTESIAN_POINT ( 'NONE',  ( 45.20000000000000995, 167.3344367211045096, 8.961492836873468093 ) ) ;
#12700 = CARTESIAN_POINT ( 'NONE',  ( 6.444103211790928043, 211.7408657792734061, 66.69886208192143329 ) ) ;
#12701 = CARTESIAN_POINT ( 'NONE',  ( 88.27499999726880731, 160.0630714827496206, 15.58253174999999402 ) ) ;
#12702 = ADVANCED_FACE ( 'NONE', ( #20461 ), #15680, .F. ) ;
#12703 = EDGE_CURVE ( 'NONE', #13382, #5796, #5227, .T. ) ;
#12704 = CIRCLE ( 'NONE', #15429, 13.00000000000001776 ) ;
#12705 = DIRECTION ( 'NONE',  ( -0.000000000000000000, -0.000000000000000000, 1.000000000000000000 ) ) ;
#12706 = CARTESIAN_POINT ( 'NONE',  ( 27.50000000000000355, 15.87713240271474291, -15.54379906938135214 ) ) ;
#12707 = CARTESIAN_POINT ( 'NONE',  ( 58.62499999726880873, 138.6155565068815747, -3.929120461958505118E-15 ) ) ;
#12708 = CARTESIAN_POINT ( 'NONE',  ( 70.17499999726881299, 164.1591823560292198, 12.60653300113718167 ) ) ;
#12709 = CARTESIAN_POINT ( 'NONE',  ( -7.456977232089304408, 196.8216656703010301, 69.05113791807856671 ) ) ;
#12710 = FACE_BOUND ( 'NONE', #7555, .T. ) ;
#12711 = PRODUCT_DEFINITION_SHAPE ( 'NONE', 'NONE',  #27284 ) ;
#12712 = CARTESIAN_POINT ( 'NONE',  ( 3.753561863808689836, 218.3979405102790565, 13.40113791807856636 ) ) ;
#12713 = EDGE_CURVE ( 'NONE', #14808, #20912, #772, .T. ) ;
#12714 = CARTESIAN_POINT ( 'NONE',  ( 3.044812012440130555, 197.4746971517856764, 83.60113791807857808 ) ) ;
#12715 = CARTESIAN_POINT ( 'NONE',  ( -7.456977232089471386, 217.1783343296987709, 50.94886208192143329 ) ) ;
#12716 = CARTESIAN_POINT ( 'NONE',  ( 6.220909254589680693, 198.5229672870052582, 55.44886208192142618 ) ) ;
#12717 = CARTESIAN_POINT ( 'NONE',  ( -64.96121601855533356, -1.809269760319439646, -19.53878398144470907 ) ) ;
#12718 = VECTOR ( 'NONE', #33269, 1000.000000000000000 ) ;
#12719 = CARTESIAN_POINT ( 'NONE',  ( 3.662846001190051659, 195.5725841191953691, 95.60113791807857808 ) ) ;
#12720 = CARTESIAN_POINT ( 'NONE',  ( -67.50001199999999812, 162.5335705082559059, 15.28016032735713736 ) ) ;
#12721 = CARTESIAN_POINT ( 'NONE',  ( 6.139770520408368348, 198.4640165459539674, -0.5488620819214343749 ) ) ;
#12722 = AXIS2_PLACEMENT_3D ( 'NONE', #8413, #25968, #2971 ) ;
#12723 = EDGE_CURVE ( 'NONE', #24566, #3823, #16010, .T. ) ;
#12724 = CARTESIAN_POINT ( 'NONE',  ( 3.135527875058981895, 197.5041725223112792, 70.59886208192143897 ) ) ;
#12725 = VECTOR ( 'NONE', #26094, 1000.000000000000000 ) ;
#12726 = CARTESIAN_POINT ( 'NONE',  ( 92.60208470531341618, 155.0000000000000000, 0.000000000000000000 ) ) ;
#12727 = ORIENTED_EDGE ( 'NONE', *, *, #22368, .T. ) ;
#12728 = CARTESIAN_POINT ( 'NONE',  ( 9.736236675708031640, 199.9851607334238963, 76.29886208192142760 ) ) ;
#12729 = CARTESIAN_POINT ( 'NONE',  ( -3.135527875058821579, 197.5041725223112223, 92.90113791807857524 ) ) ;
#12730 = MANIFOLD_SOLID_BREP ( 'EndChamfer', #7973 ) ;
#12731 = EDGE_LOOP ( 'NONE', ( #13426, #6545, #18129, #2043 ) ) ;
#12732 = CARTESIAN_POINT ( 'NONE',  ( 77.77499999726880731, 169.8198683612136222, -4.815267126137197984 ) ) ;
#12733 = CARTESIAN_POINT ( 'NONE',  ( 8.000000000000008882, 207.0476921513415220, 48.99886208192144466 ) ) ;
#12734 = ORIENTED_EDGE ( 'NONE', *, *, #858, .T. ) ;
#12735 = CARTESIAN_POINT ( 'NONE',  ( 72.72499999726881015, 140.1801316387863778, -4.815267126137194431 ) ) ;
#12736 = CARTESIAN_POINT ( 'NONE',  ( 6.500000000000000888, 3.402385889607308922, -5.998095356498452269 ) ) ;
#12737 = CARTESIAN_POINT ( 'NONE',  ( -56.00013514549282689, 194.9999915534094725, -0.1669880218061202404 ) ) ;
#12738 = CARTESIAN_POINT ( 'NONE',  ( 62.72499999726881015, 140.1801316387863778, -4.815267126137194431 ) ) ;
#12739 = CARTESIAN_POINT ( 'NONE',  ( -7.500000000000000000, 1.644753667986373458, -7.029983668655349405 ) ) ;
#12740 = CARTESIAN_POINT ( 'NONE',  ( -6.220909254589682469, 215.4770327129946850, 56.94886208192141908 ) ) ;
#12741 = VERTEX_POINT ( 'NONE', #24011 ) ;
#12742 = DIRECTION ( 'NONE',  ( -1.000000000000000000, -2.312964634635740985E-16, 0.000000000000000000 ) ) ;
#12743 = MECHANICAL_DESIGN_GEOMETRIC_PRESENTATION_REPRESENTATION (  '', ( #22542 ), #25262 ) ;
#12744 =( LENGTH_UNIT ( ) NAMED_UNIT ( * ) SI_UNIT ( .MILLI., .METRE. ) );
#12745 = CARTESIAN_POINT ( 'NONE',  ( 7.894787914004607998, -0.7647108141804126458, -7.591390474663421095 ) ) ;
#12746 = CARTESIAN_POINT ( 'NONE',  ( 8.015496119326595448, 204.4483345814782638, 31.14886208192143968 ) ) ;
#12747 = AXIS2_PLACEMENT_3D ( 'NONE', #1367, #11756, #22315 ) ;
#12748 = CARTESIAN_POINT ( 'NONE',  ( -10.01549611932653860, 203.7984951890123284, 72.35113791807859229 ) ) ;
#12749 = DIRECTION ( 'NONE',  ( 0.000000000000000000, 0.000000000000000000, 1.000000000000000000 ) ) ;
#12750 = CARTESIAN_POINT ( 'NONE',  ( 10.01549611932653860, 210.2015048109876716, 55.85113791807857808 ) ) ;
#12751 = CARTESIAN_POINT ( 'NONE',  ( 6.220909254589536808, 215.4770327129947702, 25.55113791807856671 ) ) ;
#12752 = CARTESIAN_POINT ( 'NONE',  ( 2.426778023690261410, 199.3768101843759837, 5.601137918078567424 ) ) ;
#12753 = CARTESIAN_POINT ( 'NONE',  ( 46.38867513459482694, 140.7341522555726669, -4.635254915624220651 ) ) ;
#12754 = DIRECTION ( 'NONE',  ( 1.000000000000000000, -0.000000000000000000, -0.000000000000000000 ) ) ;
#12755 = CARTESIAN_POINT ( 'NONE',  ( 36.92499999726880588, 145.8408176439707802, -12.60653300113719588 ) ) ;
#12756 = CARTESIAN_POINT ( 'NONE',  ( -3.753561863808691168, 195.6020594897209435, 35.90113791807856813 ) ) ;
#12757 = CARTESIAN_POINT ( 'NONE',  ( 0.5620262070071402327, -7.564407249984300918, -6.443844059477449093 ) ) ;
#12758 = CARTESIAN_POINT ( 'NONE',  ( -10.01549611932653860, 203.7984951890123284, 87.35113791807854966 ) ) ;
#12759 = CARTESIAN_POINT ( 'NONE',  ( 3.044812012440130555, 197.4746971517856764, 62.60113791807857098 ) ) ;
#12760 = CARTESIAN_POINT ( 'NONE',  ( 0.000000000000000000, 0.000000000000000000, -2.899999999999999911 ) ) ;
#12761 =( GEOMETRIC_REPRESENTATION_CONTEXT ( 3 ) GLOBAL_UNCERTAINTY_ASSIGNED_CONTEXT ( ( #9690 ) ) GLOBAL_UNIT_ASSIGNED_CONTEXT ( ( #16325, #6095, #15833 ) ) REPRESENTATION_CONTEXT ( 'NONE', 'WORKASPACE' ) );
#12762 = CARTESIAN_POINT ( 'NONE',  ( 9.680171189290716072, 214.0920067884432854, 21.69886208192144039 ) ) ;
#12763 = CARTESIAN_POINT ( 'NONE',  ( -8.062137200540822946, 201.0835637161416400, 29.19886208192143684 ) ) ;
#12764 = CARTESIAN_POINT ( 'NONE',  ( 75.19999999453763451, 146.4771138417591203, 11.73074641843673227 ) ) ;
#12765 = VERTEX_POINT ( 'NONE', #29293 ) ;
#12766 = CARTESIAN_POINT ( 'NONE',  ( -12.01549611932652972, 203.1486557965464499, 63.35113791807857098 ) ) ;
#12767 = CARTESIAN_POINT ( 'NONE',  ( 2.517493886308900919, 214.5937144450984420, 79.40113791807858945 ) ) ;
#12768 = CARTESIAN_POINT ( 'NONE',  ( 0.05014649552828275708, 196.4853777576173002, 40.74886208192143044 ) ) ;
#12769 = CYLINDRICAL_SURFACE ( 'NONE', #23235, 12.10452846326765020 ) ;
#12770 = VERTEX_POINT ( 'NONE', #675 ) ;
#12771 = CARTESIAN_POINT ( 'NONE',  ( -3.753561863808878130, 218.3979405102790281, 42.09886208192143897 ) ) ;
#12772 = VECTOR ( 'NONE', #28426, 1000.000000000000000 ) ;
#12773 = ORIENTED_EDGE ( 'NONE', *, *, #18971, .F. ) ;
#12774 = VERTEX_POINT ( 'NONE', #6279 ) ;
#12775 = DIRECTION ( 'NONE',  ( 0.000000000000000000, 0.000000000000000000, -1.000000000000000000 ) ) ;
#12776 = DIRECTION ( 'NONE',  ( 0.000000000000000000, 1.000000000000000000, -6.454785026890489601E-15 ) ) ;
#12777 = ORIENTED_EDGE ( 'NONE', *, *, #13635, .F. ) ;
#12778 = CARTESIAN_POINT ( 'NONE',  ( 6.500168698208129925, 211.6636982574063381, 43.70113791807857240 ) ) ;
#12779 = SURFACE_STYLE_FILL_AREA ( #325 ) ;
#12780 = CARTESIAN_POINT ( 'NONE',  ( 8.118202686958138514, 201.1607312380088501, 22.29886208192143826 ) ) ;
#12781 = CARTESIAN_POINT ( 'NONE',  ( 61.57499999726881157, 164.1591823560292198, -12.60653300113719766 ) ) ;
#12782 = VERTEX_POINT ( 'NONE', #11077 ) ;
#12783 = CARTESIAN_POINT ( 'NONE',  ( 9.443650191645208025, 207.8375535574373032, -0.8718850525427659370 ) ) ;
#12784 =( LENGTH_UNIT ( ) NAMED_UNIT ( * ) SI_UNIT ( .MILLI., .METRE. ) );
#12785 = LINE ( 'NONE', #10574, #16905 ) ;
#12786 = CARTESIAN_POINT ( 'NONE',  ( -0.05014649552828403384, 217.5146222423826714, 102.2488620819214020 ) ) ;
#12787 = CARTESIAN_POINT ( 'NONE',  ( 0.05014649552810505201, 217.5146222423826714, 37.25113791807855534 ) ) ;
#12788 =( NAMED_UNIT ( * ) PLANE_ANGLE_UNIT ( ) SI_UNIT ( $, .RADIAN. ) );
#12789 = CARTESIAN_POINT ( 'NONE',  ( -9.984503880673473830, 210.2968891136704315, 24.65113791807856103 ) ) ;
#12790 = CARTESIAN_POINT ( 'NONE',  ( 3.044812012439969795, 216.5253028482143520, 102.3988620819214361 ) ) ;
#12791 = CARTESIAN_POINT ( 'NONE',  ( 6.500168698208244500, 202.3363017425938324, 79.29886208192144181 ) ) ;
#12792 = CARTESIAN_POINT ( 'NONE',  ( 34.12499999726881583, 155.0000000000000000, 15.58253174999999402 ) ) ;
#12793 = DIRECTION ( 'NONE',  ( -0.000000000000000000, -0.000000000000000000, 1.000000000000000000 ) ) ;
#12794 = CARTESIAN_POINT ( 'NONE',  ( 9.680171189290831535, 199.9079932115568852, 8.301137918078564937 ) ) ;
#12795 = CARTESIAN_POINT ( 'NONE',  ( -63.50000000000001421, 210.0000000000000000, 0.000000000000000000 ) ) ;
#12796 = CARTESIAN_POINT ( 'NONE',  ( 50.77499999726880731, 140.1801316387863778, 4.815267126137185549 ) ) ;
#12797 = CARTESIAN_POINT ( 'NONE',  ( 6.139770520408368348, 198.4640165459539674, 53.45113791807855108 ) ) ;
#12798 = CARTESIAN_POINT ( 'NONE',  ( 32.50000000000000000, 155.0000000000000000, -6.938893903907228378E-15 ) ) ;
#12799 = CARTESIAN_POINT ( 'NONE',  ( 78.11132485994281183, 169.2658477444273331, -4.635254915624224203 ) ) ;
#12800 = CARTESIAN_POINT ( 'NONE',  ( -10.00000000000000711, 206.9523078486584495, 2.498862081921433997 ) ) ;
#12801 = CARTESIAN_POINT ( 'NONE',  ( 52.59999999453762598, 168.7903194862797420, 4.480746418436729606 ) ) ;
#12802 = ORIENTED_EDGE ( 'NONE', *, *, #11856, .T. ) ;
#12803 = CARTESIAN_POINT ( 'NONE',  ( 3.662846001190051659, 195.5725841191953691, 26.60113791807856742 ) ) ;
#12804 = CARTESIAN_POINT ( 'NONE',  ( 4.000000000000000000, 3.518949890710768802, -4.770489558936219510E-15 ) ) ;
#12805 = EDGE_CURVE ( 'NONE', #9151, #7879, #16672, .T. ) ;
#12806 = CARTESIAN_POINT ( 'NONE',  ( -8.118202686958138514, 212.8392687619910930, 8.798862081921434708 ) ) ;
#12807 = DIRECTION ( 'NONE',  ( 1.000000000000000000, 0.000000000000000000, 0.000000000000000000 ) ) ;
#12808 = ORIENTED_EDGE ( 'NONE', *, *, #4163, .F. ) ;
#12809 = CARTESIAN_POINT ( 'NONE',  ( -9.984503880673473830, 210.2968891136704315, 6.651137918078564581 ) ) ;
#12810 = CARTESIAN_POINT ( 'NONE',  ( 6.220909254589536808, 215.4770327129947702, 67.55113791807853829 ) ) ;
#12811 = ORIENTED_EDGE ( 'NONE', *, *, #14769, .F. ) ;
#12812 = CARTESIAN_POINT ( 'NONE',  ( -8.000000000000008882, 206.9523078486584780, 35.49886208192143044 ) ) ;
#12813 = DIRECTION ( 'NONE',  ( 1.000000000000000000, 0.000000000000000000, 0.000000000000000000 ) ) ;
#12814 = CARTESIAN_POINT ( 'NONE',  ( 74.27499999726880731, 160.0630714827496206, 15.58253174999999224 ) ) ;
#12815 = ORIENTED_EDGE ( 'NONE', *, *, #12896, .F. ) ;
#12816 = CARTESIAN_POINT ( 'NONE',  ( 2.517493886308900919, 214.5937144450984420, 10.40113791807856636 ) ) ;
#12817 = CARTESIAN_POINT ( 'NONE',  ( 9.736236675708031640, 199.9851607334238963, 103.2988620819214560 ) ) ;
#12818 = CARTESIAN_POINT ( 'NONE',  ( 36.27499999726881441, 160.0630714827496206, 15.58253174999999224 ) ) ;
#12819 = EDGE_LOOP ( 'NONE', ( #7224, #18965 ) ) ;
#12820 = CARTESIAN_POINT ( 'NONE',  ( 47.12499999726880873, 155.0000000000000000, -15.58253175000000823 ) ) ;
#12821 = CARTESIAN_POINT ( 'NONE',  ( 7.499999999999999112, 0.7513028741560161539, -0.02472015219302839059 ) ) ;
#12822 = CARTESIAN_POINT ( 'NONE',  ( 3.044812012440130555, 197.4746971517856764, 8.601137918078565647 ) ) ;
#12823 = EDGE_CURVE ( 'NONE', #22989, #30277, #16954, .T. ) ;
#12824 = CARTESIAN_POINT ( 'NONE',  ( -9.984503880673420539, 203.7031108863293980, 68.34886208192143897 ) ) ;
#12825 = CARTESIAN_POINT ( 'NONE',  ( 48.37499999726880873, 155.0000000000000000, 15.58253174999999402 ) ) ;
#12826 = CARTESIAN_POINT ( 'NONE',  ( -0.3755270751584372513, 206.3579517667438665, 116.9470267523194593 ) ) ;
#12827 = CARTESIAN_POINT ( 'NONE',  ( -10.01549611932653860, 203.7984951890123284, 12.35113791807856387 ) ) ;
#12828 = FACE_OUTER_BOUND ( 'NONE', #27882, .T. ) ;
#12829 = CARTESIAN_POINT ( 'NONE',  ( 66.20000000000001705, 142.6655632788954620, -8.961492836873480528 ) ) ;
#12830 = CARTESIAN_POINT ( 'NONE',  ( 8.118202686958039038, 212.8392687619912635, 100.7011379180785866 ) ) ;
#12831 = CARTESIAN_POINT ( 'NONE',  ( 111.1125082318798007, 155.0000000000000000, 0.000000000000000000 ) ) ;
#12832 = SHAPE_REPRESENTATION ( 'pad', ( #2404 ), #13844 ) ;
#12833 = CARTESIAN_POINT ( 'NONE',  ( 8.062137200540920645, 201.0835637161417822, 71.30113791807856671 ) ) ;
#12834 = CARTESIAN_POINT ( 'NONE',  ( 57.18867513459483121, 169.2658477444273331, -4.635254915624224203 ) ) ;
#12835 = DIRECTION ( 'NONE',  ( 0.000000000000000000, 0.000000000000000000, 1.000000000000000000 ) ) ;
#12836 = CARTESIAN_POINT ( 'NONE',  ( -11.98450388067341876, 203.0532714938636047, 98.34886208192145318 ) ) ;
#12837 = CARTESIAN_POINT ( 'NONE',  ( 67.82499999726881867, 168.2552932293087906, 9.630534252274372875 ) ) ;
#12838 = ORIENTED_EDGE ( 'NONE', *, *, #6031, .F. ) ;
#12839 = CARTESIAN_POINT ( 'NONE',  ( -58.50000000000002132, 194.9217985566782829, -2.500000000000000000 ) ) ;
#12840 = CARTESIAN_POINT ( 'NONE',  ( 35.09999999453762598, 150.2886644046228639, 14.49999999999999645 ) ) ;
#12841 = CARTESIAN_POINT ( 'NONE',  ( 3.662846001190051659, 195.5725841191953691, 98.60113791807857808 ) ) ;
#12842 = CARTESIAN_POINT ( 'NONE',  ( 92.60208470531341618, 155.0000000000000000, -12.10452846326766441 ) ) ;
#12843 = ADVANCED_FACE ( 'NONE', ( #24514 ), #10910, .T. ) ;
#12844 = ORIENTED_EDGE ( 'NONE', *, *, #3675, .F. ) ;
#12845 = CARTESIAN_POINT ( 'NONE',  ( 6.220909254589680693, 198.5229672870052582, 82.44886208192141908 ) ) ;
#12846 = CARTESIAN_POINT ( 'NONE',  ( -7.375838497908014268, 196.7627149292498530, 20.04886208192143471 ) ) ;
#12847 = CARTESIAN_POINT ( 'NONE',  ( 115.4999999999999858, 129.0854607986834424, -100.8678580070900921 ) ) ;
#12848 = EDGE_CURVE ( 'NONE', #13192, #8276, #8675, .T. ) ;
#12849 = CARTESIAN_POINT ( 'NONE',  ( 6.139770520408368348, 198.4640165459539674, 41.45113791807857240 ) ) ;
#12850 = EDGE_LOOP ( 'NONE', ( #1601, #17785, #14942, #26634, #9662, #33348 ) ) ;
#12851 = CARTESIAN_POINT ( 'NONE',  ( -8.000000000000008882, 206.9523078486584780, 2.498862081921435330 ) ) ;
#12852 = CONICAL_SURFACE ( 'NONE', #31881, 6.500000000000000888, 0.8987552595851582282 ) ;
#12853 = EDGE_CURVE ( 'NONE', #8611, #16190, #21287, .T. ) ;
#12854 = PLANE ( 'NONE',  #7818 ) ;
#12855 = ORIENTED_EDGE ( 'NONE', *, *, #3735, .T. ) ;
#12856 = CARTESIAN_POINT ( 'NONE',  ( 2.517493886309087436, 199.4062855549015865, 82.59886208192143897 ) ) ;
#12857 = ORIENTED_EDGE ( 'NONE', *, *, #22521, .T. ) ;
#12858 = CARTESIAN_POINT ( 'NONE',  ( 0.3999999999999975797, 0.000000000000000000, 0.000000000000000000 ) ) ;
#12859 = ORIENTED_EDGE ( 'NONE', *, *, #6440, .T. ) ;
#12860 = CARTESIAN_POINT ( 'NONE',  ( 81.51132485994280330, 146.1832212156128890, -12.13525491562423042 ) ) ;
#12861 = CARTESIAN_POINT ( 'NONE',  ( 4.984841277089725686, 213.7757310962907411, 58.55113791807858092 ) ) ;
#12862 = CARTESIAN_POINT ( 'NONE',  ( 80.12499999726881583, 155.0000000000000000, 15.58253174999999402 ) ) ;
#12863 = EDGE_CURVE ( 'NONE', #13425, #32876, #16504, .T. ) ;
#12864 = CARTESIAN_POINT ( 'NONE',  ( -31.74999999999995737, 4.286263797015736595E-16, -3.500000000000000000 ) ) ;
#12865 = CARTESIAN_POINT ( 'NONE',  ( -6.444103211791042618, 211.7408657792732356, 87.80113791807858092 ) ) ;
#12866 = DIRECTION ( 'NONE',  ( 1.000000000000000000, 0.000000000000000000, 0.000000000000000000 ) ) ;
#12867 = CARTESIAN_POINT ( 'NONE',  ( 48.30000000000000426, 146.4771138417591203, -11.73074641843674470 ) ) ;
#12868 = CARTESIAN_POINT ( 'NONE',  ( 6.500168698208244500, 202.3363017425938324, 67.29886208192144181 ) ) ;
#12869 = CARTESIAN_POINT ( 'NONE',  ( 115.4999999999999858, 155.0000000000000000, 100.0000000000000000 ) ) ;
#12870 = EDGE_CURVE ( 'NONE', #25544, #866, #16924, .T. ) ;
#12871 = VECTOR ( 'NONE', #13968, 1000.000000000000000 ) ;
#12872 = CARTESIAN_POINT ( 'NONE',  ( 52.72499999726881015, 140.1801316387863778, -4.815267126137194431 ) ) ;
#12873 = CARTESIAN_POINT ( 'NONE',  ( 6.139770520408367460, 198.4640165459539389, -0.5488620819214342639 ) ) ;
#12874 = CARTESIAN_POINT ( 'NONE',  ( -64.96121601855533356, 1.809269760319424769, -19.53878398144470907 ) ) ;
#12875 = CARTESIAN_POINT ( 'NONE',  ( 59.92499999726881299, 164.1591823560292198, 12.60653300113718167 ) ) ;
#12876 = CARTESIAN_POINT ( 'NONE',  ( 70.97499999726881015, 140.1801316387863778, -4.815267126137194431 ) ) ;
#12877 = CARTESIAN_POINT ( 'NONE',  ( -0.05014649552807705357, 194.3824533091408000, 65.75113791807856956 ) ) ;
#12878 = DIRECTION ( 'NONE',  ( -1.000000000000000000, 0.000000000000000000, 0.000000000000000000 ) ) ;
#12879 = CARTESIAN_POINT ( 'NONE',  ( 7.456977232089302632, 217.1783343296989131, 13.55113791807856849 ) ) ;
#12880 = CARTESIAN_POINT ( 'NONE',  ( -10.01549611932653860, 203.7984951890123000, 90.35113791807857808 ) ) ;
#12881 = CONICAL_SURFACE ( 'NONE', #17227, 12.00000000000000355, 0.7853981633974503884 ) ;
#12882 = CARTESIAN_POINT ( 'NONE',  ( -3.662846001189865142, 195.5725841191952838, 49.89886208192143613 ) ) ;
#12883 = CARTESIAN_POINT ( 'NONE',  ( 3.135527875058981895, 197.5041725223112792, 58.59886208192143897 ) ) ;
#12884 = CARTESIAN_POINT ( 'NONE',  ( -7.777900015783941967, -4.169681370001537601, -7.928862157988302073 ) ) ;
#12885 = CARTESIAN_POINT ( 'NONE',  ( -9.680171189290831535, 214.0920067884431148, 99.80113791807858092 ) ) ;
#12886 = CARTESIAN_POINT ( 'NONE',  ( 34.08867513459483689, 142.2402378747194405, 9.270509831248432420 ) ) ;
#12887 = CARTESIAN_POINT ( 'NONE',  ( 9.984503880673470277, 203.7031108863295401, 14.15113791807856458 ) ) ;
#12888 = CARTESIAN_POINT ( 'NONE',  ( -3.135527875058982783, 216.4958274776886924, 72.09886208192143897 ) ) ;
#12889 = ORIENTED_EDGE ( 'NONE', *, *, #33460, .F. ) ;
#12890 = CARTESIAN_POINT ( 'NONE',  ( 12.01549611932659367, 203.1486557965466773, 82.14886208192143613 ) ) ;
#12891 = CARTESIAN_POINT ( 'NONE',  ( -8.062137200540920645, 212.9164362838581894, 90.80113791807858092 ) ) ;
#12892 = ORIENTED_EDGE ( 'NONE', *, *, #22246, .F. ) ;
#12893 = CARTESIAN_POINT ( 'NONE',  ( 74.97499999726881015, 140.1801316387863778, -4.815267126137194431 ) ) ;
#12894 = CARTESIAN_POINT ( 'NONE',  ( -7.984503880673422316, 204.3529502787951628, 50.34886208192144608 ) ) ;
#12895 = EDGE_LOOP ( 'NONE', ( #5113, #21631, #16611, #10521 ) ) ;
#12896 = EDGE_CURVE ( 'NONE', #17833, #1148, #22625, .T. ) ;
#12897 = VECTOR ( 'NONE', #26052, 1000.000000000000000 ) ;
#12898 = CARTESIAN_POINT ( 'NONE',  ( 68.52499999726880731, 140.1801316387863778, 4.815267126137185549 ) ) ;
#12899 = CARTESIAN_POINT ( 'NONE',  ( 6.500000000000301981, 0.6542365398607151716, -6.055391205186719361 ) ) ;
#12900 = CARTESIAN_POINT ( 'NONE',  ( -56.32919368135717519, 194.9806731544236982, 1.250698461946182505 ) ) ;
#12901 = CARTESIAN_POINT ( 'NONE',  ( 61.02499999726880020, 149.9369285172503510, -15.58253175000000823 ) ) ;
#12902 = ADVANCED_FACE ( 'NONE', ( #7135, #9184, #4230, #6792, #4578 ), #27236, .F. ) ;
#12903 = CARTESIAN_POINT ( 'NONE',  ( -7.500000000000698996, 1.613867362005801054, -7.450195926347907616 ) ) ;
#12904 = CARTESIAN_POINT ( 'NONE',  ( -8.062137200540822946, 201.0835637161416400, 53.19886208192143329 ) ) ;
#12905 = ORIENTED_EDGE ( 'NONE', *, *, #6476, .T. ) ;
#12906 = CARTESIAN_POINT ( 'NONE',  ( -125.0000000000000000, 0.000000000000000000, 35.00200000000000244 ) ) ;
#12907 = DIRECTION ( 'NONE',  ( 0.000000000000000000, 0.000000000000000000, -1.000000000000000000 ) ) ;
#12908 = CARTESIAN_POINT ( 'NONE',  ( 2.517493886309087436, 199.4062855549015865, 34.59886208192143897 ) ) ;
#12909 = EDGE_CURVE ( 'NONE', #14059, #22749, #18193, .T. ) ;
#12910 = CARTESIAN_POINT ( 'NONE',  ( 8.062137200540920645, 201.0835637161417822, 74.30113791807858092 ) ) ;
#12911 = CARTESIAN_POINT ( 'NONE',  ( 45.58867513459481557, 163.8167787843871110, 12.13525491562421621 ) ) ;
#12912 = CARTESIAN_POINT ( 'NONE',  ( 9.984503880673470277, 203.7031108863295401, 53.15113791807857524 ) ) ;
#12913 = CONTEXT_DEPENDENT_SHAPE_REPRESENTATION ( #2922, #3008 ) ;
#12914 = CARTESIAN_POINT ( 'NONE',  ( -6.139770520408369237, 215.5359834540460042, 27.95113791807856174 ) ) ;
#12915 = CARTESIAN_POINT ( 'NONE',  ( -2.517493886308901807, 199.4062855549015012, 11.90113791807856813 ) ) ;
#12916 = CARTESIAN_POINT ( 'NONE',  ( 87.07499999726880446, 141.7447067706911810, -9.630534252274387086 ) ) ;
#12917 = CARTESIAN_POINT ( 'NONE',  ( -6.830473686658677934E-14, -4.041451884327390331, -0.3126073911696551910 ) ) ;
#12918 = CARTESIAN_POINT ( 'NONE',  ( 39.22499999726881015, 160.0630714827496206, -15.58253175000000823 ) ) ;
#12919 = CARTESIAN_POINT ( 'NONE',  ( 7.456977232089302632, 217.1783343296989131, 40.55113791807856671 ) ) ;
#12920 = FACE_BOUND ( 'NONE', #4206, .T. ) ;
#12921 = CARTESIAN_POINT ( 'NONE',  ( -6.220909254589537696, 198.5229672870051161, 81.05113791807856671 ) ) ;
#12922 = CARTESIAN_POINT ( 'NONE',  ( 6.139770520408367460, 198.4640165459539389, 56.45113791807857950 ) ) ;
#12923 = DIRECTION ( 'NONE',  ( 0.4999999999999958367, 0.000000000000000000, -0.8660254037844410391 ) ) ;
#12924 = CIRCLE ( 'NONE', #7487, 4.171999999999999709 ) ;
#12925 = CARTESIAN_POINT ( 'NONE',  ( -7.456977232089471386, 217.1783343296987709, 20.94886208192143684 ) ) ;
#12926 = CIRCLE ( 'NONE', #13930, 8.624472924841564136 ) ;
#12927 = CARTESIAN_POINT ( 'NONE',  ( -10.01549611932659545, 210.2015048109875011, 32.64886208192143613 ) ) ;
#12928 = CARTESIAN_POINT ( 'NONE',  ( 73.79999999453762882, 146.4771138417591203, -11.73074641843674470 ) ) ;
#12929 = CARTESIAN_POINT ( 'NONE',  ( 3.662846001190051659, 195.5725841191953691, 68.60113791807857808 ) ) ;
#12930 = CARTESIAN_POINT ( 'NONE',  ( -8.000000000000008882, 207.0476921513413515, 81.50113791807856956 ) ) ;
#12931 = CARTESIAN_POINT ( 'NONE',  ( -8.118202686958138514, 212.8392687619910930, 38.79886208192143471 ) ) ;
#12932 = CARTESIAN_POINT ( 'NONE',  ( -58.50000000000001421, -88.00000000000000000, -20.00000000000000000 ) ) ;
#12933 = CONICAL_SURFACE ( 'NONE', #7497, 32.10452846326769816, 1.466076571675243523 ) ;
#12934 = VERTEX_POINT ( 'NONE', #25024 ) ;
#12935 = CARTESIAN_POINT ( 'NONE',  ( 9.680171189290716072, 214.0920067884432854, 54.69886208192144039 ) ) ;
#12936 = ORIENTED_EDGE ( 'NONE', *, *, #10837, .F. ) ;
#12937 = ORIENTED_EDGE ( 'NONE', *, *, #2955, .T. ) ;
#12938 = ADVANCED_FACE ( 'NONE', ( #14285 ), #1677, .T. ) ;
#12939 = DIRECTION ( 'NONE',  ( 1.000000000000000000, 0.000000000000000000, 0.000000000000000000 ) ) ;
#12940 = LINE ( 'NONE', #21104, #30126 ) ;
#12941 = EDGE_LOOP ( 'NONE', ( #22343, #817, #13471, #28985 ) ) ;
#12942 =( BOUNDED_CURVE ( )  B_SPLINE_CURVE ( 2, ( #12352, #7595, #28021, #33307, #15415, #12186, #20363, #2475, #17977, #25638, #4686 ),
 .UNSPECIFIED., .F., .F. ) 
 B_SPLINE_CURVE_WITH_KNOTS ( ( 3, 2, 2, 2, 2, 3 ),
 ( 0.000000000000000000, 0.003571428571428599073, 0.007142857142857198145, 0.01071428571428579765, 0.01428571428571439629, 0.01785714285714299493 ),
 .UNSPECIFIED. ) 
 CURVE ( )  GEOMETRIC_REPRESENTATION_ITEM ( )  RATIONAL_B_SPLINE_CURVE ( ( 1.000000000000000000, 0.9510565162951534202, 1.000000000000000000, 0.9510565162951534202, 1.000000000000000000, 0.9510565162951534202, 1.000000000000000000, 0.9510565162951534202, 1.000000000000000000, 0.9510565162951515328, 1.000000000000001998 ) ) 
 REPRESENTATION_ITEM ( '' )  );
#12943 = CARTESIAN_POINT ( 'NONE',  ( -2.517493886308901807, 199.4062855549015012, 38.90113791807856813 ) ) ;
#12944 = CIRCLE ( 'NONE', #25439, 1.000000000000000888 ) ;
#12945 = PRODUCT_DEFINITION ( 'UNKNOWN', '', #27867, #14186 ) ;
#12946 = EDGE_CURVE ( 'NONE', #30536, #30105, #30473, .T. ) ;
#12947 = CARTESIAN_POINT ( 'NONE',  ( 81.81132485994281467, 159.8737954434937478, -14.99999999999993072 ) ) ;
#12948 = AXIS2_PLACEMENT_3D ( 'NONE', #32784, #24625, #22394 ) ;
#12949 = CARTESIAN_POINT ( 'NONE',  ( 10.00000000000000711, 207.0476921513415220, 24.99886208192143400 ) ) ;
#12950 = CARTESIAN_POINT ( 'NONE',  ( 62.47499999726881015, 149.9369285172503510, 15.58253174999999580 ) ) ;
#12951 = ORIENTED_EDGE ( 'NONE', *, *, #3972, .F. ) ;
#12952 = FACE_OUTER_BOUND ( 'NONE', #11379, .T. ) ;
#12953 = CONICAL_SURFACE ( 'NONE', #24910, 27.50000000000000355, 1.047197551196595411 ) ;
#12954 = MANIFOLD_SOLID_BREP ( 'Hex', #2552 ) ;
#12955 = CARTESIAN_POINT ( 'NONE',  ( -7.640563834021360018E-16, -9.147862274876560562, -8.047472243342937759 ) ) ;
#12956 = CARTESIAN_POINT ( 'NONE',  ( -6.500168698208244500, 211.6636982574061676, 2.798862081921434708 ) ) ;
#12957 = CARTESIAN_POINT ( 'NONE',  ( 3.135527875058820690, 216.4958274776887492, 46.40113791807857524 ) ) ;
#12958 = CARTESIAN_POINT ( 'NONE',  ( -3.135527875058821579, 197.5041725223112223, 29.90113791807856813 ) ) ;
#12959 = DIRECTION ( 'NONE',  ( -1.000000000000000000, -0.000000000000000000, -0.000000000000000000 ) ) ;
#12960 = AXIS2_PLACEMENT_3D ( 'NONE', #9907, #27957, #19619 ) ;
#12961 = APPLICATION_PROTOCOL_DEFINITION ( 'draft international standard', 'automotive_design', 1998, #14847 ) ;
#12962 = CARTESIAN_POINT ( 'NONE',  ( 2.426778023690075337, 214.6231898156240447, 96.39886208192146455 ) ) ;
#12963 = CARTESIAN_POINT ( 'NONE',  ( 83.50000000000000000, 155.0000000000000000, 14.49999999999999467 ) ) ;
#12964 = CARTESIAN_POINT ( 'NONE',  ( 8.542937654374687995, 0.000000000000000000, -6.800000000000000711 ) ) ;
#12965 = CARTESIAN_POINT ( 'NONE',  ( 12.00000000000000711, 206.9523078486586485, 11.00113791807856600 ) ) ;
#12966 = CARTESIAN_POINT ( 'NONE',  ( 47.88867513459484115, 150.1262045565062806, 14.99999999999992006 ) ) ;
#12967 = CARTESIAN_POINT ( 'NONE',  ( 55.87499999726882294, 171.3844434931184253, -7.942151717890132712E-15 ) ) ;
#12968 = B_SPLINE_CURVE_WITH_KNOTS ( 'NONE', 3,
 ( #16052, #13496, #7570, #33621, #7732, #18118, #2621, #5166 ),
 .UNSPECIFIED., .F., .F.,
 ( 4, 2, 2, 4 ),
 ( 0.04438889715320012280, 0.04840678451617880934, 0.05242467187915750282, 0.06046044660511487590 ),
 .UNSPECIFIED. ) ;
#12969 = CARTESIAN_POINT ( 'NONE',  ( 10.00000000000000711, 206.9523078486586201, 59.00113791807857666 ) ) ;
#12970 = CARTESIAN_POINT ( 'NONE',  ( 35.71132485994280614, 155.0000000000000000, -15.00000000000002487 ) ) ;
#12971 = B_SPLINE_CURVE_WITH_KNOTS ( 'NONE', 3,
 ( #24216, #1212, #16879, #21997, #13652, #879, #27274, #1053, #29160 ),
 .UNSPECIFIED., .F., .F.,
 ( 4, 2, 1, 2, 4 ),
 ( 0.000000000000000000, 0.002165063509461097498, 0.004330127018922194995, 0.006495190528383292493, 0.008660254037844389990 ),
 .UNSPECIFIED. ) ;
#12972 = DIRECTION ( 'NONE',  ( 1.000000000000000000, 0.000000000000000000, 0.000000000000000000 ) ) ;
#12973 = CARTESIAN_POINT ( 'NONE',  ( 2.000000000000000000, -0.8865213383406685965, 1.535500000000000531 ) ) ;
#12974 = CARTESIAN_POINT ( 'NONE',  ( 55.79999999453762882, 146.4771138417591203, -11.73074641843674470 ) ) ;
#12975 = VERTEX_POINT ( 'NONE', #1849 ) ;
#12976 = CARTESIAN_POINT ( 'NONE',  ( -3.662846001190052991, 218.4274158808045740, 40.10113791807856387 ) ) ;
#12977 = AXIS2_PLACEMENT_3D ( 'NONE', #22626, #14454, #1678 ) ;
#12978 = LINE ( 'NONE', #12804, #21952 ) ;
#12979 = CARTESIAN_POINT ( 'NONE',  ( 3.135527875058981895, 197.5041725223112792, 13.59886208192143719 ) ) ;
#12980 = CIRCLE ( 'NONE', #29278, 3.299999999999999822 ) ;
#12981 = CARTESIAN_POINT ( 'NONE',  ( 10.00000000000000888, 207.8294911128234617, -1.040744497668167012 ) ) ;
#12982 = VERTEX_POINT ( 'NONE', #19738 ) ;
#12983 = CARTESIAN_POINT ( 'NONE',  ( -3.044812012440131443, 216.5253028482142952, 7.101137918078566535 ) ) ;
#12984 = CARTESIAN_POINT ( 'NONE',  ( -6.220909254589537696, 198.5229672870051161, 69.05113791807858092 ) ) ;
#12985 = ORIENTED_EDGE ( 'NONE', *, *, #30843, .T. ) ;
#12986 = CARTESIAN_POINT ( 'NONE',  ( 8.015496119326595448, 204.4483345814782638, 34.14886208192144323 ) ) ;
#12987 = VECTOR ( 'NONE', #20204, 1000.000000000000114 ) ;
#12988 = CARTESIAN_POINT ( 'NONE',  ( 9.092171885314263236, -26.50489691992491359, -17.71727689882190404 ) ) ;
#12989 = ORIENTED_EDGE ( 'NONE', *, *, #31007, .T. ) ;
#12990 = CARTESIAN_POINT ( 'NONE',  ( -4.984841277089726574, 200.2242689037092305, 12.05113791807856849 ) ) ;
#12991 = CARTESIAN_POINT ( 'NONE',  ( -11.98450388067341876, 203.0532714938636047, 95.34886208192143897 ) ) ;
#12992 = CARTESIAN_POINT ( 'NONE',  ( 41.77499999726881441, 169.8198683612136222, -4.815267126137197984 ) ) ;
#12993 = ORIENTED_EDGE ( 'NONE', *, *, #2095, .F. ) ;
#12994 = CARTESIAN_POINT ( 'NONE',  ( 48.12499999726880873, 155.0000000000000000, 15.58253174999999402 ) ) ;
#12995 = CARTESIAN_POINT ( 'NONE',  ( 127.5000000000000000, 81.56696077377769427, 76.47359838532574372 ) ) ;
#12996 = CARTESIAN_POINT ( 'NONE',  ( 10.01549611932653860, 210.2015048109876716, 7.851137918078566535 ) ) ;
#12997 = CARTESIAN_POINT ( 'NONE',  ( 3.135527875058981895, 197.5041725223112792, 85.59886208192143897 ) ) ;
#12998 = CARTESIAN_POINT ( 'NONE',  ( 55.87499999726882294, 171.3844434931184253, -7.942151717890132712E-15 ) ) ;
#12999 = LINE ( 'NONE', #7562, #13405 ) ;
#13000 = CARTESIAN_POINT ( 'NONE',  ( 0.05014649552810505201, 217.5146222423826714, 16.25113791807856600 ) ) ;
#13001 = CARTESIAN_POINT ( 'NONE',  ( 2.000000000000000000, -0.8865213383406685965, 1.535500000000000531 ) ) ;
#13002 = VECTOR ( 'NONE', #8454, 1000.000000000000114 ) ;
#13003 = VECTOR ( 'NONE', #7933, 1000.000000000000000 ) ;
#13004 = CARTESIAN_POINT ( 'NONE',  ( 64.50000000000000000, 155.0000000000000000, -14.50000000000000711 ) ) ;
#13005 = CARTESIAN_POINT ( 'NONE',  ( 0.05014649552810505201, 217.5146222423826714, 97.25113791807854113 ) ) ;
#13006 = CARTESIAN_POINT ( 'NONE',  ( 38.68867513459483121, 150.1262045565064227, -15.00000000000002665 ) ) ;
#13007 = CARTESIAN_POINT ( 'NONE',  ( 3.135527875058820690, 216.4958274776887492, 85.40113791807857524 ) ) ;
#13008 = LINE ( 'NONE', #10122, #10226 ) ;
#13009 = DIRECTION ( 'NONE',  ( 0.000000000000000000, 0.000000000000000000, 1.000000000000000000 ) ) ;
#13010 = CARTESIAN_POINT ( 'NONE',  ( -12.00000000000000711, 206.9523078486584780, 95.49886208192144466 ) ) ;
#13011 = VECTOR ( 'NONE', #30015, 1000.000000000000000 ) ;
#13012 = CARTESIAN_POINT ( 'NONE',  ( 70.02499999726879309, 160.0630714827496206, 15.58253174999999402 ) ) ;
#13013 = ORIENTED_EDGE ( 'NONE', *, *, #25144, .F. ) ;
#13014 = CARTESIAN_POINT ( 'NONE',  ( -60.87189664283175006, 194.9921494935721569, 0.8066102793772919055 ) ) ;
#13015 = CARTESIAN_POINT ( 'NONE',  ( 35.49999999453762456, 139.7537977485451393, -4.138211985947621020E-15 ) ) ;
#13016 = CARTESIAN_POINT ( 'NONE',  ( 0.05014649552807549926, 219.6175466908591716, 94.25113791807859798 ) ) ;
#13017 = CARTESIAN_POINT ( 'NONE',  ( -125.0000000000000000, 0.000000000000000000, -35.00000000000000000 ) ) ;
#13018 = ORIENTED_EDGE ( 'NONE', *, *, #19905, .T. ) ;
#13019 = CARTESIAN_POINT ( 'NONE',  ( 9.984503880673420539, 210.2968891136705736, 84.84886208192143897 ) ) ;
#13020 = CARTESIAN_POINT ( 'NONE',  ( 12.00000000000000711, 207.0476921513415220, 21.99886208192143400 ) ) ;
#13021 = CARTESIAN_POINT ( 'NONE',  ( 10.20891672561132424, 208.8253170565643302, -1.573594014082846382 ) ) ;
#13022 = AXIS2_PLACEMENT_3D ( 'NONE', #24945, #9441, #1943 ) ;
#13023 = CARTESIAN_POINT ( 'NONE',  ( 9.984503880673470277, 203.7031108863295401, 38.15113791807856813 ) ) ;
#13024 = EDGE_LOOP ( 'NONE', ( #9532, #23621, #28052, #19248 ) ) ;
#13025 = CARTESIAN_POINT ( 'NONE',  ( 6.500168698208244500, 202.3363017425938324, 4.298862081921435596 ) ) ;
#13026 = CARTESIAN_POINT ( 'NONE',  ( 8.399999999999998579, 0.000000000000000000, 0.000000000000000000 ) ) ;
#13027 = VERTEX_POINT ( 'NONE', #17180 ) ;
#13028 = CARTESIAN_POINT ( 'NONE',  ( 8.015496119326595448, 204.4483345814782638, 91.14886208192143613 ) ) ;
#13029 = EDGE_LOOP ( 'NONE', ( #4012, #12056, #13560, #33034 ) ) ;
#13030 = CARTESIAN_POINT ( 'NONE',  ( 7.984503880673485376, 204.3529502787953902, 35.15113791807856103 ) ) ;
#13031 = CARTESIAN_POINT ( 'NONE',  ( 56.71132485994280614, 155.0000000000000000, 15.00000000000001243 ) ) ;
#13032 = ORIENTED_EDGE ( 'NONE', *, *, #16789, .T. ) ;
#13033 = CARTESIAN_POINT ( 'NONE',  ( 6.658902113225075858, 5.287118297641098863, -7.776713651267108673 ) ) ;
#13034 = CARTESIAN_POINT ( 'NONE',  ( 81.72499999726881015, 169.8198683612136222, 4.815267126137181997 ) ) ;
#13035 = CARTESIAN_POINT ( 'NONE',  ( 117.5000000000000000, 102.0000000000001990, 91.79869280115065067 ) ) ;
#13036 = CARTESIAN_POINT ( 'NONE',  ( -4.984841277089726574, 200.2242689037092305, 87.05113791807856671 ) ) ;
#13037 = CARTESIAN_POINT ( 'NONE',  ( 3.096526599377912525, -6.872473572140722631, -5.976664475826341615E-15 ) ) ;
#13038 = EDGE_CURVE ( 'NONE', #31786, #12471, #10595, .T. ) ;
#13039 =( LENGTH_UNIT ( ) NAMED_UNIT ( * ) SI_UNIT ( .MILLI., .METRE. ) );
#13040 = CARTESIAN_POINT ( 'NONE',  ( 49.70000000000000284, 146.4771138417591203, 11.73074641843673227 ) ) ;
#13041 = CARTESIAN_POINT ( 'NONE',  ( 4.984841277089891776, 200.2242689037093726, 64.44886208192143329 ) ) ;
#13042 = VECTOR ( 'NONE', #19623, 1000.000000000000000 ) ;
#13043 = CARTESIAN_POINT ( 'NONE',  ( 27.50000000000000711, -5.348566131067986618, -0.2306174136865334345 ) ) ;
#13044 = CARTESIAN_POINT ( 'NONE',  ( 54.42499999726881299, 141.7447067706911810, 9.630534252274376428 ) ) ;
#13045 = CARTESIAN_POINT ( 'NONE',  ( 119.7500000000000000, 3.125910954823619074E-14, 35.00000599999999906 ) ) ;
#13046 = CARTESIAN_POINT ( 'NONE',  ( -64.50000000000000000, 2.605762844159070557, -20.00000000000000000 ) ) ;
#13047 = CARTESIAN_POINT ( 'NONE',  ( 55.72499999726881015, 169.8198683612136222, 4.815267126137181997 ) ) ;
#13048 = CARTESIAN_POINT ( 'NONE',  ( 71.87499999726881583, 171.3844434931184253, -7.942151717890132712E-15 ) ) ;
#13049 = CARTESIAN_POINT ( 'NONE',  ( 3.662846001190051659, 195.5725841191953691, 71.60113791807857808 ) ) ;
#13050 = DIRECTION ( 'NONE',  ( -1.000000000000000000, -0.000000000000000000, 0.000000000000000000 ) ) ;
#13051 = CARTESIAN_POINT ( 'NONE',  ( 12.01549611932652972, 210.8513442034534933, 13.85113791807856742 ) ) ;
#13052 = CARTESIAN_POINT ( 'NONE',  ( -8.062137200540920645, 212.9164362838581894, 84.80113791807856671 ) ) ;
#13053 = CARTESIAN_POINT ( 'NONE',  ( 54.78867513459483263, 155.0000000000000000, -15.00000000000002487 ) ) ;
#13054 = CARTESIAN_POINT ( 'NONE',  ( -3.753561863808878130, 218.3979405102790281, 51.09886208192143897 ) ) ;
#13055 = CARTESIAN_POINT ( 'NONE',  ( -10.01549611932659545, 210.2015048109875011, 59.64886208192143613 ) ) ;
#13056 = CARTESIAN_POINT ( 'NONE',  ( 9.736236675707914401, 214.0148392665762458, 100.7011379180785866 ) ) ;
#13057 = CARTESIAN_POINT ( 'NONE',  ( -67.50001199999999812, 166.2340547598724356, 12.80757580047019495 ) ) ;
#13058 = CARTESIAN_POINT ( 'NONE',  ( -6.139770520408369237, 215.5359834540460042, 12.95113791807856352 ) ) ;
#13059 = CARTESIAN_POINT ( 'NONE',  ( -0.05014649552828403384, 217.5146222423826714, 75.24886208192144466 ) ) ;
#13060 = ORIENTED_EDGE ( 'NONE', *, *, #6602, .F. ) ;
#13061 = CARTESIAN_POINT ( 'NONE',  ( -11.98450388067341876, 203.0532714938636047, 80.34886208192143897 ) ) ;
#13062 = CARTESIAN_POINT ( 'NONE',  ( 3.044812012440130555, 197.4746971517856764, 95.60113791807857808 ) ) ;
#13063 = ORIENTED_EDGE ( 'NONE', *, *, #5983, .T. ) ;
#13064 =( LENGTH_UNIT ( ) NAMED_UNIT ( * ) SI_UNIT ( .MILLI., .METRE. ) );
#13065 = CARTESIAN_POINT ( 'NONE',  ( -2.426778023690076225, 199.3768101843759553, 64.89886208192143613 ) ) ;
#13066 = EDGE_CURVE ( 'NONE', #15536, #10922, #20628, .T. ) ;
#13067 = ORIENTED_EDGE ( 'NONE', *, *, #18228, .T. ) ;
#13068 = CARTESIAN_POINT ( 'NONE',  ( 68.42499999726881299, 141.7447067706911810, 9.630534252274376428 ) ) ;
#13069 = DIRECTION ( 'NONE',  ( -1.000000000000000000, 0.000000000000000000, 0.000000000000000000 ) ) ;
#13070 = CARTESIAN_POINT ( 'NONE',  ( -56.97195197156149504, 194.9507991595696694, 1.985452284598899553 ) ) ;
#13071 = CARTESIAN_POINT ( 'NONE',  ( 63.32499999726881867, 164.1591823560292198, -12.60653300113719766 ) ) ;
#13072 = DIRECTION ( 'NONE',  ( -1.000000000000000000, -0.000000000000000000, -0.000000000000000000 ) ) ;
#13073 = EDGE_CURVE ( 'NONE', #5826, #734, #252, .T. ) ;
#13074 = CARTESIAN_POINT ( 'NONE',  ( -10.00000000000000711, 206.9523078486584495, 50.49886208192143044 ) ) ;
#13075 = AXIS2_PLACEMENT_3D ( 'NONE', #14121, #27070, #843 ) ;
#13076 = ORIENTED_EDGE ( 'NONE', *, *, #28058, .F. ) ;
#13077 = FACE_OUTER_BOUND ( 'NONE', #12587, .T. ) ;
#13078 = CARTESIAN_POINT ( 'NONE',  ( 89.50000000000001421, 155.0000000000000000, 13.00000000000001066 ) ) ;
#13079 = CARTESIAN_POINT ( 'NONE',  ( -6.444103211790928043, 202.2591342207265939, 32.19886208192144039 ) ) ;
#13080 = CARTESIAN_POINT ( 'NONE',  ( -10.01549611932653860, 203.7984951890123284, 75.35113791807853545 ) ) ;
#13081 = CARTESIAN_POINT ( 'NONE',  ( 0.000000000000000000, 0.000000000000000000, -8.499999999999998224 ) ) ;
#13082 = CARTESIAN_POINT ( 'NONE',  ( 8.062137200540920645, 201.0835637161417822, 53.30113791807857382 ) ) ;
#13083 = ADVANCED_FACE ( 'NONE', ( #7814 ), #31147, .F. ) ;
#13084 = CARTESIAN_POINT ( 'NONE',  ( 6.139770520408368348, 198.4640165459539674, 32.45113791807856529 ) ) ;
#13085 = CARTESIAN_POINT ( 'NONE',  ( -2.517493886308901807, 199.4062855549015012, 17.90113791807856458 ) ) ;
#13086 = CARTESIAN_POINT ( 'NONE',  ( 87.43602562408077006, 158.0897711082857882, -15.58253175000000468 ) ) ;
#13087 = DIRECTION ( 'NONE',  ( -0.000000000000000000, -0.000000000000000000, 1.000000000000000000 ) ) ;
#13088 = CARTESIAN_POINT ( 'NONE',  ( 38.32499999726881157, 145.8408176439707802, 12.60653300113718345 ) ) ;
#13089 = CARTESIAN_POINT ( 'NONE',  ( 0.05014649552807549926, 219.6175466908591716, 40.25113791807856245 ) ) ;
#13090 = CARTESIAN_POINT ( 'NONE',  ( 6.270061300899935297, -4.268872906156509828, -6.443866470201760954 ) ) ;
#13091 = CARTESIAN_POINT ( 'NONE',  ( 8.062137200540920645, 201.0835637161417822, 83.30113791807858092 ) ) ;
#13092 = CARTESIAN_POINT ( 'NONE',  ( -8.062137200540920645, 212.9164362838581894, 54.80113791807857382 ) ) ;
#13093 = CARTESIAN_POINT ( 'NONE',  ( 3.662846001189864698, 218.4274158808046593, 21.39886208192143613 ) ) ;
#13094 = CARTESIAN_POINT ( 'NONE',  ( -3.044812012439970683, 197.4746971517856196, 25.89886208192143613 ) ) ;
#13095 = CARTESIAN_POINT ( 'NONE',  ( 80.99999999453763166, 155.0000000000000000, 14.49999999999999467 ) ) ;
#13096 = CARTESIAN_POINT ( 'NONE',  ( -12.00000000000000711, 207.0476921513413515, 69.50113791807856956 ) ) ;
#13097 = CARTESIAN_POINT ( 'NONE',  ( -8.015496119326531499, 204.4483345814780364, 87.35113791807857808 ) ) ;
#13098 = EDGE_CURVE ( 'NONE', #23251, #1081, #3035, .T. ) ;
#13099 = CARTESIAN_POINT ( 'NONE',  ( 8.062137200540822946, 212.9164362838583315, 48.69886208192144039 ) ) ;
#13100 = CARTESIAN_POINT ( 'NONE',  ( 0.000000000000000000, 1.773042676681340968, -2.276824562219559311E-15 ) ) ;
#13101 = VERTEX_POINT ( 'NONE', #2863 ) ;
#13102 = CARTESIAN_POINT ( 'NONE',  ( 11.98450388067341876, 210.9467285061363953, 51.84886208192144608 ) ) ;
#13103 = AXIS2_PLACEMENT_3D ( 'NONE', #21448, #6097, #19391 ) ;
#13104 = ORIENTED_EDGE ( 'NONE', *, *, #25390, .F. ) ;
#13105 = ADVANCED_FACE ( 'NONE', ( #17862, #2534 ), #20925, .T. ) ;
#13106 = ORIENTED_EDGE ( 'NONE', *, *, #20817, .F. ) ;
#13107 = CARTESIAN_POINT ( 'NONE',  ( -7.908030677224553884, 3.059924800338342799, -7.792662696733364314 ) ) ;
#13108 = ORIENTED_EDGE ( 'NONE', *, *, #27838, .T. ) ;
#13109 = CARTESIAN_POINT ( 'NONE',  ( 0.05014649552807626948, 215.4116977939061144, 46.25113791807857666 ) ) ;
#13110 = FACE_BOUND ( 'NONE', #13350, .T. ) ;
#13111 = CARTESIAN_POINT ( 'NONE',  ( 8.062137200540822946, 212.9164362838583315, 21.69886208192143684 ) ) ;
#13112 = CARTESIAN_POINT ( 'NONE',  ( 62.77499999726882152, 140.1801316387863778, 4.815267126137185549 ) ) ;
#13113 = ORIENTED_EDGE ( 'NONE', *, *, #20401, .T. ) ;
#13114 = DIRECTION ( 'NONE',  ( 0.000000000000000000, 0.000000000000000000, 1.000000000000000000 ) ) ;
#13115 = B_SPLINE_CURVE_WITH_KNOTS ( 'NONE', 3,
 ( #6572, #11519, #11691, #1792, #7085, #9292 ),
 .UNSPECIFIED., .F., .F.,
 ( 4, 2, 4 ),
 ( 0.005649496001316482025, 0.006672230966438342029, 0.007694965931560201165 ),
 .UNSPECIFIED. ) ;
#13116 = DIRECTION ( 'NONE',  ( 1.000000000000000000, 0.000000000000000000, 0.000000000000000000 ) ) ;
#13117 = CARTESIAN_POINT ( 'NONE',  ( -8.015496119326597224, 209.5516654185217362, 8.648862081921436129 ) ) ;
#13118 = CARTESIAN_POINT ( 'NONE',  ( 8.118202686958039038, 212.8392687619912635, 40.70113791807857240 ) ) ;
#13119 = CARTESIAN_POINT ( 'NONE',  ( -10.00000000000000711, 207.0476921513413515, 27.50113791807856600 ) ) ;
#13120 = CARTESIAN_POINT ( 'NONE',  ( -3.044812012439970683, 197.4746971517856196, 103.8988620819214361 ) ) ;
#13121 =( NAMED_UNIT ( * ) PLANE_ANGLE_UNIT ( ) SI_UNIT ( $, .RADIAN. ) );
#13122 = VECTOR ( 'NONE', #12570, 1000.000000000000000 ) ;
#13123 = CARTESIAN_POINT ( 'NONE',  ( 2.517493886309087436, 199.4062855549015865, 91.59886208192145318 ) ) ;
#13124 = CARTESIAN_POINT ( 'NONE',  ( 85.59999999999999432, 150.2886644046228639, 14.49999999999999645 ) ) ;
#13125 = CARTESIAN_POINT ( 'NONE',  ( 81.78867513459482552, 155.0000000000000000, 15.00000000000001243 ) ) ;
#13126 = DIRECTION ( 'NONE',  ( 1.000000000000000000, 0.000000000000000000, 0.000000000000000000 ) ) ;
#13127 = CARTESIAN_POINT ( 'NONE',  ( 7.456977232089302632, 217.1783343296989131, 10.55113791807856671 ) ) ;
#13128 = DIRECTION ( 'NONE',  ( 1.000000000000000000, 0.000000000000000000, 0.000000000000000000 ) ) ;
#13129 = CARTESIAN_POINT ( 'NONE',  ( 55.17499999726881299, 145.8408176439707802, -12.60653300113719588 ) ) ;
#13130 = ADVANCED_FACE ( 'NONE', ( #10377 ), #15477, .F. ) ;
#13131 = CARTESIAN_POINT ( 'NONE',  ( -6.139770520408369237, 215.5359834540460042, 54.95113791807856529 ) ) ;
#13132 = ADVANCED_FACE ( 'NONE', ( #25868 ), #23145, .F. ) ;
#13133 = DIRECTION ( 'NONE',  ( -0.000000000000000000, -0.000000000000000000, 1.000000000000000000 ) ) ;
#13134 = CARTESIAN_POINT ( 'NONE',  ( -7.500000000000000888, -1.443375672974068769, -7.063244554130002406 ) ) ;
#13135 = DIRECTION ( 'NONE',  ( 0.000000000000000000, 0.000000000000000000, 1.000000000000000000 ) ) ;
#13136 = CARTESIAN_POINT ( 'NONE',  ( 57.89999999453762314, 150.2886644046228639, -14.50000000000000888 ) ) ;
#13137 = ORIENTED_EDGE ( 'NONE', *, *, #15619, .T. ) ;
#13138 = CARTESIAN_POINT ( 'NONE',  ( -7.456977232089304408, 196.8216656703010301, 36.05113791807855961 ) ) ;
#13139 = ADVANCED_FACE ( 'NONE', ( #5417 ), #14394, .F. ) ;
#13140 = CARTESIAN_POINT ( 'NONE',  ( 37.68867513459483121, 159.8737954434936057, 15.00000000000001421 ) ) ;
#13141 = CARTESIAN_POINT ( 'NONE',  ( 10.01549611932659545, 203.7984951890123853, 10.14886208192143613 ) ) ;
#13142 = DIRECTION ( 'NONE',  ( 0.000000000000000000, 0.000000000000000000, -1.000000000000000000 ) ) ;
#13143 = ORIENTED_EDGE ( 'NONE', *, *, #21554, .F. ) ;
#13144 =( BOUNDED_CURVE ( )  B_SPLINE_CURVE ( 2, ( #14704, #11984, #33278, #25096, #30218, #12497, #4319, #25270, #1935, #9774, #27817 ),
 .UNSPECIFIED., .F., .T. ) 
 B_SPLINE_CURVE_WITH_KNOTS ( ( 3, 2, 2, 2, 2, 3 ),
 ( 0.5357142857142855874, 0.5392857142857141461, 0.5428571428571427049, 0.5464285714285711526, 0.5499999999999998224, 0.5535714285714283811 ),
 .UNSPECIFIED. ) 
 CURVE ( )  GEOMETRIC_REPRESENTATION_ITEM ( )  RATIONAL_B_SPLINE_CURVE ( ( 1.000000000000001554, 0.9510565162951518658, 1.000000000000000000, 0.9510565162951534202, 1.000000000000000000, 0.9510565162951534202, 1.000000000000000000, 0.9510565162951534202, 1.000000000000000000, 0.9510565162951564178, 0.9999999999999970024 ) ) 
 REPRESENTATION_ITEM ( '' )  );
#13145 = CARTESIAN_POINT ( 'NONE',  ( -3.044812012440131443, 216.5253028482142952, 73.10113791807857808 ) ) ;
#13146 = EDGE_CURVE ( 'NONE', #1081, #12774, #646, .T. ) ;
#13147 = ORIENTED_EDGE ( 'NONE', *, *, #1826, .F. ) ;
#13148 = CARTESIAN_POINT ( 'NONE',  ( 6.500168698208244500, 202.3363017425938324, 37.29886208192144181 ) ) ;
#13149 = CARTESIAN_POINT ( 'NONE',  ( 80.18867513459481700, 140.7341522555726669, 4.635254915624211769 ) ) ;
#13150 = VECTOR ( 'NONE', #29002, 1000.000000000000114 ) ;
#13151 = ORIENTED_EDGE ( 'NONE', *, *, #7623, .F. ) ;
#13152 = CARTESIAN_POINT ( 'NONE',  ( 8.000000000000008882, 206.9523078486586485, 14.00113791807856600 ) ) ;
#13153 = CARTESIAN_POINT ( 'NONE',  ( 12.00000000000000711, 207.0476921513415220, 102.9988620819214304 ) ) ;
#13154 = CARTESIAN_POINT ( 'NONE',  ( 40.87499999726880873, 138.6155565068815747, -3.929120461958505118E-15 ) ) ;
#13155 = EDGE_LOOP ( 'NONE', ( #12007, #17114, #24487, #27790 ) ) ;
#13156 = CARTESIAN_POINT ( 'NONE',  ( 53.02499999726881441, 149.9369285172503510, -15.58253175000000823 ) ) ;
#13157 = CARTESIAN_POINT ( 'NONE',  ( -5.000000000000001776, 0.000000000000000000, -9.974600000000000577 ) ) ;
#13158 = CARTESIAN_POINT ( 'NONE',  ( -10.01549611932653860, 203.7984951890123284, 12.35113791807856387 ) ) ;
#13159 = CIRCLE ( 'NONE', #12081, 40.00000000000000711 ) ;
#13160 = CARTESIAN_POINT ( 'NONE',  ( 10.00000000000000711, 207.0476921513415220, 78.99886208192144466 ) ) ;
#13161 = CARTESIAN_POINT ( 'NONE',  ( 52.17499999726880588, 164.1591823560292198, 12.60653300113718167 ) ) ;
#13162 = CARTESIAN_POINT ( 'NONE',  ( 34.49999999999998579, -2.093232994345345860E-14, -30.00000000000000000 ) ) ;
#13163 = CARTESIAN_POINT ( 'NONE',  ( -9.984503880673473830, 210.2968891136704315, 15.65113791807856813 ) ) ;
#13164 = DIRECTION ( 'NONE',  ( 0.000000000000000000, 0.000000000000000000, -1.000000000000000000 ) ) ;
#13165 = CARTESIAN_POINT ( 'NONE',  ( 65.50000000000000000, 155.0000000000000000, 14.49999999999999467 ) ) ;
#13166 = PLANE ( 'NONE',  #28511 ) ;
#13167 = CARTESIAN_POINT ( 'NONE',  ( 0.000000000000000000, 0.000000000000000000, 30.00000000000000000 ) ) ;
#13168 = CARTESIAN_POINT ( 'NONE',  ( 6.139770520408368348, 198.4640165459539674, 83.45113791807858661 ) ) ;
#13169 = CARTESIAN_POINT ( 'NONE',  ( 117.5000000000000000, 257.3881375866408803, -27.43481878086871717 ) ) ;
#13170 = CARTESIAN_POINT ( 'NONE',  ( 35.07499999726881157, 141.7447067706911810, -9.630534252274385310 ) ) ;
#13171 = CARTESIAN_POINT ( 'NONE',  ( 0.05014649552828288198, 194.3824533091408000, 94.74886208192144466 ) ) ;
#13172 = CARTESIAN_POINT ( 'NONE',  ( 68.82499999726880446, 141.7447067706911810, -9.630534252274385310 ) ) ;
#13173 = ORIENTED_EDGE ( 'NONE', *, *, #18151, .T. ) ;
#13174 = CARTESIAN_POINT ( 'NONE',  ( 4.000000000000000000, 3.518949890710768802, -4.770489558936219510E-15 ) ) ;
#13175 = CIRCLE ( 'NONE', #2774, 2.149999999999984812 ) ;
#13176 = CARTESIAN_POINT ( 'NONE',  ( 87.87499999726877320, 171.3844434931184253, -7.942151717890132712E-15 ) ) ;
#13177 = CARTESIAN_POINT ( 'NONE',  ( 12.01549611932652972, 210.8513442034534933, 94.85113791807856387 ) ) ;
#13178 = LINE ( 'NONE', #243, #18648 ) ;
#13179 = EDGE_LOOP ( 'NONE', ( #28100, #16906, #23456, #33340 ) ) ;
#13180 = CARTESIAN_POINT ( 'NONE',  ( 6.139770520408223575, 215.5359834540460611, 93.54886208192142760 ) ) ;
#13181 = AXIS2_PLACEMENT_3D ( 'NONE', #11525, #13406, #31637 ) ;
#13182 = CARTESIAN_POINT ( 'NONE',  ( 7.456977232089471386, 196.8216656703012006, 25.44886208192143684 ) ) ;
#13183 = DIRECTION ( 'NONE',  ( 0.000000000000000000, 0.000000000000000000, -1.000000000000000000 ) ) ;
#13184 = CARTESIAN_POINT ( 'NONE',  ( 6.220909254589536808, 215.4770327129947702, 46.55113791807856671 ) ) ;
#13185 = ORIENTED_EDGE ( 'NONE', *, *, #31480, .T. ) ;
#13186 = CARTESIAN_POINT ( 'NONE',  ( -7.984503880673422316, 204.3529502787951628, 8.348862081921435419 ) ) ;
#13187 = CARTESIAN_POINT ( 'NONE',  ( 74.61132485994281183, 159.8737954434936057, 15.00000000000001421 ) ) ;
#13188 = ORIENTED_EDGE ( 'NONE', *, *, #2334, .F. ) ;
#13189 = CARTESIAN_POINT ( 'NONE',  ( -2.517493886309087880, 214.5937144450984135, 93.09886208192145318 ) ) ;
#13190 = CARTESIAN_POINT ( 'NONE',  ( -2.517493886308901807, 199.4062855549015012, 29.90113791807857169 ) ) ;
#13191 = CARTESIAN_POINT ( 'NONE',  ( 7.500000000000000000, -2.571118828324946648, -0.3627527587569098766 ) ) ;
#13192 = VERTEX_POINT ( 'NONE', #31318 ) ;
#13193 = CARTESIAN_POINT ( 'NONE',  ( 0.3875187462248268488, 8.436519985393664101, -7.781689322726965230 ) ) ;
#13194 = PRODUCT_DEFINITION_FORMATION_WITH_SPECIFIED_SOURCE ( 'ANY', '', #17886, .NOT_KNOWN. ) ;
#13195 = CARTESIAN_POINT ( 'NONE',  ( 34.47499999726881015, 149.9369285172503510, 15.58253174999999580 ) ) ;
#13196 = CARTESIAN_POINT ( 'NONE',  ( -5.935092644091702674, 206.1175677538518585, -6.000000000000015987 ) ) ;
#13197 = CARTESIAN_POINT ( 'NONE',  ( 8.000000000000008882, 206.9523078486586485, 92.00113791807858377 ) ) ;
#13199 = AXIS2_PLACEMENT_3D ( 'NONE', #15561, #23234, #10309 ) ;
#13198 = DIRECTION ( 'NONE',  ( 0.000000000000000000, 0.000000000000000000, 1.000000000000000000 ) ) ;
#13200 = CARTESIAN_POINT ( 'NONE',  ( 46.59999999999999432, 159.7113355953771077, -14.50000000000000888 ) ) ;
#13201 = CARTESIAN_POINT ( 'NONE',  ( 4.903702542908435547, 213.8346818373419751, 63.54886208192144181 ) ) ;
#13202 = CARTESIAN_POINT ( 'NONE',  ( -60.00000000000000000, -7.347880794884118356E-15, 35.00000000000000000 ) ) ;
#13203 = AXIS2_PLACEMENT_3D ( 'NONE', #9832, #4884, #19872 ) ;
#13204 = CARTESIAN_POINT ( 'NONE',  ( 52.22499999726881725, 149.9369285172503510, 15.58253174999999580 ) ) ;
#13205 = CARTESIAN_POINT ( 'NONE',  ( -0.05014649552810635652, 196.4853777576173002, 5.751137918078565114 ) ) ;
#13206 = FACE_OUTER_BOUND ( 'NONE', #5469, .T. ) ;
#13207 = CARTESIAN_POINT ( 'NONE',  ( 65.72499999726881015, 169.8198683612136222, 4.815267126137181997 ) ) ;
#13208 = CARTESIAN_POINT ( 'NONE',  ( 71.57499999726881867, 164.1591823560292198, -12.60653300113719766 ) ) ;
#13209 = CARTESIAN_POINT ( 'NONE',  ( 7.375838497908181246, 196.7627149292499666, 65.45113791807858661 ) ) ;
#13210 = CARTESIAN_POINT ( 'NONE',  ( 5.000000000000000000, 0.000000000000000000, 0.000000000000000000 ) ) ;
#13211 = CARTESIAN_POINT ( 'NONE',  ( -0.05014649552810635652, 196.4853777576173002, 86.75113791807858377 ) ) ;
#13212 = CARTESIAN_POINT ( 'NONE',  ( 85.08867513459482268, 167.7597621252805880, -9.270509831248443078 ) ) ;
#13213 = CARTESIAN_POINT ( 'NONE',  ( -11.98450388067341876, 203.0532714938636047, 50.34886208192144608 ) ) ;
#13214 = CIRCLE ( 'NONE', #9968, 2.149999999999984812 ) ;
#13215 = CARTESIAN_POINT ( 'NONE',  ( 9.984503880673420539, 210.2968891136705736, 54.84886208192142476 ) ) ;
#13216 = CARTESIAN_POINT ( 'NONE',  ( -12.00000000000000711, 207.0476921513413515, 93.50113791807858377 ) ) ;
#13217 = CARTESIAN_POINT ( 'NONE',  ( 33.98867513459481415, 146.1832212156128890, 12.13525491562421976 ) ) ;
#13218 = CARTESIAN_POINT ( 'NONE',  ( -0.05014649552810635652, 196.4853777576173002, 8.751137918078562450 ) ) ;
#13219 = CARTESIAN_POINT ( 'NONE',  ( -9.984503880673420539, 203.7031108863293980, 77.34886208192142476 ) ) ;
#13220 = EDGE_CURVE ( 'NONE', #7971, #5638, #9860, .T. ) ;
#13221 = VERTEX_POINT ( 'NONE', #17691 ) ;
#13222 = CARTESIAN_POINT ( 'NONE',  ( -3.135527875058821579, 197.5041725223112223, 98.90113791807857524 ) ) ;
#13223 = CIRCLE ( 'NONE', #25753, 4.200000000000001954 ) ;
#13224 = ORIENTED_EDGE ( 'NONE', *, *, #9062, .F. ) ;
#13225 = DIRECTION ( 'NONE',  ( 0.000000000000000000, 0.000000000000000000, -1.000000000000000000 ) ) ;
#13226 = CARTESIAN_POINT ( 'NONE',  ( 8.015496119326595448, 204.4483345814782638, 61.14886208192145034 ) ) ;
#13227 = CONICAL_SURFACE ( 'NONE', #25729, 12.00000000000001066, 0.1047197551196188681 ) ;
#13228 = ORIENTED_EDGE ( 'NONE', *, *, #19348, .T. ) ;
#13229 = VECTOR ( 'NONE', #14772, 1000.000000000000000 ) ;
#13230 = CARTESIAN_POINT ( 'NONE',  ( 78.62499999726881583, 138.6155565068815747, -3.929120461958505118E-15 ) ) ;
#13231 = DIRECTION ( 'NONE',  ( 0.000000000000000000, -0.5000000000000009992, -0.8660254037844380415 ) ) ;
#13232 = CARTESIAN_POINT ( 'NONE',  ( 125.5000000000000000, 231.4735983853260279, 73.43303922622204993 ) ) ;
#13233 = CARTESIAN_POINT ( 'NONE',  ( 71.22499999726879594, 160.0630714827496206, -15.58253175000000823 ) ) ;
#13234 = CARTESIAN_POINT ( 'NONE',  ( -4.984841277089726574, 200.2242689037092305, 60.05113791807858092 ) ) ;
#13235 = CARTESIAN_POINT ( 'NONE',  ( 0.000000000000000000, 0.000000000000000000, -9.449444346342714240 ) ) ;
#13236 = CARTESIAN_POINT ( 'NONE',  ( 6.139770520408223575, 215.5359834540460611, 48.54886208192143471 ) ) ;
#13237 = CARTESIAN_POINT ( 'NONE',  ( -10.00000000000000888, 210.1396626997885448, 100.6464902082600474 ) ) ;
#13238 = AXIS2_PLACEMENT_3D ( 'NONE', #23091, #33481, #31430 ) ;
#13239 = DIRECTION ( 'NONE',  ( 0.000000000000000000, 0.7071067811865411334, -0.7071067811865540120 ) ) ;
#13240 = CARTESIAN_POINT ( 'NONE',  ( -7.984503880673422316, 204.3529502787951628, 38.34886208192142476 ) ) ;
#13241 = CARTESIAN_POINT ( 'NONE',  ( -10.00000000000000711, 207.0476921513413515, 78.50113791807856956 ) ) ;
#13242 = CARTESIAN_POINT ( 'NONE',  ( 62.78867513459482552, 155.0000000000000000, -15.00000000000002487 ) ) ;
#13243 = CARTESIAN_POINT ( 'NONE',  ( -0.05014649552810635652, 196.4853777576173002, 53.75113791807857666 ) ) ;
#13244 = CARTESIAN_POINT ( 'NONE',  ( -10.00000000000000711, 207.0476921513413515, 27.50113791807856600 ) ) ;
#13245 = CARTESIAN_POINT ( 'NONE',  ( 4.903702542908601636, 200.1653181626581102, 11.45113791807856529 ) ) ;
#13246 = CARTESIAN_POINT ( 'NONE',  ( -6.746558653881498557, 3.895127454924315558, -6.526045885145518533 ) ) ;
#13247 = VECTOR ( 'NONE', #31720, 1000.000000000000227 ) ;
#13248 = CARTESIAN_POINT ( 'NONE',  ( 59.78867513459481842, 155.0000000000000000, 15.00000000000001243 ) ) ;
#13249 = CARTESIAN_POINT ( 'NONE',  ( 42.32499999726881157, 145.8408176439707802, 12.60653300113718345 ) ) ;
#13250 = CARTESIAN_POINT ( 'NONE',  ( 12.00000000000000711, 206.9523078486586485, 41.00113791807856245 ) ) ;
#13251 = CARTESIAN_POINT ( 'NONE',  ( 32.50000000000000000, 155.0000000000000000, -15.00000000000002487 ) ) ;
#13252 = AXIS2_PLACEMENT_3D ( 'NONE', #30370, #7375, #32917 ) ;
#13253 = CARTESIAN_POINT ( 'NONE',  ( -3.135527875058821579, 197.5041725223112223, 89.90113791807857524 ) ) ;
#13254 = CARTESIAN_POINT ( 'NONE',  ( 8.062137200540920645, 201.0835637161417822, 59.30113791807857382 ) ) ;
#13255 = CARTESIAN_POINT ( 'NONE',  ( 0.05014649552828288198, 194.3824533091408000, 25.74886208192143755 ) ) ;
#13256 = CARTESIAN_POINT ( 'NONE',  ( 10.00000000000000711, 207.0476921513415220, 30.99886208192143755 ) ) ;
#13257 = CARTESIAN_POINT ( 'NONE',  ( 80.59999999453762598, 168.7903194862797420, 4.480746418436729606 ) ) ;
#13258 = CARTESIAN_POINT ( 'NONE',  ( -7.375838497908182134, 217.2372850707499765, 69.95113791807858661 ) ) ;
#13259 = CARTESIAN_POINT ( 'NONE',  ( 2.517493886308900919, 214.5937144450984420, 91.40113791807857524 ) ) ;
#13260 = CARTESIAN_POINT ( 'NONE',  ( -10.00000000000000711, 206.9523078486584495, 53.49886208192143755 ) ) ;
#13261 = EDGE_CURVE ( 'NONE', #20223, #13276, #5176, .T. ) ;
#13262 = CARTESIAN_POINT ( 'NONE',  ( 10.12668159690567649, 0.000000000000000000, -9.226681596905677907 ) ) ;
#13263 = ORIENTED_EDGE ( 'NONE', *, *, #3784, .F. ) ;
#13264 = CARTESIAN_POINT ( 'NONE',  ( -12.00000000000000711, 206.9523078486584780, 47.49886208192144466 ) ) ;
#13265 = PRESENTATION_LAYER_ASSIGNMENT (  '', '', ( #30690 ) ) ;
#13266 = ORIENTED_EDGE ( 'NONE', *, *, #22463, .F. ) ;
#13267 = EDGE_LOOP ( 'NONE', ( #27757, #26458, #15207, #14181 ) ) ;
#13268 = CARTESIAN_POINT ( 'NONE',  ( 87.28867513459482552, 170.7719333635740497, -7.904646289410545231E-15 ) ) ;
#13269 = EDGE_CURVE ( 'NONE', #250, #31739, #7332, .T. ) ;
#13270 = DIRECTION ( 'NONE',  ( -1.000000000000000000, 0.000000000000000000, 0.000000000000000000 ) ) ;
#13271 = VECTOR ( 'NONE', #29340, 1000.000000000000000 ) ;
#13272 = CARTESIAN_POINT ( 'NONE',  ( -7.984503880673488041, 209.6470497212046098, 45.65113791807857524 ) ) ;
#13273 = AXIS2_PLACEMENT_3D ( 'NONE', #23993, #8489, #1157 ) ;
#13274 = CARTESIAN_POINT ( 'NONE',  ( 10.01549611932659545, 203.7984951890123853, 28.14886208192143613 ) ) ;
#13275 = CARTESIAN_POINT ( 'NONE',  ( 65.37499999726881583, 155.0000000000000000, -15.58253175000000823 ) ) ;
#13276 = VERTEX_POINT ( 'NONE', #7984 ) ;
#13277 = LINE ( 'NONE', #23669, #16159 ) ;
#13278 = ADVANCED_BREP_SHAPE_REPRESENTATION ( '', ( #23813, #2404 ), #29629 ) ;
#13279 = CARTESIAN_POINT ( 'NONE',  ( -4.606548227981510202, -6.456511556909259930, -7.591235721156638583 ) ) ;
#13280 = CARTESIAN_POINT ( 'NONE',  ( 0.05014649552828262524, 198.5883022060938572, 1.748862081921434886 ) ) ;
#13281 = CARTESIAN_POINT ( 'NONE',  ( 9.984503880673470277, 203.7031108863295401, 50.15113791807855392 ) ) ;
#13282 = CARTESIAN_POINT ( 'NONE',  ( 86.81132485994281467, 150.1262045565061385, 14.99999999999982947 ) ) ;
#13283 = EDGE_CURVE ( 'NONE', #31163, #18587, #4914, .T. ) ;
#13284 =( BOUNDED_CURVE ( )  B_SPLINE_CURVE ( 2, ( #25920, #2592, #2765, #20652, #39, #18088, #12631, #20302, #23198, #20475, #31047 ),
 .UNSPECIFIED., .F., .T. ) 
 B_SPLINE_CURVE_WITH_KNOTS ( ( 3, 2, 2, 2, 2, 3 ),
 ( 0.4642857142857142461, 0.4678571428571428048, 0.4714285714285714191, 0.4749999999999999778, 0.4785714285714286476, 0.4821428571428572063 ),
 .UNSPECIFIED. ) 
 CURVE ( )  GEOMETRIC_REPRESENTATION_ITEM ( )  RATIONAL_B_SPLINE_CURVE ( ( 1.000000000000000666, 0.9510565162951526430, 1.000000000000000000, 0.9510565162951534202, 1.000000000000000000, 0.9510565162951534202, 1.000000000000000000, 0.9510565162951534202, 1.000000000000000000, 0.9510565162951526430, 1.000000000000000666 ) ) 
 REPRESENTATION_ITEM ( '' )  );
#13285 = CARTESIAN_POINT ( 'NONE',  ( 8.062137200540920645, 201.0835637161417822, 32.30113791807857382 ) ) ;
#13286 = CYLINDRICAL_SURFACE ( 'NONE', #33141, 15.00000000000001776 ) ;
#13287 = CONTEXT_DEPENDENT_SHAPE_REPRESENTATION ( #25949, #15436 ) ;
#13288 = CARTESIAN_POINT ( 'NONE',  ( -6.444103211790928043, 202.2591342207265939, 95.19886208192144750 ) ) ;
#13289 = CARTESIAN_POINT ( 'NONE',  ( 41.52499999726881441, 169.8198683612136222, -4.815267126137197984 ) ) ;
#13290 = DIRECTION ( 'NONE',  ( 0.000000000000000000, 0.000000000000000000, 1.000000000000000000 ) ) ;
#13291 = CARTESIAN_POINT ( 'NONE',  ( 7.456977232089302632, 217.1783343296989131, 13.55113791807856849 ) ) ;
#13292 = CARTESIAN_POINT ( 'NONE',  ( 48.18867513459482410, 140.7341522555726669, 4.635254915624211769 ) ) ;
#13293 = CARTESIAN_POINT ( 'NONE',  ( 55.37499999726881583, 155.0000000000000000, -15.58253175000000823 ) ) ;
#13294 = ADVANCED_FACE ( 'NONE', ( #25693 ), #5246, .T. ) ;
#13295 = CARTESIAN_POINT ( 'NONE',  ( 8.062137200540920645, 201.0835637161417822, 59.30113791807857382 ) ) ;
#13296 = CARTESIAN_POINT ( 'NONE',  ( -8.062137200540920645, 212.9164362838581894, 27.80113791807856671 ) ) ;
#13297 = CARTESIAN_POINT ( 'NONE',  ( 86.92499999726881299, 145.8408176439707802, -12.60653300113719588 ) ) ;
#13298 = CARTESIAN_POINT ( 'NONE',  ( -6.139770520408224463, 198.4640165459539105, 2.048862081921434264 ) ) ;
#13299 = STYLED_ITEM ( 'NONE', ( #10743 ), #12555 ) ;
#13300 = CARTESIAN_POINT ( 'NONE',  ( 58.59999999453763309, 168.7903194862797420, 4.480746418436729606 ) ) ;
#13301 = VERTEX_POINT ( 'NONE', #20591 ) ;
#13302 = CARTESIAN_POINT ( 'NONE',  ( 3.753561863808689836, 218.3979405102790565, 43.40113791807856813 ) ) ;
#13303 = DIRECTION ( 'NONE',  ( -1.000000000000000000, -0.000000000000000000, 0.000000000000000000 ) ) ;
#13304 = CARTESIAN_POINT ( 'NONE',  ( -6.139770520408224463, 198.4640165459539389, 17.04886208192143826 ) ) ;
#13305 = CARTESIAN_POINT ( 'NONE',  ( 44.81132485994280756, 150.1262045565063943, 14.99999999999999289 ) ) ;
#13306 = VERTEX_POINT ( 'NONE', #30992 ) ;
#13307 = UNCERTAINTY_MEASURE_WITH_UNIT (LENGTH_MEASURE( 1.000000000000000082E-05 ), #32499, 'distance_accuracy_value', 'NONE');
#13308 = CARTESIAN_POINT ( 'NONE',  ( -10.01549611932653860, 203.7984951890123284, 75.35113791807853545 ) ) ;
#13309 = VERTEX_POINT ( 'NONE', #2709 ) ;
#13310 = CYLINDRICAL_SURFACE ( 'NONE', #5334, 4.000000000000000888 ) ;
#13311 = DIRECTION ( 'NONE',  ( 0.000000000000000000, 0.000000000000000000, 1.000000000000000000 ) ) ;
#13312 = ORIENTED_EDGE ( 'NONE', *, *, #12823, .F. ) ;
#13313 = CARTESIAN_POINT ( 'NONE',  ( -0.05014649552807731031, 198.5883022060938572, 17.75113791807856956 ) ) ;
#13314 = EDGE_CURVE ( 'NONE', #26705, #24119, #13409, .T. ) ;
#13315 = EDGE_CURVE ( 'NONE', #29143, #320, #13320, .T. ) ;
#13316 = CARTESIAN_POINT ( 'NONE',  ( 7.456977232089471386, 196.8216656703012006, 100.4488620819214475 ) ) ;
#13317 = CARTESIAN_POINT ( 'NONE',  ( 41.47499999726881015, 160.0630714827496206, -15.58253175000000823 ) ) ;
#13318 = ORIENTED_EDGE ( 'NONE', *, *, #5380, .T. ) ;
#13319 = CARTESIAN_POINT ( 'NONE',  ( 50.62499999726880162, 138.6155565068815463, -3.929120461958505118E-15 ) ) ;
#13320 = B_SPLINE_CURVE_WITH_KNOTS ( 'NONE', 3,
 ( #5736, #32134, #16460, #8152, #29416 ),
 .UNSPECIFIED., .F., .F.,
 ( 4, 1, 4 ),
 ( 0.000000000000000000, 0.003752776749732568765, 0.007505553499465137529 ),
 .UNSPECIFIED. ) ;
#13321 = DIRECTION ( 'NONE',  ( -1.000000000000000000, 0.000000000000000000, 0.000000000000000000 ) ) ;
#13322 = CARTESIAN_POINT ( 'NONE',  ( 8.062137200540920645, 201.0835637161417822, 5.301137918078566713 ) ) ;
#13323 = CARTESIAN_POINT ( 'NONE',  ( -3.044812012439970683, 197.4746971517856196, 76.89886208192143613 ) ) ;
#13324 = CARTESIAN_POINT ( 'NONE',  ( 54.37499999726881583, 155.0000000000000000, 15.58253174999999402 ) ) ;
#13325 = DIRECTION ( 'NONE',  ( -1.000000000000000000, -0.000000000000000000, -0.000000000000000000 ) ) ;
#13326 = CARTESIAN_POINT ( 'NONE',  ( -8.118202686958039038, 201.1607312380087080, 9.201137918078565292 ) ) ;
#13327 = CARTESIAN_POINT ( 'NONE',  ( 44.18867513459481700, 140.7341522555726669, 4.635254915624211769 ) ) ;
#13328 = EDGE_CURVE ( 'NONE', #4979, #9657, #26858, .T. ) ;
#13329 = CARTESIAN_POINT ( 'NONE',  ( 74.70000000000000284, 163.5228861582408797, -11.73074641843674470 ) ) ;
#13330 = CARTESIAN_POINT ( 'NONE',  ( -3.135527875058821579, 197.5041725223112223, 95.90113791807858945 ) ) ;
#13331 = LINE ( 'NONE', #12659, #6054 ) ;
#13332 = CARTESIAN_POINT ( 'NONE',  ( -6.139770520408369237, 215.5359834540460042, 81.95113791807854398 ) ) ;
#13333 = CARTESIAN_POINT ( 'NONE',  ( 40.17499999726881299, 164.1591823560292198, 12.60653300113718167 ) ) ;
#13334 = EDGE_CURVE ( 'NONE', #9027, #31619, #14767, .T. ) ;
#13335 = CARTESIAN_POINT ( 'NONE',  ( 12.00000000000000711, 207.0476921513415220, 93.99886208192144466 ) ) ;
#13336 = CARTESIAN_POINT ( 'NONE',  ( 70.12499999726881583, 155.0000000000000000, 15.58253174999999402 ) ) ;
#13337 = ORIENTED_EDGE ( 'NONE', *, *, #23977, .F. ) ;
#13338 = CARTESIAN_POINT ( 'NONE',  ( -125.0000000000000000, 0.000000000000000000, -20.00000000000000000 ) ) ;
#13339 = CARTESIAN_POINT ( 'NONE',  ( 41.89999999453762314, 150.2886644046228639, -14.50000000000000888 ) ) ;
#13340 = PRODUCT_DEFINITION_SHAPE ( 'NONE', 'NONE',  #33721 ) ;
#13341 = DIRECTION ( 'NONE',  ( -0.000000000000000000, -0.000000000000000000, -1.000000000000000000 ) ) ;
#13342 = VERTEX_POINT ( 'NONE', #16297 ) ;
#13343 = CARTESIAN_POINT ( 'NONE',  ( -8.062137200540822946, 201.0835637161416400, 98.19886208192143329 ) ) ;
#13344 = CARTESIAN_POINT ( 'NONE',  ( 3.753561863808876797, 195.6020594897209719, 34.59886208192143187 ) ) ;
#13345 = LINE ( 'NONE', #20853, #177 ) ;
#13346 = CARTESIAN_POINT ( 'NONE',  ( -10.01549611932653860, 203.7984951890123284, 39.35113791807857098 ) ) ;
#13347 = ORIENTED_EDGE ( 'NONE', *, *, #10960, .T. ) ;
#13348 = CARTESIAN_POINT ( 'NONE',  ( -8.062137200540822946, 201.0835637161416400, 104.1988620819214475 ) ) ;
#13349 = CARTESIAN_POINT ( 'NONE',  ( 73.91132485994280898, 163.8167787843871110, -12.13525491562423397 ) ) ;
#13350 = EDGE_LOOP ( 'NONE', ( #4242, #18387 ) ) ;
#13351 = CARTESIAN_POINT ( 'NONE',  ( 8.000000000000008882, 207.0476921513415220, 90.99886208192144466 ) ) ;
#13352 = EDGE_CURVE ( 'NONE', #33645, #32873, #31188, .T. ) ;
#13353 =( REPRESENTATION_RELATIONSHIP ('NONE','NONE', #25663, #17198 ) REPRESENTATION_RELATIONSHIP_WITH_TRANSFORMATION ( #4910 )SHAPE_REPRESENTATION_RELATIONSHIP( ) );
#13354 = CARTESIAN_POINT ( 'NONE',  ( 4.984841277089725686, 213.7757310962907411, 31.55113791807857382 ) ) ;
#13355 = CARTESIAN_POINT ( 'NONE',  ( -8.331345277524542681, 1.033251829022860324E-15, -8.000000000000000000 ) ) ;
#13356 = ORIENTED_EDGE ( 'NONE', *, *, #4594, .F. ) ;
#13357 = CARTESIAN_POINT ( 'NONE',  ( 33.92499999726881299, 164.1591823560292198, 12.60653300113718167 ) ) ;
#13358 = CARTESIAN_POINT ( 'NONE',  ( 36.57499999726881157, 145.8408176439707802, 12.60653300113718345 ) ) ;
#13359 = DIRECTION ( 'NONE',  ( 1.000000000000000000, 0.000000000000000000, 0.000000000000000000 ) ) ;
#13360 = CARTESIAN_POINT ( 'NONE',  ( -8.000000000000008882, 207.0476921513413515, 84.50113791807856956 ) ) ;
#13361 = CARTESIAN_POINT ( 'NONE',  ( 0.000000000000000000, 0.000000000000000000, 0.000000000000000000 ) ) ;
#13362 = CARTESIAN_POINT ( 'NONE',  ( 48.70000000000000284, 163.5228861582408797, -11.73074641843674470 ) ) ;
#13363 = CARTESIAN_POINT ( 'NONE',  ( 8.015496119326595448, 204.4483345814782638, 67.14886208192143613 ) ) ;
#13364 = CYLINDRICAL_SURFACE ( 'NONE', #14523, 2.149999999999994138 ) ;
#13365 = CARTESIAN_POINT ( 'NONE',  ( 50.42499999726880588, 141.7447067706911810, 9.630534252274376428 ) ) ;
#13367 = ORIENTED_EDGE ( 'NONE', *, *, #5019, .T. ) ;
#13366 = CARTESIAN_POINT ( 'NONE',  ( -10.01549611932653860, 203.7984951890123000, 15.35113791807856565 ) ) ;
#13368 = CARTESIAN_POINT ( 'NONE',  ( 62.52499999726882152, 140.1801316387863778, 4.815267126137185549 ) ) ;
#13369 = CARTESIAN_POINT ( 'NONE',  ( 79.47499999726881015, 160.0630714827496206, -15.58253175000000823 ) ) ;
#13370 = CARTESIAN_POINT ( 'NONE',  ( -9.680171189290831535, 214.0920067884431148, 78.80113791807858092 ) ) ;
#13371 = FACE_OUTER_BOUND ( 'NONE', #22234, .T. ) ;
#13372 = CARTESIAN_POINT ( 'NONE',  ( 3.044812012440130555, 197.4746971517856764, 89.60113791807857808 ) ) ;
#13373 = CARTESIAN_POINT ( 'NONE',  ( 53.98867513459482126, 146.1832212156128890, 12.13525491562421976 ) ) ;
#13374 = ORIENTED_EDGE ( 'NONE', *, *, #14915, .F. ) ;
#13375 = CARTESIAN_POINT ( 'NONE',  ( 12.01549611932659367, 203.1486557965466773, 52.14886208192143613 ) ) ;
#13376 = CARTESIAN_POINT ( 'NONE',  ( 3.044812012439969795, 216.5253028482143520, 69.39886208192143613 ) ) ;
#13377 = CARTESIAN_POINT ( 'NONE',  ( 7.375838497908181246, 196.7627149292499666, 95.45113791807858661 ) ) ;
#13378 = CARTESIAN_POINT ( 'NONE',  ( 34.28867513459483263, 139.2280666364260071, -4.041636747397287284E-15 ) ) ;
#13379 = B_SPLINE_CURVE_WITH_KNOTS ( 'NONE', 3,
 ( #27932, #7156, #14988, #25377, #1535, #1875, #27761, #4764 ),
 .UNSPECIFIED., .F., .F.,
 ( 4, 2, 2, 4 ),
 ( 2.459764730720142121E-07, 0.001920659145285718043, 0.002880865729692040113, 0.003841072314098362400 ),
 .UNSPECIFIED. ) ;
#13380 = CARTESIAN_POINT ( 'NONE',  ( 8.062137200540920645, 201.0835637161417822, 17.30113791807856671 ) ) ;
#13381 = CARTESIAN_POINT ( 'NONE',  ( -3.135527875058982783, 216.4958274776886924, 78.09886208192143897 ) ) ;
#13382 = VERTEX_POINT ( 'NONE', #21744 ) ;
#13383 = CARTESIAN_POINT ( 'NONE',  ( -0.05014649552810635652, 196.4853777576173002, 101.7511379180785411 ) ) ;
#13384 = ORIENTED_EDGE ( 'NONE', *, *, #1670, .T. ) ;
#13385 = FACE_OUTER_BOUND ( 'NONE', #24454, .T. ) ;
#13386 = CARTESIAN_POINT ( 'NONE',  ( 4.984841277089891776, 200.2242689037093726, 61.44886208192144039 ) ) ;
#13387 = EDGE_LOOP ( 'NONE', ( #22557, #32290 ) ) ;
#13388 = CARTESIAN_POINT ( 'NONE',  ( 80.22499999726881015, 149.9369285172503510, 15.58253174999999580 ) ) ;
#13389 = DIRECTION ( 'NONE',  ( 0.000000000000000000, -0.04769215134144196705, 0.9988620819214357738 ) ) ;
#13390 = CARTESIAN_POINT ( 'NONE',  ( 0.000000000000000000, 0.000000000000000000, -20.00000000000000000 ) ) ;
#13391 = UNCERTAINTY_MEASURE_WITH_UNIT (LENGTH_MEASURE( 1.000000000000000082E-05 ), #17898, 'distance_accuracy_value', 'NONE');
#13392 = CARTESIAN_POINT ( 'NONE',  ( 67.92499999726881299, 164.1591823560292198, 12.60653300113718167 ) ) ;
#13393 = CARTESIAN_POINT ( 'NONE',  ( -6.444103211791042618, 211.7408657792732356, 57.80113791807857382 ) ) ;
#13394 = CYLINDRICAL_SURFACE ( 'NONE', #31972, 1.000000000000000000 ) ;
#13395 = CIRCLE ( 'NONE', #901, 24.99999999999999289 ) ;
#13396 = CARTESIAN_POINT ( 'NONE',  ( -9.395856286962974480, 206.1620322824069831, 104.2858818099143008 ) ) ;
#13397 = CLOSED_SHELL ( 'NONE', ( #30057, #5596, #18940, #15010, #30174, #27037, #17455, #18278, #5799, #24450, #19679, #28701, #14405, #18318, #26847, #9259, #20012, #33275, #10576, #10500, #16465, #7695, #9550, #17050, #4789, #22435, #19596 ) ) ;
#13398 =( LENGTH_UNIT ( ) NAMED_UNIT ( * ) SI_UNIT ( .MILLI., .METRE. ) );
#13399 = DIRECTION ( 'NONE',  ( 0.000000000000000000, 0.000000000000000000, -1.000000000000000000 ) ) ;
#13400 = CARTESIAN_POINT ( 'NONE',  ( -8.000000000000008882, 206.9523078486584780, 38.49886208192143044 ) ) ;
#13401 = CARTESIAN_POINT ( 'NONE',  ( 10.01549611932653860, 210.2015048109876716, 79.85113791807853545 ) ) ;
#13402 = DIRECTION ( 'NONE',  ( -1.000000000000000000, -0.000000000000000000, -0.000000000000000000 ) ) ;
#13403 = ADVANCED_FACE ( 'NONE', ( #23803 ), #25028, .F. ) ;
#13404 = CARTESIAN_POINT ( 'NONE',  ( -8.062137200540920645, 212.9164362838581894, 66.80113791807858092 ) ) ;
#13405 = VECTOR ( 'NONE', #57, 1000.000000000000000 ) ;
#13406 = DIRECTION ( 'NONE',  ( 0.000000000000000000, 0.000000000000000000, -1.000000000000000000 ) ) ;
#13407 = CARTESIAN_POINT ( 'NONE',  ( -4.984841277089726574, 200.2242689037092305, 18.05113791807856316 ) ) ;
#13408 = CARTESIAN_POINT ( 'NONE',  ( -6.500000000000000000, 3.752776749732564809, -6.064240316920399110 ) ) ;
#13409 = LINE ( 'NONE', #19028, #16021 ) ;
#13410 = CARTESIAN_POINT ( 'NONE',  ( 47.22499999726881015, 160.0630714827496206, -15.58253175000000823 ) ) ;
#13411 = CARTESIAN_POINT ( 'NONE',  ( -9.736236675707914401, 199.9851607334237542, 42.20113791807857240 ) ) ;
#13412 = DIRECTION ( 'NONE',  ( 1.000000000000000000, 0.000000000000000000, 0.000000000000000000 ) ) ;
#13413 = CARTESIAN_POINT ( 'NONE',  ( -6.139770520408369237, 215.5359834540460042, 93.95113791807854398 ) ) ;
#13414 = CARTESIAN_POINT ( 'NONE',  ( 8.118202686958039038, 212.8392687619912635, 61.70113791807857240 ) ) ;
#13415 = CARTESIAN_POINT ( 'NONE',  ( 0.05014649552828288198, 194.3824533091408000, 22.74886208192143755 ) ) ;
#13416 = CARTESIAN_POINT ( 'NONE',  ( -8.118202686958138514, 212.8392687619910930, 35.79886208192143471 ) ) ;
#13417 = CARTESIAN_POINT ( 'NONE',  ( 79.29999999453762882, 142.6655632788954620, 8.961492836873471646 ) ) ;
#13418 = CARTESIAN_POINT ( 'NONE',  ( -12.01549611932652972, 203.1486557965464499, 69.35113791807857808 ) ) ;
#13419 = CARTESIAN_POINT ( 'NONE',  ( -4.903702542908602524, 213.8346818373418898, 87.95113791807857240 ) ) ;
#13420 = CARTESIAN_POINT ( 'NONE',  ( 10.01549611932659545, 203.7984951890123853, 55.14886208192143613 ) ) ;
#13421 = CARTESIAN_POINT ( 'NONE',  ( 49.18867513459482410, 169.2658477444273331, -4.635254915624224203 ) ) ;
#13422 = ORIENTED_EDGE ( 'NONE', *, *, #7865, .T. ) ;
#13423 = CARTESIAN_POINT ( 'NONE',  ( 3.753561863808876797, 195.6020594897209719, 52.59886208192143897 ) ) ;
#13424 = CONICAL_SURFACE ( 'NONE', #32458, 32.10452846326766974, 1.466076571675243301 ) ;
#13425 = VERTEX_POINT ( 'NONE', #15970 ) ;
#13426 = ORIENTED_EDGE ( 'NONE', *, *, #1239, .F. ) ;
#13427 = AXIS2_PLACEMENT_3D ( 'NONE', #259, #26469, #16077 ) ;
#13428 = CARTESIAN_POINT ( 'NONE',  ( 77.27499999726882152, 149.9369285172503510, -15.58253175000000823 ) ) ;
#13429 = DIRECTION ( 'NONE',  ( 0.000000000000000000, 0.000000000000000000, -1.000000000000000000 ) ) ;
#13430 = CARTESIAN_POINT ( 'NONE',  ( -54.75000000000000000, -7.347880794884118356E-15, 35.00000000000000000 ) ) ;
#13431 = CARTESIAN_POINT ( 'NONE',  ( 6.444103211791042618, 202.2591342207267644, 38.30113791807856671 ) ) ;
#13432 = CARTESIAN_POINT ( 'NONE',  ( -6.220909254589682469, 215.4770327129946850, 26.94886208192142618 ) ) ;
#13433 = CARTESIAN_POINT ( 'NONE',  ( 65.87499999726880162, 171.3844434931184253, -7.942151717890134290E-15 ) ) ;
#13434 = ORIENTED_EDGE ( 'NONE', *, *, #33465, .T. ) ;
#13435 = PLANE ( 'NONE',  #6931 ) ;
#13436 = UNCERTAINTY_MEASURE_WITH_UNIT (LENGTH_MEASURE( 1.000000000000000082E-05 ), #19726, 'distance_accuracy_value', 'NONE');
#13437 =( NAMED_UNIT ( * ) SI_UNIT ( $, .STERADIAN. ) SOLID_ANGLE_UNIT ( ) );
#13438 = PLANE ( 'NONE',  #24980 ) ;
#13439 = CARTESIAN_POINT ( 'NONE',  ( -2.517493886309087880, 214.5937144450984135, 6.098862081921434530 ) ) ;
#13440 = AXIS2_PLACEMENT_3D ( 'NONE', #8385, #21990, #19269 ) ;
#13441 = CARTESIAN_POINT ( 'NONE',  ( 8.118202686958039038, 212.8392687619912635, 55.70113791807857950 ) ) ;
#13442 = DIRECTION ( 'NONE',  ( 0.000000000000000000, 0.000000000000000000, -1.000000000000000000 ) ) ;
#13443 = EDGE_CURVE ( 'NONE', #13301, #4391, #26354, .T. ) ;
#13444 = CARTESIAN_POINT ( 'NONE',  ( 8.118202686958039038, 212.8392687619912635, 25.70113791807856529 ) ) ;
#13445 = CARTESIAN_POINT ( 'NONE',  ( 86.97499999726882436, 140.1801316387863778, -4.815267126137194431 ) ) ;
#13446 = CONTEXT_DEPENDENT_SHAPE_REPRESENTATION ( #32911, #30951 ) ;
#13447 = AXIS2_PLACEMENT_3D ( 'NONE', #3374, #33184, #19383 ) ;
#13448 = CARTESIAN_POINT ( 'NONE',  ( 4.903702542908435547, 213.8346818373419751, 87.54886208192142760 ) ) ;
#13449 = CARTESIAN_POINT ( 'NONE',  ( 38.92499999726881299, 145.8408176439707802, -12.60653300113719588 ) ) ;
#13450 = DIRECTION ( 'NONE',  ( 0.000000000000000000, -0.000000000000000000, -1.000000000000000000 ) ) ;
#13451 = DIRECTION ( 'NONE',  ( 0.000000000000000000, -0.04769215134145524809, -0.9988620819214351076 ) ) ;
#13452 = CARTESIAN_POINT ( 'NONE',  ( -11.98450388067348804, 210.9467285061362247, 6.651137918078566358 ) ) ;
#13453 = CARTESIAN_POINT ( 'NONE',  ( 7.298354728637812983, -4.926141412639873707, -7.913704048099693189 ) ) ;
#13454 = CARTESIAN_POINT ( 'NONE',  ( 54.77499999726881441, 140.1801316387863778, 4.815267126137185549 ) ) ;
#13455 = CARTESIAN_POINT ( 'NONE',  ( -8.062137200540920645, 212.9164362838581894, 54.80113791807857382 ) ) ;
#13456 = CARTESIAN_POINT ( 'NONE',  ( -3.135527875058821579, 197.5041725223112223, 26.90113791807856813 ) ) ;
#13457 = AXIS2_PLACEMENT_3D ( 'NONE', #31759, #10335, #15757 ) ;
#13458 = DIRECTION ( 'NONE',  ( 0.000000000000000000, 0.000000000000000000, 1.000000000000000000 ) ) ;
#13459 = ADVANCED_FACE ( 'NONE', ( #31801 ), #18751, .T. ) ;
#13460 = DIRECTION ( 'NONE',  ( 1.000000000000000000, -0.000000000000000000, -0.000000000000000000 ) ) ;
#13461 = CARTESIAN_POINT ( 'NONE',  ( -9.984503880673420539, 203.7031108863293980, 2.348862081921433642 ) ) ;
#13462 = CARTESIAN_POINT ( 'NONE',  ( 59.39999999453763024, 141.2096805137202580, 4.480746418436733158 ) ) ;
#13463 = VERTEX_POINT ( 'NONE', #803 ) ;
#13464 = CARTESIAN_POINT ( 'NONE',  ( 11.98450388067348271, 203.0532714938637753, 38.15113791807856813 ) ) ;
#13465 = CARTESIAN_POINT ( 'NONE',  ( 3.999999999999999112, 4.898587196589411843E-16, -7.974599999999998801 ) ) ;
#13466 = CARTESIAN_POINT ( 'NONE',  ( 10.01549611932659545, 203.7984951890123853, 25.14886208192143613 ) ) ;
#13467 = CARTESIAN_POINT ( 'NONE',  ( 72.21132485994282035, 170.7719333635740497, -7.904646289410545231E-15 ) ) ;
#13468 = ORIENTED_EDGE ( 'NONE', *, *, #33450, .T. ) ;
#13469 = ADVANCED_FACE ( 'NONE', ( #8635 ), #27025, .F. ) ;
#13470 = CARTESIAN_POINT ( 'NONE',  ( -10.00000000000000711, 207.0476921513413515, 81.50113791807856956 ) ) ;
#13471 = ORIENTED_EDGE ( 'NONE', *, *, #27442, .T. ) ;
#13472 = CIRCLE ( 'NONE', #9142, 27.50000000000000355 ) ;
#13473 = DIRECTION ( 'NONE',  ( 0.000000000000000000, 0.000000000000000000, 1.000000000000000000 ) ) ;
#13474 = DIRECTION ( 'NONE',  ( 0.000000000000000000, 0.000000000000000000, -1.000000000000000000 ) ) ;
#13475 = ORIENTED_EDGE ( 'NONE', *, *, #15983, .T. ) ;
#13476 = CARTESIAN_POINT ( 'NONE',  ( -7.984503880673488041, 209.6470497212046098, 12.65113791807856636 ) ) ;
#13477 = ADVANCED_FACE ( 'NONE', ( #30433 ), #27700, .T. ) ;
#13478 =( BOUNDED_CURVE ( )  B_SPLINE_CURVE ( 3, ( #23736, #33464, #15565, #10313 ),
 .UNSPECIFIED., .F., .T. ) 
 B_SPLINE_CURVE_WITH_KNOTS ( ( 4, 4 ),
 ( 0.000000000000000000, 0.5248789335016748048 ),
 .UNSPECIFIED. ) 
 CURVE ( )  GEOMETRIC_REPRESENTATION_ITEM ( )  RATIONAL_B_SPLINE_CURVE ( ( 1.000000000000000000, 0.9771733092046011038, 0.9771733092046011038, 1.000000000000000000 ) ) 
 REPRESENTATION_ITEM ( '' )  );
#13479 = CARTESIAN_POINT ( 'NONE',  ( -7.456977232089471386, 217.1783343296987709, 95.94886208192144750 ) ) ;
#13480 = CARTESIAN_POINT ( 'NONE',  ( 42.27499999726880731, 160.0630714827496206, 15.58253174999999224 ) ) ;
#13482 = ORIENTED_EDGE ( 'NONE', *, *, #5623, .T. ) ;
#13481 = VECTOR ( 'NONE', #8678, 1000.000000000000000 ) ;
#13483 = CARTESIAN_POINT ( 'NONE',  ( 48.32499999726881157, 145.8408176439707802, 12.60653300113718345 ) ) ;
#13484 = DIRECTION ( 'NONE',  ( 1.000000000000000000, 0.000000000000000000, 0.000000000000000000 ) ) ;
#13485 = CARTESIAN_POINT ( 'NONE',  ( 60.98867513459482836, 163.8167787843871110, -12.13525491562423397 ) ) ;
#13486 = CARTESIAN_POINT ( 'NONE',  ( 10.00000000000000711, 207.0476921513415220, 84.99886208192143044 ) ) ;
#13487 = CARTESIAN_POINT ( 'NONE',  ( 53.87499999726881583, 171.3844434931184253, -7.942151717890132712E-15 ) ) ;
#13488 = CARTESIAN_POINT ( 'NONE',  ( -10.00000000000000711, 207.0476921513413515, 21.50113791807856956 ) ) ;
#13489 = CARTESIAN_POINT ( 'NONE',  ( 127.5000000000000000, 155.0000000000010800, 106.0000000000000142 ) ) ;
#13490 = EDGE_CURVE ( 'NONE', #27429, #15361, #30257, .T. ) ;
#13491 = CARTESIAN_POINT ( 'NONE',  ( 76.80000000000001137, 167.3344367211045096, -8.961492836873482304 ) ) ;
#13492 = CARTESIAN_POINT ( 'NONE',  ( 40.18867513459483121, 140.7341522555726669, 4.635254915624211769 ) ) ;
#13493 = CARTESIAN_POINT ( 'NONE',  ( 105.9028607166213192, 155.0000000000000000, -32.10452846326769816 ) ) ;
#13494 = CARTESIAN_POINT ( 'NONE',  ( -0.05014649552810635652, 196.4853777576173002, 80.75113791807854113 ) ) ;
#13495 = CIRCLE ( 'NONE', #11310, 0.9999999999999947820 ) ;
#13496 = CARTESIAN_POINT ( 'NONE',  ( -27.49999999999999289, 1.342284157770882835, 1.943940613948618489E-15 ) ) ;
#13497 = CARTESIAN_POINT ( 'NONE',  ( 39.77499999726881441, 169.8198683612136222, -4.815267126137197984 ) ) ;
#13498 = CARTESIAN_POINT ( 'NONE',  ( 7.456977232089471386, 196.8216656703012006, 94.44886208192143329 ) ) ;
#13499 = CIRCLE ( 'NONE', #11339, 12.00000000000000355 ) ;
#13500 = CARTESIAN_POINT ( 'NONE',  ( 80.12499999726881583, 155.0000000000000000, 15.58253174999999402 ) ) ;
#13501 = EDGE_CURVE ( 'NONE', #24969, #33593, #11864, .T. ) ;
#13502 = EDGE_LOOP ( 'NONE', ( #10795, #32077 ) ) ;
#13503 = CARTESIAN_POINT ( 'NONE',  ( 48.61132485994281893, 159.8737954434936057, 15.00000000000001421 ) ) ;
#13504 = CARTESIAN_POINT ( 'NONE',  ( 40.29999999453762882, 167.3344367211045096, -8.961492836873482304 ) ) ;
#13505 = FACE_OUTER_BOUND ( 'NONE', #11579, .T. ) ;
#13506 = AXIS2_PLACEMENT_3D ( 'NONE', #9642, #19536, #19361 ) ;
#13507 = CARTESIAN_POINT ( 'NONE',  ( -6.523606932383669843, -4.893847819345372940, -7.213065638944913260 ) ) ;
#13508 = ORIENTED_EDGE ( 'NONE', *, *, #16605, .F. ) ;
#13509 = CARTESIAN_POINT ( 'NONE',  ( 10.01549611932659367, 203.7984951890124421, 94.14886208192143613 ) ) ;
#13510 = CARTESIAN_POINT ( 'NONE',  ( 0.05014649552828288198, 194.3824533091408000, 34.74886208192142334 ) ) ;
#13511 = CARTESIAN_POINT ( 'NONE',  ( -7.914973979435149687, -3.817460047930451239, -7.907502498112421563 ) ) ;
#13512 = CARTESIAN_POINT ( 'NONE',  ( 8.062137200540920645, 201.0835637161417822, 41.30113791807857382 ) ) ;
#13513 = ORIENTED_EDGE ( 'NONE', *, *, #22668, .T. ) ;
#13514 = EDGE_CURVE ( 'NONE', #14561, #20988, #29927, .T. ) ;
#13515 = CARTESIAN_POINT ( 'NONE',  ( 4.903702542908435547, 213.8346818373419751, 3.548862081921434264 ) ) ;
#13516 = CARTESIAN_POINT ( 'NONE',  ( -0.5735064479039806429, 3.710337782248036120, -0.1388410611046141385 ) ) ;
#13517 = EDGE_LOOP ( 'NONE', ( #8248, #14890, #29991, #30272, #12521 ) ) ;
#13518 = CARTESIAN_POINT ( 'NONE',  ( 6.500168698208244500, 202.3363017425938324, 88.29886208192142760 ) ) ;
#13519 = AXIS2_PLACEMENT_3D ( 'NONE', #6698, #32245, #29529 ) ;
#13520 = CIRCLE ( 'NONE', #22771, 3.399999999999999911 ) ;
#13521 = CARTESIAN_POINT ( 'NONE',  ( -0.05014649552807731031, 198.5883022060938572, 32.75113791807856956 ) ) ;
#13522 = CARTESIAN_POINT ( 'NONE',  ( 7.499999999999999112, -2.930060224340428565, -0.4701183149080248036 ) ) ;
#13523 = ORIENTED_EDGE ( 'NONE', *, *, #32658, .T. ) ;
#13524 = DIRECTION ( 'NONE',  ( -1.000000000000000000, -0.000000000000000000, -0.000000000000000000 ) ) ;
#13525 = VECTOR ( 'NONE', #16707, 1000.000000000000000 ) ;
#13526 = CARTESIAN_POINT ( 'NONE',  ( 35.57499999726881157, 164.1591823560292198, -12.60653300113719766 ) ) ;
#13527 = DIRECTION ( 'NONE',  ( -0.5000000000000041078, 0.8660254037844362651, 0.000000000000000000 ) ) ;
#13528 = CARTESIAN_POINT ( 'NONE',  ( 4.903702542908601636, 200.1653181626581102, 101.4511379180785866 ) ) ;
#13529 = AXIS2_PLACEMENT_3D ( 'NONE', #3313, #32563, #19624 ) ;
#13530 = CARTESIAN_POINT ( 'NONE',  ( 245.0000000000000000, 77.50000000000027001, 134.2339375865881834 ) ) ;
#13531 = CARTESIAN_POINT ( 'NONE',  ( 53.60000000000000853, 150.2886644046228639, 14.49999999999999645 ) ) ;
#13532 = CARTESIAN_POINT ( 'NONE',  ( -6.500168698208244500, 211.6636982574061676, 68.79886208192144181 ) ) ;
#13533 = DIRECTION ( 'NONE',  ( 0.000000000000000000, -1.000000000000000000, 0.000000000000000000 ) ) ;
#13534 = CARTESIAN_POINT ( 'NONE',  ( 59.52499999726881441, 169.8198683612136222, -4.815267126137197984 ) ) ;
#13536 = ORIENTED_EDGE ( 'NONE', *, *, #13314, .F. ) ;
#13535 = CARTESIAN_POINT ( 'NONE',  ( 6.220909254589536808, 215.4770327129947987, 7.551137918078564937 ) ) ;
#13537 = CARTESIAN_POINT ( 'NONE',  ( -6.499999999999424460, 2.723853875611551789, -6.224027332484248554 ) ) ;
#13538 = CARTESIAN_POINT ( 'NONE',  ( 62.02499999726880020, 160.0630714827496206, 15.58253174999999224 ) ) ;
#13539 = CARTESIAN_POINT ( 'NONE',  ( 78.27499999726880731, 160.0630714827496206, 15.58253174999999402 ) ) ;
#13540 = CARTESIAN_POINT ( 'NONE',  ( -9.736236675707914401, 199.9851607334237542, 78.20113791807857240 ) ) ;
#13541 = CARTESIAN_POINT ( 'NONE',  ( 49.21132485994281325, 139.2280666364260071, -4.041636747397287284E-15 ) ) ;
#13542 = EDGE_CURVE ( 'NONE', #25011, #12975, #19688, .T. ) ;
#13543 = EDGE_CURVE ( 'NONE', #26498, #11757, #30571, .T. ) ;
#13544 = CARTESIAN_POINT ( 'NONE',  ( -6.220909254589537696, 198.5229672870051445, 93.05113791807856671 ) ) ;
#13545 = ORIENTED_EDGE ( 'NONE', *, *, #7670, .F. ) ;
#13546 = AXIS2_PLACEMENT_3D ( 'NONE', #17552, #2225, #17045 ) ;
#13547 = CARTESIAN_POINT ( 'NONE',  ( 7.456977232089471386, 196.8216656703012006, 58.44886208192144039 ) ) ;
#13548 = CARTESIAN_POINT ( 'NONE',  ( -10.00000000000000711, 207.0476921513413515, 54.50113791807857666 ) ) ;
#13549 = CARTESIAN_POINT ( 'NONE',  ( -3.044812012439970683, 197.4746971517856196, 70.89886208192143613 ) ) ;
#13550 = CARTESIAN_POINT ( 'NONE',  ( -9.680171189290716072, 199.9079932115567146, 8.198862081921433287 ) ) ;
#13551 = DIRECTION ( 'NONE',  ( 1.000000000000000000, 0.000000000000000000, 0.000000000000000000 ) ) ;
#13552 = CARTESIAN_POINT ( 'NONE',  ( -6.139770520408369237, 215.5359834540460042, 9.951137918078567068 ) ) ;
#13553 = EDGE_CURVE ( 'NONE', #20988, #13101, #28408, .T. ) ;
#13554 = EDGE_CURVE ( 'NONE', #26453, #14059, #17139, .T. ) ;
#13555 = CARTESIAN_POINT ( 'NONE',  ( -8.062137200540822946, 201.0835637161416400, 83.19886208192143329 ) ) ;
#13556 = APPLICATION_CONTEXT ( 'automotive_design' ) ;
#13557 = AXIS2_PLACEMENT_3D ( 'NONE', #4138, #32418, #22035 ) ;
#13558 = ORIENTED_EDGE ( 'NONE', *, *, #2237, .T. ) ;
#13559 = CARTESIAN_POINT ( 'NONE',  ( 6.139770520408368348, 198.4640165459539674, 98.45113791807854398 ) ) ;
#13560 = ORIENTED_EDGE ( 'NONE', *, *, #2883, .F. ) ;
#13561 = CYLINDRICAL_SURFACE ( 'NONE', #32481, 99.99999999999997158 ) ;
#13562 = CARTESIAN_POINT ( 'NONE',  ( -6.444103211790928043, 202.2591342207265939, 59.19886208192144750 ) ) ;
#13563 = VERTEX_POINT ( 'NONE', #1134 ) ;
#13564 = CARTESIAN_POINT ( 'NONE',  ( 75.42499999726879878, 168.2552932293087906, -9.630534252274387086 ) ) ;
#13565 = DIRECTION ( 'NONE',  ( 0.000000000000000000, 0.000000000000000000, -1.000000000000000000 ) ) ;
#13566 = CARTESIAN_POINT ( 'NONE',  ( 115.4999999999999858, 155.0000000000000000, -6.938893903907228378E-15 ) ) ;
#13567 = CIRCLE ( 'NONE', #27723, 4.000000000000000000 ) ;
#13568 = CARTESIAN_POINT ( 'NONE',  ( 70.42499999726881299, 141.7447067706911810, 9.630534252274376428 ) ) ;
#13569 = CARTESIAN_POINT ( 'NONE',  ( -6.500168698208129925, 202.3363017425936050, 57.20113791807857240 ) ) ;
#13570 = LINE ( 'NONE', #3509, #18922 ) ;
#13571 = CARTESIAN_POINT ( 'NONE',  ( 0.000000000000000000, 0.000000000000000000, -8.000000000000000000 ) ) ;
#13572 = CARTESIAN_POINT ( 'NONE',  ( 35.29999999999999716, 163.5228861582408797, 11.73074641843673049 ) ) ;
#13573 = CARTESIAN_POINT ( 'NONE',  ( 0.05014649552828262524, 198.5883022060938572, 43.74886208192144466 ) ) ;
#13574 = CARTESIAN_POINT ( 'NONE',  ( -8.118202686958039038, 201.1607312380087080, 81.20113791807857240 ) ) ;
#13575 = DIRECTION ( 'NONE',  ( -1.000000000000000000, -0.000000000000000000, 0.000000000000000000 ) ) ;
#13576 = CARTESIAN_POINT ( 'NONE',  ( 6.220909254589536808, 215.4770327129947702, 61.55113791807858092 ) ) ;
#13577 = DIRECTION ( 'NONE',  ( -0.3500148194780949296, -0.04467534437043436252, 0.9356782244720135422 ) ) ;
#13578 = CARTESIAN_POINT ( 'NONE',  ( 6.500168698208129925, 211.6636982574063381, 19.70113791807856884 ) ) ;
#13579 = FACE_OUTER_BOUND ( 'NONE', #7548, .T. ) ;
#13580 = CARTESIAN_POINT ( 'NONE',  ( -4.444974277457898637, 4.939246403833854160, -5.720331885005371930 ) ) ;
#13581 = CARTESIAN_POINT ( 'NONE',  ( 44.72499999726881015, 140.1801316387863778, -4.815267126137194431 ) ) ;
#13582 = CARTESIAN_POINT ( 'NONE',  ( -3.753561863808691168, 195.6020594897209435, 44.90113791807856813 ) ) ;
#13583 = CARTESIAN_POINT ( 'NONE',  ( 7.915340744421234476, 3.857466640755322640, -7.913699667209310284 ) ) ;
#13584 = CARTESIAN_POINT ( 'NONE',  ( -3.135527875058821579, 197.5041725223112223, 92.90113791807857524 ) ) ;
#13585 = CARTESIAN_POINT ( 'NONE',  ( 0.05014649552810506589, 217.5146222423826714, 64.25113791807856956 ) ) ;
#13586 = CARTESIAN_POINT ( 'NONE',  ( 12.00000000000000711, 207.0476921513415220, 30.99886208192143400 ) ) ;
#13587 = CARTESIAN_POINT ( 'NONE',  ( 8.118202686958138514, 201.1607312380088501, 34.29886208192143471 ) ) ;
#13588 = CARTESIAN_POINT ( 'NONE',  ( 76.59999999453762598, 168.7903194862797420, 4.480746418436729606 ) ) ;
#13589 = CARTESIAN_POINT ( 'NONE',  ( -11.98450388067348804, 210.9467285061362247, 72.65113791807856103 ) ) ;
#13590 = CARTESIAN_POINT ( 'NONE',  ( 6.500168698208129925, 211.6636982574063381, 85.70113791807858661 ) ) ;
#13591 = CARTESIAN_POINT ( 'NONE',  ( 3.044812012439969795, 216.5253028482143520, 48.39886208192143613 ) ) ;
#13592 = CARTESIAN_POINT ( 'NONE',  ( 91.60208470531341618, 155.0000000000000000, -12.00000000000001066 ) ) ;
#13593 = EDGE_LOOP ( 'NONE', ( #29234, #29785, #4600, #7743 ) ) ;
#13594 = CARTESIAN_POINT ( 'NONE',  ( 11.98450388067341876, 210.9467285061363953, 48.84886208192143897 ) ) ;
#13595 = VERTEX_POINT ( 'NONE', #4025 ) ;
#13596 = ORIENTED_EDGE ( 'NONE', *, *, #4778, .T. ) ;
#13597 = CARTESIAN_POINT ( 'NONE',  ( 79.27499999726880731, 149.9369285172503510, -15.58253175000000823 ) ) ;
#13598 = CARTESIAN_POINT ( 'NONE',  ( 52.91132485994280898, 146.1832212156128890, 12.13525491562421976 ) ) ;
#13599 = CARTESIAN_POINT ( 'NONE',  ( 0.000000000000000000, 0.000000000000000000, 0.000000000000000000 ) ) ;
#13600 = CARTESIAN_POINT ( 'NONE',  ( -8.000000000000008882, 207.0476921513413515, 48.50113791807856956 ) ) ;
#13601 = CARTESIAN_POINT ( 'NONE',  ( 8.062137200540822946, 212.9164362838583315, 33.69886208192143329 ) ) ;
#13602 = CARTESIAN_POINT ( 'NONE',  ( 69.87499999726880162, 171.3844434931184253, -7.942151717890134290E-15 ) ) ;
#13603 = VERTEX_POINT ( 'NONE', #9471 ) ;
#13604 = DIRECTION ( 'NONE',  ( -1.000000000000000000, -0.000000000000000000, -0.000000000000000000 ) ) ;
#13605 = CARTESIAN_POINT ( 'NONE',  ( 43.48867513459482836, 167.7597621252805880, 9.270509831248428867 ) ) ;
#13606 = CARTESIAN_POINT ( 'NONE',  ( 6.444103211790928043, 211.7408657792734061, 15.69886208192143684 ) ) ;
#13607 = CARTESIAN_POINT ( 'NONE',  ( -3.044812012440131443, 216.5253028482142952, 55.10113791807857098 ) ) ;
#13608 = CARTESIAN_POINT ( 'NONE',  ( 105.9028607166213192, 155.0000000000000000, 0.000000000000000000 ) ) ;
#13609 = PRODUCT_DEFINITION_SHAPE ( 'NONE', 'NONE',  #33693 ) ;
#13610 = CARTESIAN_POINT ( 'NONE',  ( -0.05014649552810635652, 196.4853777576173002, 38.75113791807856956 ) ) ;
#13611 = CARTESIAN_POINT ( 'NONE',  ( 83.17499999726882720, 145.8408176439707802, -12.60653300113719588 ) ) ;
#13612 = CONTEXT_DEPENDENT_SHAPE_REPRESENTATION ( #27485, #11458 ) ;
#13613 = CARTESIAN_POINT ( 'NONE',  ( -7.984503880673422316, 204.3529502787951628, 92.34886208192143897 ) ) ;
#13614 = CARTESIAN_POINT ( 'NONE',  ( 40.42499999726881299, 141.7447067706911810, 9.630534252274376428 ) ) ;
#13615 = DIRECTION ( 'NONE',  ( -0.5773502691896268413, 0.5773502691896268413, -0.5773502691896235106 ) ) ;
#13616 = CARTESIAN_POINT ( 'NONE',  ( -7.456977232089304408, 196.8216656703010301, 18.05113791807856316 ) ) ;
#13617 = DIRECTION ( 'NONE',  ( 1.000000000000000000, 0.000000000000000000, 0.000000000000000000 ) ) ;
#13618 = CARTESIAN_POINT ( 'NONE',  ( 55.67499999726879878, 168.2552932293087906, -9.630534252274385310 ) ) ;
#13619 = CARTESIAN_POINT ( 'NONE',  ( -6.220909254589537696, 198.5229672870051161, 69.05113791807858092 ) ) ;
#13620 = CARTESIAN_POINT ( 'NONE',  ( -10.00000000000000711, 207.0476921513413515, 27.50113791807856600 ) ) ;
#13621 = CARTESIAN_POINT ( 'NONE',  ( 4.000000000000003553, 4.286263797015736595E-16, -3.500000000000000000 ) ) ;
#13622 = CARTESIAN_POINT ( 'NONE',  ( 78.71132485994280614, 155.0000000000000000, 15.00000000000001243 ) ) ;
#13623 = CARTESIAN_POINT ( 'NONE',  ( -9.984503880673420539, 203.7031108863293980, 8.348862081921435419 ) ) ;
#13624 = TOROIDAL_SURFACE ( 'NONE', #13103, 6.500000000000000888, 1.500000000000000000 ) ;
#13625 = CARTESIAN_POINT ( 'NONE',  ( 60.89999999453761603, 159.7113355953771077, 14.49999999999999289 ) ) ;
#13626 = EDGE_LOOP ( 'NONE', ( #10393, #33552, #51, #3448, #33138, #3840 ) ) ;
#13627 = CARTESIAN_POINT ( 'NONE',  ( 3.753561863808689836, 218.3979405102790565, 52.40113791807858235 ) ) ;
#13628 = CARTESIAN_POINT ( 'NONE',  ( 37.28867513459483263, 170.7719333635740497, -7.904646289410545231E-15 ) ) ;
#13629 = CARTESIAN_POINT ( 'NONE',  ( -6.139770520408224463, 198.4640165459539389, 23.04886208192143116 ) ) ;
#13630 = DIRECTION ( 'NONE',  ( 0.000000000000000000, 0.000000000000000000, -1.000000000000000000 ) ) ;
#13631 = VERTEX_POINT ( 'NONE', #21909 ) ;
#13632 = CIRCLE ( 'NONE', #32667, 5.999999999999995559 ) ;
#13633 = CARTESIAN_POINT ( 'NONE',  ( -3.044812012440131443, 216.5253028482142952, 76.10113791807856387 ) ) ;
#13634 = ORIENTED_EDGE ( 'NONE', *, *, #6673, .T. ) ;
#13635 = EDGE_CURVE ( 'NONE', #21429, #4805, #31657, .T. ) ;
#13636 = FACE_OUTER_BOUND ( 'NONE', #3333, .T. ) ;
#13637 = CARTESIAN_POINT ( 'NONE',  ( -6.781345014477444977, -3.590342129888860256, -6.122077150241852728 ) ) ;
#13638 = ORIENTED_EDGE ( 'NONE', *, *, #1406, .T. ) ;
#13639 = CARTESIAN_POINT ( 'NONE',  ( -7.984503880673488041, 209.6470497212046098, 27.65113791807857169 ) ) ;
#13640 = CARTESIAN_POINT ( 'NONE',  ( 89.50000000000001421, 155.0000000000000000, -6.938893903907228378E-15 ) ) ;
#13641 = CARTESIAN_POINT ( 'NONE',  ( -6.139770520408224463, 198.4640165459539389, 2.048862081921434264 ) ) ;
#13642 = CARTESIAN_POINT ( 'NONE',  ( 42.17499999726881299, 164.1591823560292198, 12.60653300113718167 ) ) ;
#13643 = ORIENTED_EDGE ( 'NONE', *, *, #2660, .F. ) ;
#13644 = CARTESIAN_POINT ( 'NONE',  ( 51.02499999726880731, 149.9369285172503510, -15.58253175000000823 ) ) ;
#13645 = CARTESIAN_POINT ( 'NONE',  ( 127.5000000000000000, 154.9999999999996305, -106.0000000000000142 ) ) ;
#13646 = CARTESIAN_POINT ( 'NONE',  ( 2.000000000000000000, 0.000000000000000000, 0.000000000000000000 ) ) ;
#13647 = VECTOR ( 'NONE', #12749, 1000.000000000000000 ) ;
#13648 = DIRECTION ( 'NONE',  ( 0.000000000000000000, 0.000000000000000000, 1.000000000000000000 ) ) ;
#13649 = CARTESIAN_POINT ( 'NONE',  ( 0.05014649552828275708, 196.4853777576173002, 82.74886208192143044 ) ) ;
#13650 = CARTESIAN_POINT ( 'NONE',  ( 55.47499999726881015, 160.0630714827496206, -15.58253175000000823 ) ) ;
#13651 = CARTESIAN_POINT ( 'NONE',  ( -3.135527875058821579, 197.5041725223112223, 23.90113791807856813 ) ) ;
#13652 = CARTESIAN_POINT ( 'NONE',  ( 7.500000000000000000, -5.637851296924623057E-15, -6.991905250253753756 ) ) ;
#13653 = CARTESIAN_POINT ( 'NONE',  ( -7.375838497908014268, 196.7627149292498530, 83.04886208192144181 ) ) ;
#13654 = CARTESIAN_POINT ( 'NONE',  ( 70.90000000000000568, 168.7903194862797420, -4.480746418436745593 ) ) ;
#13655 = CARTESIAN_POINT ( 'NONE',  ( 62.61132485994281893, 159.8737954434936057, 15.00000000000001421 ) ) ;
#13656 = DIRECTION ( 'NONE',  ( -1.000000000000000000, -0.000000000000000000, -0.000000000000000000 ) ) ;
#13657 = CARTESIAN_POINT ( 'NONE',  ( 8.118202686958039038, 212.8392687619912635, 85.70113791807858661 ) ) ;
#13658 = CARTESIAN_POINT ( 'NONE',  ( 27.50000000000000711, -9.324699302609174012, -17.12819780694305649 ) ) ;
#13659 = CARTESIAN_POINT ( 'NONE',  ( 35.67499999726880588, 168.2552932293087906, -9.630534252274385310 ) ) ;
#13660 = CARTESIAN_POINT ( 'NONE',  ( -10.00000000000000711, 207.0476921513413515, 39.50113791807856956 ) ) ;
#13661 = CARTESIAN_POINT ( 'NONE',  ( 74.42499999726881299, 141.7447067706911810, 9.630534252274376428 ) ) ;
#13662 = EDGE_LOOP ( 'NONE', ( #32285, #285, #4009, #19969 ) ) ;
#13663 = CARTESIAN_POINT ( 'NONE',  ( 40.39999999453763024, 168.7903194862797420, -4.480746418436745593 ) ) ;
#13664 = CARTESIAN_POINT ( 'NONE',  ( -7.375838497908182134, 217.2372850707499765, 6.951137918078566180 ) ) ;
#13665 = CARTESIAN_POINT ( 'NONE',  ( 2.047034997319582939, 2.859595677584332307, -2.900000000000001688 ) ) ;
#13666 = EDGE_LOOP ( 'NONE', ( #30274, #19808, #7839, #5183 ) ) ;
#13667 = CARTESIAN_POINT ( 'NONE',  ( 6.220909254589680693, 198.5229672870052582, 91.44886208192144750 ) ) ;
#13668 = CIRCLE ( 'NONE', #16951, 32.10452846326769816 ) ;
#13669 = CARTESIAN_POINT ( 'NONE',  ( 9.680171189290716072, 214.0920067884432854, 36.69886208192142618 ) ) ;
#13670 = FACE_OUTER_BOUND ( 'NONE', #20524, .T. ) ;
#13671 = CARTESIAN_POINT ( 'NONE',  ( 3.135527875058820690, 216.4958274776887492, 55.40113791807857524 ) ) ;
#13672 = VERTEX_POINT ( 'NONE', #24643 ) ;
#13673 = CARTESIAN_POINT ( 'NONE',  ( 4.903702542908435547, 213.8346818373419751, 9.548862081921432932 ) ) ;
#13674 = ADVANCED_FACE ( 'NONE', ( #14582 ), #8968, .T. ) ;
#13675 = CARTESIAN_POINT ( 'NONE',  ( 50.58867513459482268, 146.1832212156128890, -12.13525491562423042 ) ) ;
#13676 = VERTEX_POINT ( 'NONE', #19358 ) ;
#13677 = CARTESIAN_POINT ( 'NONE',  ( -8.015496119326597224, 209.5516654185217362, 89.64886208192142192 ) ) ;
#13678 = CARTESIAN_POINT ( 'NONE',  ( -7.984503880673488041, 209.6470497212046098, 27.65113791807857169 ) ) ;
#13679 = DIRECTION ( 'NONE',  ( 0.000000000000000000, 0.000000000000000000, -1.000000000000000000 ) ) ;
#13680 = EDGE_LOOP ( 'NONE', ( #32271, #17127, #30068, #7248 ) ) ;
#13681 = CARTESIAN_POINT ( 'NONE',  ( 1.282512619718868541, 8.391164935524033197, -7.795653906408837486 ) ) ;
#13682 = ADVANCED_FACE ( 'NONE', ( #32804 ), #32743, .T. ) ;
#13683 = CARTESIAN_POINT ( 'NONE',  ( 87.52499999726882152, 169.8198683612136222, -4.815267126137197984 ) ) ;
#13684 = CARTESIAN_POINT ( 'NONE',  ( 107.5000000000000000, 155.0000000000000000, -6.938893903907228378E-15 ) ) ;
#13685 = CARTESIAN_POINT ( 'NONE',  ( -6.500168698208129925, 202.3363017425936050, 93.20113791807858661 ) ) ;
#13686 = CARTESIAN_POINT ( 'NONE',  ( 57.60000000000000142, 150.2886644046228639, 14.49999999999999645 ) ) ;
#13687 = CARTESIAN_POINT ( 'NONE',  ( 0.05014649552828262524, 198.5883022060938572, 76.74886208192144466 ) ) ;
#13688 = CARTESIAN_POINT ( 'NONE',  ( -6.270061300899934409, 4.268872906156499170, -6.443866470201760954 ) ) ;
#13689 = EDGE_CURVE ( 'NONE', #24269, #608, #32972, .T. ) ;
#13690 = CARTESIAN_POINT ( 'NONE',  ( 57.62499999726880873, 171.3844434931184253, -7.942151717890132712E-15 ) ) ;
#13691 = CARTESIAN_POINT ( 'NONE',  ( 0.05014649552810506589, 217.5146222423826714, 13.25113791807856600 ) ) ;
#13692 = DIRECTION ( 'NONE',  ( 0.000000000000000000, 1.224646799147353207E-16, 1.000000000000000000 ) ) ;
#13693 = VECTOR ( 'NONE', #24473, 1000.000000000000114 ) ;
#13694 = CARTESIAN_POINT ( 'NONE',  ( 62.82499999726881867, 141.7447067706911810, -9.630534252274387086 ) ) ;
#13695 = CARTESIAN_POINT ( 'NONE',  ( 76.97499999726881015, 140.1801316387863778, -4.815267126137194431 ) ) ;
#13696 = CARTESIAN_POINT ( 'NONE',  ( 9.680171189290831535, 199.9079932115568852, 80.30113791807858092 ) ) ;
#13697 = FACE_OUTER_BOUND ( 'NONE', #9022, .T. ) ;
#13698 = EDGE_CURVE ( 'NONE', #2210, #20526, #16964, .T. ) ;
#13699 = CARTESIAN_POINT ( 'NONE',  ( 3.135527875058820690, 216.4958274776887492, 100.4011379180785752 ) ) ;
#13700 = DIRECTION ( 'NONE',  ( 0.000000000000000000, -0.000000000000000000, 1.000000000000000000 ) ) ;
#13701 = ORIENTED_EDGE ( 'NONE', *, *, #20406, .F. ) ;
#13702 = CARTESIAN_POINT ( 'NONE',  ( -8.118202686958138514, 212.8392687619910930, 5.798862081921434708 ) ) ;
#13703 = CARTESIAN_POINT ( 'NONE',  ( 3.662846001189864698, 218.4274158808046593, 60.39886208192143613 ) ) ;
#13704 = CARTESIAN_POINT ( 'NONE',  ( 9.984503880673420539, 210.2968891136705736, 63.84886208192141765 ) ) ;
#13705 = CARTESIAN_POINT ( 'NONE',  ( 3.662846001189864698, 218.4274158808046593, 3.398862081921433909 ) ) ;
#13706 = SHAPE_REPRESENTATION ( 'Heavy-Duty Caliper Body Housing', ( #2404 ), #33408 ) ;
#13707 = CARTESIAN_POINT ( 'NONE',  ( -60.00000000000000000, -7.347880794884118356E-15, 270.4495957273638282 ) ) ;
#13708 = CARTESIAN_POINT ( 'NONE',  ( 8.062137200540920645, 201.0835637161417822, 26.30113791807856671 ) ) ;
#13709 = CARTESIAN_POINT ( 'NONE',  ( -0.05014649552828403384, 217.5146222423826714, 78.24886208192144466 ) ) ;
#13710 = ORIENTED_EDGE ( 'NONE', *, *, #17229, .F. ) ;
#13711 = PRODUCT_DEFINITION_FORMATION_WITH_SPECIFIED_SOURCE ( 'ANY', '', #28508, .NOT_KNOWN. ) ;
#13712 = CARTESIAN_POINT ( 'NONE',  ( 0.05014649552810505201, 217.5146222423826714, 100.2511379180785838 ) ) ;
#13713 = ORIENTED_EDGE ( 'NONE', *, *, #28526, .F. ) ;
#13714 = CARTESIAN_POINT ( 'NONE',  ( 2.926493552096022466, 2.351840044243029393, -0.1388410611046095033 ) ) ;
#13715 = CARTESIAN_POINT ( 'NONE',  ( 7.984503880673422316, 209.6470497212048372, 60.84886208192144608 ) ) ;
#13716 = ORIENTED_EDGE ( 'NONE', *, *, #14920, .F. ) ;
#13717 = CARTESIAN_POINT ( 'NONE',  ( 76.72499999726881015, 140.1801316387863778, -4.815267126137194431 ) ) ;
#13718 = ORIENTED_EDGE ( 'NONE', *, *, #7494, .F. ) ;
#13719 = CARTESIAN_POINT ( 'NONE',  ( 9.379977934355958169, 208.8253170565643302, -1.014254689207424676 ) ) ;
#13720 = UNCERTAINTY_MEASURE_WITH_UNIT (LENGTH_MEASURE( 1.000000000000000082E-05 ), #17903, 'distance_accuracy_value', 'NONE');
#13721 = CIRCLE ( 'NONE', #13203, 40.00000000000000711 ) ;
#13722 = CARTESIAN_POINT ( 'NONE',  ( 69.82499999726880446, 168.2552932293087906, 9.630534252274372875 ) ) ;
#13723 = CARTESIAN_POINT ( 'NONE',  ( 2.517493886308900919, 214.5937144450984420, 70.40113791807856103 ) ) ;
#13724 = EDGE_CURVE ( 'NONE', #16104, #13382, #19693, .T. ) ;
#13725 = FACE_OUTER_BOUND ( 'NONE', #30925, .T. ) ;
#13726 = EDGE_CURVE ( 'NONE', #3615, #9027, #1469, .T. ) ;
#13727 = CARTESIAN_POINT ( 'NONE',  ( 9.093938419273294826, 26.50387701106810923, -0.2340887491524412944 ) ) ;
#13728 = CARTESIAN_POINT ( 'NONE',  ( 32.70000000000000284, 163.5228861582408797, -11.73074641843674470 ) ) ;
#13729 = B_SPLINE_CURVE_WITH_KNOTS ( 'NONE', 3,
 ( #17248, #4470, #7036, #19972, #1921, #27636 ),
 .UNSPECIFIED., .F., .F.,
 ( 4, 2, 4 ),
 ( 2.475503369438313607E-07, 0.002222330217055647119, 0.004444412883774350592 ),
 .UNSPECIFIED. ) ;
#13730 = CARTESIAN_POINT ( 'NONE',  ( 6.444103211790928043, 211.7408657792734061, 42.69886208192144039 ) ) ;
#13731 = CARTESIAN_POINT ( 'NONE',  ( -8.062137200540920645, 212.9164362838581894, 75.80113791807858092 ) ) ;
#13732 = PRODUCT_DEFINITION ( 'UNKNOWN', '', #5049, #24414 ) ;
#13733 = EDGE_CURVE ( 'NONE', #33037, #12292, #32638, .T. ) ;
#13734 = CARTESIAN_POINT ( 'NONE',  ( -10.00000000000000711, 207.0476921513413515, 63.50113791807856956 ) ) ;
#13735 = VECTOR ( 'NONE', #21465, 1000.000000000000000 ) ;
#13736 = DIRECTION ( 'NONE',  ( -1.000000000000000000, 0.000000000000000000, 0.000000000000000000 ) ) ;
#13737 = CARTESIAN_POINT ( 'NONE',  ( 6.500168698208129925, 211.6636982574063381, 22.70113791807856529 ) ) ;
#13738 = CARTESIAN_POINT ( 'NONE',  ( 4.336808689942017736E-16, 8.660254037844390851, -1.000000000000000888 ) ) ;
#13739 = DIRECTION ( 'NONE',  ( 0.000000000000000000, 0.000000000000000000, -1.000000000000000000 ) ) ;
#13740 = CARTESIAN_POINT ( 'NONE',  ( 43.82499999726881157, 168.2552932293087906, 9.630534252274372875 ) ) ;
#13741 = CARTESIAN_POINT ( 'NONE',  ( -7.456977232089304408, 196.8216656703010301, 51.05113791807856671 ) ) ;
#13742 = CARTESIAN_POINT ( 'NONE',  ( 7.907996613752301229, 3.055722423191984838, -7.792112796859423263 ) ) ;
#13743 = EDGE_CURVE ( 'NONE', #28277, #23864, #19343, .T. ) ;
#13744 = CARTESIAN_POINT ( 'NONE',  ( -10.00000000000000711, 207.0476921513413515, 93.50113791807858377 ) ) ;
#13746 = CARTESIAN_POINT ( 'NONE',  ( -8.118202686958039038, 201.1607312380087080, 66.20113791807857240 ) ) ;
#13745 = APPLICATION_CONTEXT ( 'automotive_design' ) ;
#13747 = CARTESIAN_POINT ( 'NONE',  ( -7.456977232089471386, 217.1783343296987709, 32.94886208192144039 ) ) ;
#13748 = CARTESIAN_POINT ( 'NONE',  ( -3.044812012439970683, 197.4746971517856196, 37.89886208192143613 ) ) ;
#13749 = CARTESIAN_POINT ( 'NONE',  ( 81.09999999453764019, 150.2886644046228639, 14.49999999999999645 ) ) ;
#13750 = CIRCLE ( 'NONE', #173, 4.200000000000001954 ) ;
#13751 = CARTESIAN_POINT ( 'NONE',  ( 7.456977232089302632, 217.1783343296989131, 79.55113791807858092 ) ) ;
#13752 = CARTESIAN_POINT ( 'NONE',  ( -4.903702542908602524, 213.8346818373418898, 93.95113791807857240 ) ) ;
#13753 = VECTOR ( 'NONE', #22570, 1000.000000000000000 ) ;
#13754 = CARTESIAN_POINT ( 'NONE',  ( 3.135527875058981895, 197.5041725223112792, 52.59886208192143897 ) ) ;
#13755 = AXIS2_PLACEMENT_3D ( 'NONE', #2514, #20735, #18187 ) ;
#13756 = CARTESIAN_POINT ( 'NONE',  ( 130.2500000000000000, 3.061616997868383121E-14, -35.00000000000000000 ) ) ;
#13757 = ORIENTED_EDGE ( 'NONE', *, *, #434, .T. ) ;
#13758 = CARTESIAN_POINT ( 'NONE',  ( 11.98450388067341876, 210.9467285061363953, 57.84886208192143187 ) ) ;
#13759 = ORIENTED_EDGE ( 'NONE', *, *, #6759, .T. ) ;
#13760 = CARTESIAN_POINT ( 'NONE',  ( 2.517493886309087436, 199.4062855549015865, 37.59886208192143187 ) ) ;
#13761 = ORIENTED_EDGE ( 'NONE', *, *, #23908, .F. ) ;
#13762 = ADVANCED_FACE ( 'NONE', ( #10159 ), #17814, .T. ) ;
#13763 = CARTESIAN_POINT ( 'NONE',  ( 76.37499999726881583, 155.0000000000000000, 15.58253174999999402 ) ) ;
#13764 = CARTESIAN_POINT ( 'NONE',  ( 0.000000000000000000, 0.000000000000000000, 0.000000000000000000 ) ) ;
#13765 = CIRCLE ( 'NONE', #6703, 2.428571428571428381 ) ;
#13766 = CYLINDRICAL_SURFACE ( 'NONE', #20917, 2.150000000000004352 ) ;
#13767 = CARTESIAN_POINT ( 'NONE',  ( -4.984841277089726574, 200.2242689037092305, 54.05113791807856671 ) ) ;
#13768 = SURFACE_STYLE_USAGE ( .BOTH. , #26218 ) ;
#13769 = CARTESIAN_POINT ( 'NONE',  ( -3.135527875058982783, 216.4958274776886924, 36.09886208192143897 ) ) ;
#13770 = CARTESIAN_POINT ( 'NONE',  ( 67.97499999726881015, 169.8198683612136222, 4.815267126137181997 ) ) ;
#13771 = ORIENTED_EDGE ( 'NONE', *, *, #21349, .F. ) ;
#13772 = CARTESIAN_POINT ( 'NONE',  ( 68.08867513459483689, 142.2402378747194405, 9.270509831248432420 ) ) ;
#13773 = AXIS2_PLACEMENT_3D ( 'NONE', #22714, #25094, #1752 ) ;
#13774 = DIRECTION ( 'NONE',  ( 1.000000000000000000, -0.000000000000000000, -0.000000000000000000 ) ) ;
#13775 = CARTESIAN_POINT ( 'NONE',  ( -4.984841277089891776, 213.7757310962905990, 14.94886208192143506 ) ) ;
#13776 = AXIS2_PLACEMENT_3D ( 'NONE', #18597, #14310, #10932 ) ;
#13777 = CARTESIAN_POINT ( 'NONE',  ( -8.118202686958039038, 201.1607312380087080, 54.20113791807857240 ) ) ;
#13778 = CARTESIAN_POINT ( 'NONE',  ( 2.623433461001182909, -7.604994000793866782, -7.633824513837117465 ) ) ;
#13779 = CARTESIAN_POINT ( 'NONE',  ( -6.139770520408369237, 215.5359834540460042, 33.95113791807855108 ) ) ;
#13780 = CARTESIAN_POINT ( 'NONE',  ( 87.17499999726881299, 145.8408176439707802, -12.60653300113719588 ) ) ;
#13781 = AXIS2_PLACEMENT_3D ( 'NONE', #17418, #22535, #30203 ) ;
#13782 = PRODUCT_CONTEXT ( 'NONE', #6585, 'mechanical' ) ;
#13783 = CARTESIAN_POINT ( 'NONE',  ( -8.000000000000008882, 206.9523078486584780, 98.49886208192143044 ) ) ;
#13784 = CARTESIAN_POINT ( 'NONE',  ( 36.42499999726879878, 141.7447067706911810, 9.630534252274376428 ) ) ;
#13785 = DIRECTION ( 'NONE',  ( -0.000000000000000000, -0.000000000000000000, 1.000000000000000000 ) ) ;
#13786 = DIRECTION ( 'NONE',  ( 0.000000000000000000, 0.000000000000000000, -1.000000000000000000 ) ) ;
#13787 = CARTESIAN_POINT ( 'NONE',  ( 0.05014649552807549926, 219.6175466908591716, 16.25113791807856600 ) ) ;
#13788 = CARTESIAN_POINT ( 'NONE',  ( -2.971071886220377323, -5.790204346174079753, -4.679857033580009373E-15 ) ) ;
#13789 = CARTESIAN_POINT ( 'NONE',  ( 63.67499999726880588, 168.2552932293087906, -9.630534252274385310 ) ) ;
#13790 = CARTESIAN_POINT ( 'NONE',  ( 10.01549611932653860, 210.2015048109876716, 67.85113791807857808 ) ) ;
#13791 = CARTESIAN_POINT ( 'NONE',  ( -6.220909254589537696, 198.5229672870051445, 39.05113791807856671 ) ) ;
#13792 = CARTESIAN_POINT ( 'NONE',  ( -3.339999999999998970, 4.090320309152158050E-16, -0.4621369752184044666 ) ) ;
#13793 = CIRCLE ( 'NONE', #5099, 13.00000000000001066 ) ;
#13794 = CARTESIAN_POINT ( 'NONE',  ( -9.092171885314263236, 26.50489691992488517, -17.71727689882192536 ) ) ;
#13795 = CARTESIAN_POINT ( 'NONE',  ( 9.736236675708031640, 199.9851607334238963, 4.298862081921434708 ) ) ;
#13796 = CARTESIAN_POINT ( 'NONE',  ( 3.044812012439969795, 216.5253028482143520, 9.398862081921436129 ) ) ;
#13797 = CARTESIAN_POINT ( 'NONE',  ( 61.49999999453762456, 139.7537977485451393, -4.138211985947621020E-15 ) ) ;
#13798 = ORIENTED_EDGE ( 'NONE', *, *, #27251, .T. ) ;
#13799 = CARTESIAN_POINT ( 'NONE',  ( 12.01549611932652972, 210.8513442034534933, 46.85113791807857098 ) ) ;
#13800 = CYLINDRICAL_SURFACE ( 'NONE', #24070, 15.00000000000001776 ) ;
#13801 = CARTESIAN_POINT ( 'NONE',  ( -3.135527875058982783, 216.4958274776886924, 18.09886208192143542 ) ) ;
#13802 = LINE ( 'NONE', #16028, #32995 ) ;
#13803 = ORIENTED_EDGE ( 'NONE', *, *, #1901, .F. ) ;
#13804 = CONICAL_SURFACE ( 'NONE', #17601, 8.542937654374687995, 1.221730476396047926 ) ;
#13805 = CARTESIAN_POINT ( 'NONE',  ( -10.01549611932653860, 203.7984951890123284, 84.35113791807856387 ) ) ;
#13806 = AXIS2_PLACEMENT_3D ( 'NONE', #10565, #31336, #8006 ) ;
#13807 = ORIENTED_EDGE ( 'NONE', *, *, #863, .F. ) ;
#13808 = CARTESIAN_POINT ( 'NONE',  ( 50.31132485994280046, 169.2658477444273331, 4.635254915624208216 ) ) ;
#13809 = DIRECTION ( 'NONE',  ( 0.000000000000000000, 0.000000000000000000, 1.000000000000000000 ) ) ;
#13810 = EDGE_LOOP ( 'NONE', ( #26100, #25461 ) ) ;
#13811 = CARTESIAN_POINT ( 'NONE',  ( -6.500168698208129925, 202.3363017425936050, 27.20113791807857240 ) ) ;
#13812 = CARTESIAN_POINT ( 'NONE',  ( -59.14934243545564385, 194.9267577168561161, -2.419719764051426747 ) ) ;
#13813 = CARTESIAN_POINT ( 'NONE',  ( -9.680171189290716072, 199.9079932115567146, 104.1988620819214475 ) ) ;
#13814 = CARTESIAN_POINT ( 'NONE',  ( 51.37499999726881583, 155.0000000000000000, -15.58253175000000823 ) ) ;
#13815 = ORIENTED_EDGE ( 'NONE', *, *, #4323, .T. ) ;
#13816 = CARTESIAN_POINT ( 'NONE',  ( 58.12499999726881583, 155.0000000000000000, 15.58253174999999402 ) ) ;
#13817 = CARTESIAN_POINT ( 'NONE',  ( 8.399999999999998579, 0.000000000000000000, 0.000000000000000000 ) ) ;
#13818 = CARTESIAN_POINT ( 'NONE',  ( 115.4999999999999858, 155.0000000000000000, -6.938893903907228378E-15 ) ) ;
#13819 = STYLED_ITEM ( 'NONE', ( #1205 ), #14909 ) ;
#13820 = DIRECTION ( 'NONE',  ( 0.000000000000000000, -1.224646799147353207E-16, 1.000000000000000000 ) ) ;
#13821 = CARTESIAN_POINT ( 'NONE',  ( 10.00000000000000711, 207.0476921513415220, 87.99886208192144466 ) ) ;
#13822 = CARTESIAN_POINT ( 'NONE',  ( 62.17499999726882010, 164.1591823560292198, 12.60653300113718167 ) ) ;
#13823 = CARTESIAN_POINT ( 'NONE',  ( 3.135527875058820690, 216.4958274776887492, 25.40113791807856813 ) ) ;
#13824 = CARTESIAN_POINT ( 'NONE',  ( 46.78867513459482552, 155.0000000000000000, -15.00000000000002487 ) ) ;
#13825 = CARTESIAN_POINT ( 'NONE',  ( 9.680171189290716072, 214.0920067884432854, 75.69886208192143329 ) ) ;
#13826 = B_SPLINE_CURVE_WITH_KNOTS ( 'NONE', 3,
 ( #8620, #31787, #18349, #6053, #949, #21066 ),
 .UNSPECIFIED., .F., .F.,
 ( 4, 2, 4 ),
 ( 0.003841072314098351557, 0.005765657563962180328, 0.007690242813826009098 ),
 .UNSPECIFIED. ) ;
#13827 = AXIS2_PLACEMENT_3D ( 'NONE', #18576, #11230, #13450 ) ;
#13828 = CARTESIAN_POINT ( 'NONE',  ( 72.00000000000001421, 139.7537977485451393, -4.138211985947621020E-15 ) ) ;
#13829 = CARTESIAN_POINT ( 'NONE',  ( -7.808218555863076560, -4.508077085118260108, -7.999534413642739317 ) ) ;
#13830 = FACE_OUTER_BOUND ( 'NONE', #8288, .T. ) ;
#13831 = CARTESIAN_POINT ( 'NONE',  ( -6.220909254589537696, 198.5229672870051161, 99.05113791807858092 ) ) ;
#13832 = DIRECTION ( 'NONE',  ( -0.000000000000000000, -0.000000000000000000, 1.000000000000000000 ) ) ;
#13833 = CARTESIAN_POINT ( 'NONE',  ( 38.37499999726880873, 155.0000000000000000, 15.58253174999999402 ) ) ;
#13834 = CARTESIAN_POINT ( 'NONE',  ( 10.01549611932653860, 210.2015048109876716, 40.85113791807857098 ) ) ;
#13835 = EDGE_CURVE ( 'NONE', #2881, #22347, #24582, .T. ) ;
#13836 = CARTESIAN_POINT ( 'NONE',  ( 74.22499999726881015, 149.9369285172503510, 15.58253174999999580 ) ) ;
#13837 = ORIENTED_EDGE ( 'NONE', *, *, #19865, .F. ) ;
#13838 = DIRECTION ( 'NONE',  ( 0.000000000000000000, 0.000000000000000000, -1.000000000000000000 ) ) ;
#13839 = CARTESIAN_POINT ( 'NONE',  ( 43.19999999453762740, 146.4771138417591203, 11.73074641843673227 ) ) ;
#13840 = CARTESIAN_POINT ( 'NONE',  ( 9.736236675707914401, 214.0148392665762458, 16.70113791807856529 ) ) ;
#13841 = DIRECTION ( 'NONE',  ( -1.000000000000000000, 0.000000000000000000, 0.000000000000000000 ) ) ;
#13842 = CARTESIAN_POINT ( 'NONE',  ( -2.387978478801491278, -7.281554020289322970, -7.069802615102039667 ) ) ;
#13843 = ORIENTED_EDGE ( 'NONE', *, *, #4058, .T. ) ;
#13844 =( GEOMETRIC_REPRESENTATION_CONTEXT ( 3 ) GLOBAL_UNCERTAINTY_ASSIGNED_CONTEXT ( ( #13307 ) ) GLOBAL_UNIT_ASSIGNED_CONTEXT ( ( #32499, #1001, #8824 ) ) REPRESENTATION_CONTEXT ( 'NONE', 'WORKASPACE' ) );
#13845 = CARTESIAN_POINT ( 'NONE',  ( -8.118202686958138514, 212.8392687619910930, 98.79886208192144181 ) ) ;
#13846 = CARTESIAN_POINT ( 'NONE',  ( 11.98450388067341876, 210.9467285061363953, 36.84886208192142476 ) ) ;
#13847 = CYLINDRICAL_SURFACE ( 'NONE', #16473, 3.499999999999996891 ) ;
#13848 = CARTESIAN_POINT ( 'NONE',  ( 8.118202686958039038, 212.8392687619912635, 49.70113791807857240 ) ) ;
#13849 = VERTEX_POINT ( 'NONE', #7609 ) ;
#13850 = CARTESIAN_POINT ( 'NONE',  ( 6.500168698208244500, 202.3363017425938324, 16.29886208192143471 ) ) ;
#13851 = PRODUCT_DEFINITION_CONTEXT ( 'detailed design', #27683, 'design' ) ;
#13852 = CARTESIAN_POINT ( 'NONE',  ( -125.0000000000000000, -25.00000000000000000, 35.00000000000000000 ) ) ;
#13853 = EDGE_LOOP ( 'NONE', ( #30110, #32539, #8700, #15532 ) ) ;
#13854 = CARTESIAN_POINT ( 'NONE',  ( 2.517493886309087436, 199.4062855549015865, 103.5988620819214532 ) ) ;
#13855 = EDGE_CURVE ( 'NONE', #15528, #4327, #6081, .T. ) ;
#13856 = CARTESIAN_POINT ( 'NONE',  ( 4.903702542908601636, 200.1653181626581102, 41.45113791807857240 ) ) ;
#13857 = CARTESIAN_POINT ( 'NONE',  ( 4.000000000000000000, 1.759474945355380404, -3.047500000000001652 ) ) ;
#13858 = VERTEX_POINT ( 'NONE', #33322 ) ;
#13859 = CARTESIAN_POINT ( 'NONE',  ( 35.12499999726881583, 155.0000000000000000, -15.58253175000000823 ) ) ;
#13860 = CARTESIAN_POINT ( 'NONE',  ( -8.118202686958138514, 212.8392687619910930, 62.79886208192144181 ) ) ;
#13861 = CARTESIAN_POINT ( 'NONE',  ( 36.07499999726880446, 168.2552932293087906, 9.630534252274372875 ) ) ;
#13862 = DIRECTION ( 'NONE',  ( 1.000000000000000000, 0.000000000000000000, 0.000000000000000000 ) ) ;
#13863 = CARTESIAN_POINT ( 'NONE',  ( -2.517493886308901807, 199.4062855549015012, 101.9011379180785895 ) ) ;
#13864 = CARTESIAN_POINT ( 'NONE',  ( 52.00000000000000000, 139.7537977485451393, -4.138211985947621020E-15 ) ) ;
#13865 = CARTESIAN_POINT ( 'NONE',  ( -7.984503880673422316, 204.3529502787951628, 71.34886208192142476 ) ) ;
#13866 = CARTESIAN_POINT ( 'NONE',  ( 0.000000000000000000, 0.000000000000000000, 0.000000000000000000 ) ) ;
#13867 = ADVANCED_FACE ( 'NONE', ( #9819 ), #10989, .T. ) ;
#13868 = CARTESIAN_POINT ( 'NONE',  ( 55.02499999726881441, 149.9369285172503510, -15.58253175000000823 ) ) ;
#13869 = CARTESIAN_POINT ( 'NONE',  ( 10.00000000000000711, 206.9523078486586201, 8.001137918078566003 ) ) ;
#13870 = CARTESIAN_POINT ( 'NONE',  ( 72.99495483890930814, 155.0000000000000000, -6.938893903907228378E-15 ) ) ;
#13871 = CARTESIAN_POINT ( 'NONE',  ( 64.62499999726881583, 138.6155565068815747, -3.929120461958505118E-15 ) ) ;
#13872 = CARTESIAN_POINT ( 'NONE',  ( 77.87499999726881583, 171.3844434931184253, -7.942151717890132712E-15 ) ) ;
#13873 = B_SPLINE_CURVE_WITH_KNOTS ( 'NONE', 3,
 ( #10543, #13246, #23144, #20420, #7648, #13408 ),
 .UNSPECIFIED., .F., .F.,
 ( 4, 2, 4 ),
 ( -4.604908129294308270E-06, 0.0003318387708545208841, 0.0006682824498383361459 ),
 .UNSPECIFIED. ) ;
#13874 = CARTESIAN_POINT ( 'NONE',  ( -11.98450388067348804, 210.9467285061362247, 72.65113791807856103 ) ) ;
#13875 = CARTESIAN_POINT ( 'NONE',  ( 3.044812012440130555, 197.4746971517856764, 95.60113791807857808 ) ) ;
#13876 = DIRECTION ( 'NONE',  ( 0.7071067811865475727, 0.7071067811865475727, 0.000000000000000000 ) ) ;
#13877 = EDGE_CURVE ( 'NONE', #21298, #32783, #17298, .T. ) ;
#13878 = ORIENTED_EDGE ( 'NONE', *, *, #4596, .F. ) ;
#13879 = CARTESIAN_POINT ( 'NONE',  ( 3.753561863808876797, 195.6020594897209719, 103.5988620819214532 ) ) ;
#13880 = CARTESIAN_POINT ( 'NONE',  ( 12.00000000000000711, 207.0476921513415220, 57.99886208192143044 ) ) ;
#13881 = CARTESIAN_POINT ( 'NONE',  ( 6.220909254589680693, 198.5229672870052582, 70.44886208192144750 ) ) ;
#13882 = CARTESIAN_POINT ( 'NONE',  ( -12.01549611932659722, 210.8513442034533227, 2.648862081921433909 ) ) ;
#13883 = CARTESIAN_POINT ( 'NONE',  ( -2.000000000000000888, 2.449293598294707893E-16, -25.03750572909317285 ) ) ;
#13884 = CARTESIAN_POINT ( 'NONE',  ( -10.01549611932653860, 203.7984951890123284, 21.35113791807855677 ) ) ;
#13885 = CARTESIAN_POINT ( 'NONE',  ( -3.135527875058982783, 216.4958274776886924, 84.09886208192143897 ) ) ;
#13886 = ORIENTED_EDGE ( 'NONE', *, *, #24164, .F. ) ;
#13887 = CARTESIAN_POINT ( 'NONE',  ( 71.78867513459482552, 155.0000000000000000, 15.00000000000001243 ) ) ;
#13888 = ORIENTED_EDGE ( 'NONE', *, *, #3875, .F. ) ;
#13889 = FACE_OUTER_BOUND ( 'NONE', #2213, .T. ) ;
#13890 = CARTESIAN_POINT ( 'NONE',  ( 2.426778023690075337, 214.6231898156240447, 72.39886208192143613 ) ) ;
#13891 = EDGE_LOOP ( 'NONE', ( #27720, #12951, #14194 ) ) ;
#13893 = EDGE_CURVE ( 'NONE', #5650, #19014, #28212, .T. ) ;
#13892 = PRODUCT_DEFINITION_SHAPE ( 'NONE', 'NONE',  #33708 ) ;
#13894 = CARTESIAN_POINT ( 'NONE',  ( 78.42499999726881299, 141.7447067706911810, 9.630534252274376428 ) ) ;
#13895 = ORIENTED_EDGE ( 'NONE', *, *, #1899, .T. ) ;
#13896 = DIRECTION ( 'NONE',  ( -1.000000000000000000, 0.000000000000000000, 0.000000000000000000 ) ) ;
#13897 = B_SPLINE_CURVE_WITH_KNOTS ( 'NONE', 3,
 ( #3179, #23794, #24125, #16116, #8624, #21236, #2852, #13396, #24284, #18687, #8458, #294 ),
 .UNSPECIFIED., .F., .F.,
 ( 4, 2, 2, 2, 2, 4 ),
 ( -6.324557791138001430E-06, 0.0004602121660163784782, 0.0009267488898238950392, 0.001160017251727653428, 0.001393285613631411492, 0.001859822337438910272 ),
 .UNSPECIFIED. ) ;
#13898 = ADVANCED_FACE ( 'NONE', ( #25088 ), #7745, .T. ) ;
#13899 = CARTESIAN_POINT ( 'NONE',  ( 67.72499999726881015, 169.8198683612136222, 4.815267126137181997 ) ) ;
#13900 = CARTESIAN_POINT ( 'NONE',  ( 8.000000000000008882, 206.9523078486586485, 71.00113791807856956 ) ) ;
#13901 = LINE ( 'NONE', #16450, #27061 ) ;
#13902 =( NAMED_UNIT ( * ) PLANE_ANGLE_UNIT ( ) SI_UNIT ( $, .RADIAN. ) );
#13903 = CARTESIAN_POINT ( 'NONE',  ( 34.00000000000000711, 139.7537977485451393, -4.138211985947621020E-15 ) ) ;
#13904 = CARTESIAN_POINT ( 'NONE',  ( -0.05014649552828365914, 215.4116977939061144, 42.24886208192143755 ) ) ;
#13905 = CARTESIAN_POINT ( 'NONE',  ( 8.118202686958039038, 212.8392687619912635, 79.70113791807857240 ) ) ;
#13906 = CARTESIAN_POINT ( 'NONE',  ( 6.139770520408368348, 198.4640165459539674, 65.45113791807857240 ) ) ;
#13907 = EDGE_CURVE ( 'NONE', #5638, #5752, #12191, .T. ) ;
#13908 = DIRECTION ( 'NONE',  ( 0.000000000000000000, 0.000000000000000000, -1.000000000000000000 ) ) ;
#13909 = CARTESIAN_POINT ( 'NONE',  ( -2.426778023690262742, 214.6231898156240163, 25.10113791807856742 ) ) ;
#13910 = LINE ( 'NONE', #5735, #30950 ) ;
#13911 = CARTESIAN_POINT ( 'NONE',  ( 60.38867513459481984, 140.7341522555726669, -4.635254915624220651 ) ) ;
#13912 = CARTESIAN_POINT ( 'NONE',  ( 43.22499999726881015, 160.0630714827496206, -15.58253175000000823 ) ) ;
#13913 = CARTESIAN_POINT ( 'NONE',  ( -7.375838497908182134, 217.2372850707499765, 51.95113791807855819 ) ) ;
#13914 = CARTESIAN_POINT ( 'NONE',  ( 7.499999999999999112, 3.105728215500122680, -7.659336188854854122 ) ) ;
#13915 = CARTESIAN_POINT ( 'NONE',  ( -10.01549611932653860, 203.7984951890123284, 93.35113791807857808 ) ) ;
#13916 = CARTESIAN_POINT ( 'NONE',  ( 6.220909254589536808, 215.4770327129947987, 67.55113791807855250 ) ) ;
#13917 = CARTESIAN_POINT ( 'NONE',  ( 7.375838497908012492, 217.2372850707501186, 33.54886208192143471 ) ) ;
#13918 = CARTESIAN_POINT ( 'NONE',  ( -6.220909254589682469, 215.4770327129947134, 38.94886208192143329 ) ) ;
#13919 = CARTESIAN_POINT ( 'NONE',  ( 86.79999999453762882, 163.5228861582408797, 11.73074641843673049 ) ) ;
#13920 = CARTESIAN_POINT ( 'NONE',  ( -3.662846001190052991, 218.4274158808045740, 76.10113791807854966 ) ) ;
#13921 = CARTESIAN_POINT ( 'NONE',  ( 2.426778023690261410, 199.3768101843759837, 95.60113791807857808 ) ) ;
#13922 = EDGE_CURVE ( 'NONE', #5750, #4673, #15343, .T. ) ;
#13923 = CARTESIAN_POINT ( 'NONE',  ( -8.062137200540822946, 201.0835637161416400, 56.19886208192144039 ) ) ;
#13924 = ORIENTED_EDGE ( 'NONE', *, *, #31036, .F. ) ;
#13925 = CARTESIAN_POINT ( 'NONE',  ( -9.680171189290716072, 199.9079932115567146, 59.19886208192144750 ) ) ;
#13926 = VERTEX_POINT ( 'NONE', #14369 ) ;
#13927 = CARTESIAN_POINT ( 'NONE',  ( 2.426778023690075337, 214.6231898156240447, 36.39886208192144323 ) ) ;
#13928 = ORIENTED_EDGE ( 'NONE', *, *, #12602, .T. ) ;
#13929 = EDGE_CURVE ( 'NONE', #18293, #161, #10475, .T. ) ;
#13930 = AXIS2_PLACEMENT_3D ( 'NONE', #1097, #6877, #19657 ) ;
#13931 = CARTESIAN_POINT ( 'NONE',  ( 80.07499999726880446, 168.2552932293087906, 9.630534252274372875 ) ) ;
#13932 = CARTESIAN_POINT ( 'NONE',  ( -58.50000000000001421, -88.00000000000000000, 20.00000000000000000 ) ) ;
#13933 = CARTESIAN_POINT ( 'NONE',  ( 59.18867513459482410, 169.2658477444273331, -4.635254915624224203 ) ) ;
#13934 = CARTESIAN_POINT ( 'NONE',  ( 8.000000000000008882, 206.9523078486586485, 50.00113791807856956 ) ) ;
#13935 = EDGE_CURVE ( 'NONE', #6207, #26026, #13159, .T. ) ;
#13936 = DIRECTION ( 'NONE',  ( 1.000000000000000000, 0.000000000000000000, 0.000000000000000000 ) ) ;
#13937 = CARTESIAN_POINT ( 'NONE',  ( -3.044812012439970683, 197.4746971517856196, 28.89886208192143613 ) ) ;
#13938 = CARTESIAN_POINT ( 'NONE',  ( 69.07499999726881867, 141.7447067706911810, -9.630534252274387086 ) ) ;
#13939 = ORIENTED_EDGE ( 'NONE', *, *, #11189, .F. ) ;
#13940 = AXIS2_PLACEMENT_3D ( 'NONE', #10781, #19056, #1163 ) ;
#13941 = CARTESIAN_POINT ( 'NONE',  ( 36.71132485994280614, 155.0000000000000000, 15.00000000000001243 ) ) ;
#13942 = CARTESIAN_POINT ( 'NONE',  ( 51.88867513459483405, 150.1262045565062806, 14.99999999999992006 ) ) ;
#13943 = CARTESIAN_POINT ( 'NONE',  ( 125.5000000000000000, 152.8499999999996533, -106.0000000000000000 ) ) ;
#13944 = CARTESIAN_POINT ( 'NONE',  ( -2.517493886309087880, 214.5937144450984135, 18.09886208192143187 ) ) ;
#13945 = CARTESIAN_POINT ( 'NONE',  ( -10.00000000000000711, 207.0476921513413515, 48.50113791807856956 ) ) ;
#13946 = CARTESIAN_POINT ( 'NONE',  ( -8.062137200540920645, 212.9164362838581894, 33.80113791807857382 ) ) ;
#13947 = CARTESIAN_POINT ( 'NONE',  ( 83.27499999726880731, 149.9369285172503510, -15.58253175000000823 ) ) ;
#13948 = SHAPE_DEFINITION_REPRESENTATION ( #4537, #21975 ) ;
#13949 = CARTESIAN_POINT ( 'NONE',  ( -2.426778023690076225, 199.3768101843759553, 97.89886208192146455 ) ) ;
#13950 = CARTESIAN_POINT ( 'NONE',  ( 39.82499999726880446, 168.2552932293087906, 9.630534252274372875 ) ) ;
#13951 = SURFACE_STYLE_USAGE ( .BOTH. , #19237 ) ;
#13952 = CARTESIAN_POINT ( 'NONE',  ( -145.0000000000000000, 0.000000000000000000, 35.00200000000000244 ) ) ;
#13953 = CARTESIAN_POINT ( 'NONE',  ( -7.375838497908182134, 217.2372850707499765, 15.95113791807856707 ) ) ;
#13954 = DIRECTION ( 'NONE',  ( -0.000000000000000000, -0.000000000000000000, 1.000000000000000000 ) ) ;
#13955 = CARTESIAN_POINT ( 'NONE',  ( 63.57499999726881867, 164.1591823560292198, -12.60653300113719766 ) ) ;
#13956 = CARTESIAN_POINT ( 'NONE',  ( 8.062137200540920645, 201.0835637161417822, 68.30113791807856671 ) ) ;
#13957 = CARTESIAN_POINT ( 'NONE',  ( 6.139770520408367460, 198.4640165459539389, 41.45113791807857240 ) ) ;
#13958 = CARTESIAN_POINT ( 'NONE',  ( -52.50000000000002132, 155.0000000000000000, 17.00000000000001066 ) ) ;
#13959 = CARTESIAN_POINT ( 'NONE',  ( 9.680171189290716072, 214.0920067884432854, 3.698862081921433731 ) ) ;
#13960 = CARTESIAN_POINT ( 'NONE',  ( -10.01549611932659545, 210.2015048109875011, 11.64886208192143435 ) ) ;
#13961 = CARTESIAN_POINT ( 'NONE',  ( 65.29999999453762882, 142.6655632788954620, 8.961492836873471646 ) ) ;
#13962 = ORIENTED_EDGE ( 'NONE', *, *, #31210, .T. ) ;
#13963 = CARTESIAN_POINT ( 'NONE',  ( -9.680171189290831535, 214.0920067884431148, 48.80113791807857382 ) ) ;
#13964 = CARTESIAN_POINT ( 'NONE',  ( -8.000000000000008882, 207.0476921513413515, 66.50113791807856956 ) ) ;
#13965 = CARTESIAN_POINT ( 'NONE',  ( 2.000000000000000000, 1.773042676681340968, -2.276824562219559311E-15 ) ) ;
#13966 = CARTESIAN_POINT ( 'NONE',  ( 8.062137200540822946, 212.9164362838583315, 18.69886208192143329 ) ) ;
#13967 = EDGE_CURVE ( 'NONE', #30536, #24528, #26760, .T. ) ;
#13968 = DIRECTION ( 'NONE',  ( -0.000000000000000000, -0.000000000000000000, 1.000000000000000000 ) ) ;
#13969 = AXIS2_PLACEMENT_3D ( 'NONE', #6954, #33005, #19727 ) ;
#13970 = ORIENTED_EDGE ( 'NONE', *, *, #7388, .T. ) ;
#13971 = CARTESIAN_POINT ( 'NONE',  ( 3.135527875058820690, 216.4958274776887492, 85.40113791807857524 ) ) ;
#13972 = ORIENTED_EDGE ( 'NONE', *, *, #9785, .T. ) ;
#13973 = EDGE_CURVE ( 'NONE', #20097, #1044, #14696, .T. ) ;
#13974 = CARTESIAN_POINT ( 'NONE',  ( 49.91132485994280188, 163.8167787843871110, -12.13525491562423397 ) ) ;
#13975 = CARTESIAN_POINT ( 'NONE',  ( 0.000000000000000000, 0.000000000000000000, -2.629527361626598836 ) ) ;
#13976 = ORIENTED_EDGE ( 'NONE', *, *, #18516, .F. ) ;
#13977 = CARTESIAN_POINT ( 'NONE',  ( -2.426778023690262742, 214.6231898156240163, 22.10113791807856742 ) ) ;
#13978 = CARTESIAN_POINT ( 'NONE',  ( -59.30520453566667527, 194.9296309105606326, -2.372451168785852715 ) ) ;
#13979 = AXIS2_PLACEMENT_3D ( 'NONE', #31654, #15653, #5749 ) ;
#13980 = CARTESIAN_POINT ( 'NONE',  ( -6.220909254589682469, 215.4770327129946850, 2.948862081921434175 ) ) ;
#13981 = CARTESIAN_POINT ( 'NONE',  ( 47.07499999726881157, 141.7447067706911810, -9.630534252274387086 ) ) ;
#13982 = ORIENTED_EDGE ( 'NONE', *, *, #29106, .T. ) ;
#13983 = CARTESIAN_POINT ( 'NONE',  ( 56.52499999726881441, 140.1801316387863778, 4.815267126137185549 ) ) ;
#13984 = CARTESIAN_POINT ( 'NONE',  ( 7.703928834700302986, -4.447865386531950627, -7.917997657324739258 ) ) ;
#13985 = CARTESIAN_POINT ( 'NONE',  ( 54.75000000000000000, 7.990820364436479461E-15, 35.00000000000000000 ) ) ;
#13986 = VECTOR ( 'NONE', #14653, 1000.000000000000000 ) ;
#13987 = CARTESIAN_POINT ( 'NONE',  ( 92.60756280994512224, 155.0000000000000000, 0.000000000000000000 ) ) ;
#13988 = CARTESIAN_POINT ( 'NONE',  ( -8.062137200540822946, 201.0835637161416400, 89.19886208192144750 ) ) ;
#13989 = CARTESIAN_POINT ( 'NONE',  ( 58.27499999726880731, 160.0630714827496206, 15.58253174999999402 ) ) ;
#13990 = CARTESIAN_POINT ( 'NONE',  ( -10.01549611932653860, 203.7984951890123284, 27.35113791807856742 ) ) ;
#13991 = CARTESIAN_POINT ( 'NONE',  ( 47.48867513459482836, 167.7597621252805880, 9.270509831248428867 ) ) ;
#13992 = CARTESIAN_POINT ( 'NONE',  ( 7.456977232089471386, 196.8216656703012006, 79.44886208192144750 ) ) ;
#13993 = AXIS2_PLACEMENT_3D ( 'NONE', #9806, #10146, #22917 ) ;
#13994 = CARTESIAN_POINT ( 'NONE',  ( 73.89999999999999147, 141.2096805137202580, 4.480746418436733158 ) ) ;
#13995 = DIRECTION ( 'NONE',  ( -0.1045284632676463932, 1.217938055844715641E-16, -0.9945218953682741780 ) ) ;
#13996 = CARTESIAN_POINT ( 'NONE',  ( 9.443650191645208025, 207.8375535574373032, -0.8718850525427659370 ) ) ;
#13997 = CARTESIAN_POINT ( 'NONE',  ( -10.00000000000000711, 207.0476921513413515, 96.50113791807856956 ) ) ;
#13998 = CARTESIAN_POINT ( 'NONE',  ( 32.78867513459481842, 155.0000000000000000, -15.00000000000002487 ) ) ;
#13999 = CARTESIAN_POINT ( 'NONE',  ( 46.97499999726881015, 140.1801316387863778, -4.815267126137194431 ) ) ;
#14000 = CARTESIAN_POINT ( 'NONE',  ( 8.062137200540920645, 201.0835637161417822, 38.30113791807857382 ) ) ;
#14001 = CARTESIAN_POINT ( 'NONE',  ( 76.62499999726880162, 138.6155565068815463, -3.929120461958505118E-15 ) ) ;
#14002 = ORIENTED_EDGE ( 'NONE', *, *, #8289, .F. ) ;
#14003 = DIRECTION ( 'NONE',  ( 1.000000000000000000, 0.000000000000000000, 0.000000000000000000 ) ) ;
#14004 = CARTESIAN_POINT ( 'NONE',  ( 45.19999999453762740, 146.4771138417591203, 11.73074641843673227 ) ) ;
#14005 = CARTESIAN_POINT ( 'NONE',  ( -12.00000000000000711, 207.0476921513413515, 21.50113791807856956 ) ) ;
#14006 = AXIS2_PLACEMENT_3D ( 'NONE', #33521, #31308, #7972 ) ;
#14007 = DIRECTION ( 'NONE',  ( 0.9945218953682747332, 0.000000000000000000, -0.1045284632676402453 ) ) ;
#14008 = VECTOR ( 'NONE', #17828, 1000.000000000000000 ) ;
#14009 = CARTESIAN_POINT ( 'NONE',  ( -7.847095227763516867, -4.129731495738496960, -7.493596212620239783 ) ) ;
#14010 = ORIENTED_EDGE ( 'NONE', *, *, #29028, .F. ) ;
#14011 = CARTESIAN_POINT ( 'NONE',  ( -3.662846001189865142, 195.5725841191952838, 31.89886208192143613 ) ) ;
#14012 = DIRECTION ( 'NONE',  ( 0.000000000000000000, 0.000000000000000000, -1.000000000000000000 ) ) ;
#14013 = CARTESIAN_POINT ( 'NONE',  ( 8.062137200540920645, 201.0835637161417822, 53.30113791807857382 ) ) ;
#14014 = ORIENTED_EDGE ( 'NONE', *, *, #7853, .T. ) ;
#14015 = CARTESIAN_POINT ( 'NONE',  ( 6.500168698208244500, 202.3363017425938324, 13.29886208192143826 ) ) ;
#14016 = VECTOR ( 'NONE', #18454, 1000.000000000000000 ) ;
#14017 = CARTESIAN_POINT ( 'NONE',  ( 51.11132485994281183, 140.7341522555726669, 4.635254915624211769 ) ) ;
#14018 = EDGE_LOOP ( 'NONE', ( #31817, #12138, #20340, #23874, #18303, #29145, #1024 ) ) ;
#14019 = CARTESIAN_POINT ( 'NONE',  ( -2.517493886309087880, 214.5937144450984135, 96.09886208192143897 ) ) ;
#14020 = CARTESIAN_POINT ( 'NONE',  ( -4.984841277089726574, 200.2242689037092305, 36.05113791807856671 ) ) ;
#14021 = FACE_OUTER_BOUND ( 'NONE', #6396, .T. ) ;
#14022 = EDGE_LOOP ( 'NONE', ( #25123, #1770, #12048, #29677 ) ) ;
#14023 = CARTESIAN_POINT ( 'NONE',  ( 40.42499999726881299, 141.7447067706911810, 9.630534252274376428 ) ) ;
#14024 = AXIS2_PLACEMENT_3D ( 'NONE', #28198, #7247, #30931 ) ;
#14025 = CARTESIAN_POINT ( 'NONE',  ( 6.139770520408223575, 215.5359834540460611, 60.54886208192143471 ) ) ;
#14026 = CARTESIAN_POINT ( 'NONE',  ( 42.07499999726881157, 168.2552932293087906, 9.630534252274372875 ) ) ;
#14027 = DIRECTION ( 'NONE',  ( 1.000000000000000000, -0.000000000000000000, -0.000000000000000000 ) ) ;
#14028 = CARTESIAN_POINT ( 'NONE',  ( -8.015496119326531499, 204.4483345814780364, 102.3511379180785639 ) ) ;
#14029 = PRODUCT ( 'torque nut 01_iso_ISO 7040-M4-N', 'torque nut 01_iso_ISO 7040-M4-N', '', ( #15677 ) ) ;
#14030 = AXIS2_PLACEMENT_3D ( 'NONE', #23866, #13473, #31701 ) ;
#14031 = AXIS2_PLACEMENT_3D ( 'NONE', #15581, #31272, #33483 ) ;
#14032 = CARTESIAN_POINT ( 'NONE',  ( 56.90000000000000568, 168.7903194862797420, -4.480746418436745593 ) ) ;
#14033 = CARTESIAN_POINT ( 'NONE',  ( 8.015496119326595448, 204.4483345814782638, 76.14886208192143613 ) ) ;
#14034 = DIRECTION ( 'NONE',  ( -1.000000000000000000, 0.000000000000000000, 0.000000000000000000 ) ) ;
#14035 = FACE_OUTER_BOUND ( 'NONE', #30793, .T. ) ;
#14036 = AXIS2_PLACEMENT_3D ( 'NONE', #24345, #11080, #3064 ) ;
#14037 = CARTESIAN_POINT ( 'NONE',  ( 56.52499999726881441, 140.1801316387863778, 4.815267126137185549 ) ) ;
#14039 = EDGE_LOOP ( 'NONE', ( #29520, #14857, #15107, #20778 ) ) ;
#14038 = CARTESIAN_POINT ( 'NONE',  ( -9.984503880673475606, 210.2968891136704315, 9.651137918078566358 ) ) ;
#14040 = CYLINDRICAL_SURFACE ( 'NONE', #29868, 15.00000000000001776 ) ;
#14041 = CARTESIAN_POINT ( 'NONE',  ( 67.02499999726880731, 149.9369285172503510, -15.58253175000000823 ) ) ;
#14042 = CARTESIAN_POINT ( 'NONE',  ( 78.87499999726878741, 138.6155565068815463, -3.929120461958505118E-15 ) ) ;
#14043 = CARTESIAN_POINT ( 'NONE',  ( 3.753561863808689836, 218.3979405102790565, 79.40113791807858945 ) ) ;
#14044 = CARTESIAN_POINT ( 'NONE',  ( -10.00000000000000711, 207.0476921513413515, 93.50113791807858377 ) ) ;
#14045 = CARTESIAN_POINT ( 'NONE',  ( -10.00000000000000178, 208.0352956435529563, 102.7846294209004441 ) ) ;
#14046 = VERTEX_POINT ( 'NONE', #27641 ) ;
#14047 = CARTESIAN_POINT ( 'NONE',  ( 9.984503880673420539, 210.2968891136705167, 3.848862081921433642 ) ) ;
#14048 = CARTESIAN_POINT ( 'NONE',  ( -7.375838497908014268, 196.7627149292498530, 62.04886208192144181 ) ) ;
#14049 = CARTESIAN_POINT ( 'NONE',  ( 6.220909254589680693, 198.5229672870052582, 67.44886208192143329 ) ) ;
#14050 = CARTESIAN_POINT ( 'NONE',  ( 3.753561863808876797, 195.6020594897209719, 4.598862081921434530 ) ) ;
#14051 = CARTESIAN_POINT ( 'NONE',  ( -5.441945782601304238, -4.363644636964928658, -0.3576316571898465746 ) ) ;
#14052 = CARTESIAN_POINT ( 'NONE',  ( -9.984503880673473830, 210.2968891136704315, 27.65113791807855748 ) ) ;
#14053 = CARTESIAN_POINT ( 'NONE',  ( 0.05014649552828275708, 196.4853777576173002, 88.74886208192140202 ) ) ;
#14054 = EDGE_LOOP ( 'NONE', ( #9169, #15775, #12857, #23577 ) ) ;
#14055 = CARTESIAN_POINT ( 'NONE',  ( -1.604619215278546562E-14, -7.505553499465138501, -0.8000000000000003775 ) ) ;
#14056 = EDGE_LOOP ( 'NONE', ( #28491, #2295, #25672, #4257, #31042, #18339 ) ) ;
#14057 = CARTESIAN_POINT ( 'NONE',  ( 5.000000000000000000, 0.000000000000000000, 0.000000000000000000 ) ) ;
#14058 = CARTESIAN_POINT ( 'NONE',  ( 0.05014649552828262524, 198.5883022060938572, 73.74886208192144466 ) ) ;
#14059 = VERTEX_POINT ( 'NONE', #4310 ) ;
#14060 = ADVANCED_FACE ( 'NONE', ( #27984 ), #29489, .F. ) ;
#14061 = VECTOR ( 'NONE', #15264, 1000.000000000000000 ) ;
#14062 = CARTESIAN_POINT ( 'NONE',  ( 86.12499999726881583, 155.0000000000000000, 15.58253174999999402 ) ) ;
#14063 = EDGE_LOOP ( 'NONE', ( #20063, #21006 ) ) ;
#14064 = FACE_OUTER_BOUND ( 'NONE', #2977, .T. ) ;
#14065 = CARTESIAN_POINT ( 'NONE',  ( 78.62499999726881583, 138.6155565068815463, -3.929120461958505118E-15 ) ) ;
#14066 = CARTESIAN_POINT ( 'NONE',  ( -4.984841277089726574, 200.2242689037092305, 66.05113791807858092 ) ) ;
#14067 = CARTESIAN_POINT ( 'NONE',  ( -67.50000000000000000, 122.1366465496900275, 17.00000000000001421 ) ) ;
#14068 = CARTESIAN_POINT ( 'NONE',  ( 35.10000000000000142, 168.7903194862797420, 4.480746418436729606 ) ) ;
#14069 = CARTESIAN_POINT ( 'NONE',  ( 8.015496119326595448, 204.4483345814782638, 43.14886208192144323 ) ) ;
#14070 = VECTOR ( 'NONE', #25952, 1000.000000000000000 ) ;
#14071 = CARTESIAN_POINT ( 'NONE',  ( -10.01549611932653860, 203.7984951890123284, 90.35113791807857808 ) ) ;
#14072 = CARTESIAN_POINT ( 'NONE',  ( -6.139770520408369237, 215.5359834540460042, 66.95113791807858661 ) ) ;
#14073 = AXIS2_PLACEMENT_3D ( 'NONE', #17984, #7423, #2483 ) ;
#14074 = CARTESIAN_POINT ( 'NONE',  ( 8.062137200540920645, 201.0835637161417822, 89.30113791807858092 ) ) ;
#14075 = DIRECTION ( 'NONE',  ( 1.000000000000000000, -0.000000000000000000, -0.000000000000000000 ) ) ;
#14076 = CARTESIAN_POINT ( 'NONE',  ( 4.903702542908601636, 200.1653181626581102, 23.45113791807856884 ) ) ;
#14077 = CARTESIAN_POINT ( 'NONE',  ( -27.50000000000001066, 13.30988860919481809, -16.28489851701342417 ) ) ;
#14078 = DIRECTION ( 'NONE',  ( 0.000000000000000000, 0.8660254037844380415, -0.5000000000000009992 ) ) ;
#14079 = CARTESIAN_POINT ( 'NONE',  ( 51.52499999726881441, 169.8198683612136222, -4.815267126137197984 ) ) ;
#14080 = CARTESIAN_POINT ( 'NONE',  ( 9.680171189290831535, 199.9079932115568852, 44.30113791807857382 ) ) ;
#14081 = CARTESIAN_POINT ( 'NONE',  ( 0.000000000000000000, 0.000000000000000000, -2.899999999999999911 ) ) ;
#14082 = CARTESIAN_POINT ( 'NONE',  ( -9.984503880673473830, 210.2968891136704315, 90.65113791807854682 ) ) ;
#14083 = CARTESIAN_POINT ( 'NONE',  ( 0.05014649552810506589, 217.5146222423826714, 73.25113791807855534 ) ) ;
#14084 = CIRCLE ( 'NONE', #9180, 5.400000000000002132 ) ;
#14085 = CARTESIAN_POINT ( 'NONE',  ( 9.736236675708031640, 199.9851607334238963, 37.29886208192143471 ) ) ;
#14086 = CARTESIAN_POINT ( 'NONE',  ( -8.118202686958138514, 212.8392687619910930, 41.79886208192143471 ) ) ;
#14087 = CARTESIAN_POINT ( 'NONE',  ( 83.19999999453763451, 146.4771138417591203, 11.73074641843673227 ) ) ;
#14088 = CARTESIAN_POINT ( 'NONE',  ( -9.680171189290831535, 214.0920067884431148, 81.80113791807858092 ) ) ;
#14089 = CARTESIAN_POINT ( 'NONE',  ( -0.05014649552807731031, 198.5883022060938572, 98.75113791807856956 ) ) ;
#14090 = EDGE_CURVE ( 'NONE', #13563, #28748, #32188, .T. ) ;
#14091 = CARTESIAN_POINT ( 'NONE',  ( 10.01549611932659545, 203.7984951890123853, 61.14886208192144323 ) ) ;
#14092 = DIRECTION ( 'NONE',  ( 1.000000000000000000, 0.000000000000000000, 0.000000000000000000 ) ) ;
#14093 = ORIENTED_EDGE ( 'NONE', *, *, #13929, .F. ) ;
#14094 = CARTESIAN_POINT ( 'NONE',  ( -9.680171189290716072, 199.9079932115567146, 62.19886208192144039 ) ) ;
#14095 = VERTEX_POINT ( 'NONE', #24926 ) ;
#14096 = CARTESIAN_POINT ( 'NONE',  ( 73.57499999726880446, 164.1591823560292198, -12.60653300113719766 ) ) ;
#14097 = CARTESIAN_POINT ( 'NONE',  ( -7.984503880673422316, 204.3529502787951628, 38.34886208192142476 ) ) ;
#14098 = ORIENTED_EDGE ( 'NONE', *, *, #13038, .T. ) ;
#14099 = ADVANCED_FACE ( 'NONE', ( #1926 ), #11976, .T. ) ;
#14100 = CARTESIAN_POINT ( 'NONE',  ( 83.67499999726884141, 168.2552932293087906, -9.630534252274387086 ) ) ;
#14101 = PLANE ( 'NONE',  #17318 ) ;
#14102 = LINE ( 'NONE', #11390, #4572 ) ;
#14103 = CARTESIAN_POINT ( 'NONE',  ( -8.015496119326531499, 204.4483345814780364, 54.35113791807857098 ) ) ;
#14104 =( NAMED_UNIT ( * ) PLANE_ANGLE_UNIT ( ) SI_UNIT ( $, .RADIAN. ) );
#14105 = CARTESIAN_POINT ( 'NONE',  ( -8.118202686958138514, 212.8392687619910930, 29.79886208192143826 ) ) ;
#14106 = CARTESIAN_POINT ( 'NONE',  ( 68.67499999726881299, 141.7447067706911810, 9.630534252274376428 ) ) ;
#14107 = ORIENTED_EDGE ( 'NONE', *, *, #17375, .F. ) ;
#14108 = CARTESIAN_POINT ( 'NONE',  ( -54.79999999999999716, -6.711064459327494323E-15, -20.00000000000001776 ) ) ;
#14109 = ADVANCED_FACE ( 'NONE', ( #22361 ), #1739, .F. ) ;
#14110 = FILL_AREA_STYLE_COLOUR ( '', #16538 ) ;
#14111 = DIRECTION ( 'NONE',  ( 1.000000000000000000, 0.000000000000000000, 0.000000000000000000 ) ) ;
#14112 =( BOUNDED_CURVE ( )  B_SPLINE_CURVE ( 2, ( #2584, #7697, #18249, #7361, #15851, #26242, #18080, #2912, #15519, #25911, #12970 ),
 .UNSPECIFIED., .F., .T. ) 
 B_SPLINE_CURVE_WITH_KNOTS ( ( 3, 2, 2, 2, 2, 3 ),
 ( 0.01785714285714299493, 0.02142857142857154673, 0.02500000000000009853, 0.02857142857142864686, 0.03214285714285719520, 0.03571428571428574700 ),
 .UNSPECIFIED. ) 
 CURVE ( )  GEOMETRIC_REPRESENTATION_ITEM ( )  RATIONAL_B_SPLINE_CURVE ( ( 0.9999999999999981126, 0.9510565162951553075, 1.000000000000000000, 0.9510565162951534202, 1.000000000000000000, 0.9510565162951534202, 1.000000000000000000, 0.9510565162951534202, 1.000000000000000000, 0.9510565162951529761, 1.000000000000000444 ) ) 
 REPRESENTATION_ITEM ( '' )  );
#14113 = CARTESIAN_POINT ( 'NONE',  ( 64.50000000000000000, -103.0000000000000000, -30.00000000000000000 ) ) ;
#14114 = CARTESIAN_POINT ( 'NONE',  ( -2.517493886309087880, 214.5937144450984135, 15.09886208192143719 ) ) ;
#14115 = CARTESIAN_POINT ( 'NONE',  ( -0.05014649552810635652, 196.4853777576173002, 62.75113791807856956 ) ) ;
#14116 = CARTESIAN_POINT ( 'NONE',  ( 6.220909254589536808, 215.4770327129947702, 37.55113791807856671 ) ) ;
#14117 = CARTESIAN_POINT ( 'NONE',  ( 2.000000000000000000, 0.8865213383406687075, -1.535500000000000975 ) ) ;
#14118 = CARTESIAN_POINT ( 'NONE',  ( -0.05014649552807731031, 198.5883022060938572, -0.2488620819214341084 ) ) ;
#14119 = CARTESIAN_POINT ( 'NONE',  ( 43.02499999726880020, 149.9369285172503510, -15.58253175000000823 ) ) ;
#14120 = CARTESIAN_POINT ( 'NONE',  ( 35.88867513459481984, 150.1262045565062806, 14.99999999999992006 ) ) ;
#14121 = CARTESIAN_POINT ( 'NONE',  ( 125.5000000000000000, 80.04668119422552763, -74.95331880577366235 ) ) ;
#14122 = CARTESIAN_POINT ( 'NONE',  ( 3.753561863808689836, 218.3979405102790565, 16.40113791807856458 ) ) ;
#14123 = AXIS2_PLACEMENT_3D ( 'NONE', #437, #21048, #14973 ) ;
#14124 = CARTESIAN_POINT ( 'NONE',  ( 82.78867513459482552, 155.0000000000000000, -15.00000000000002487 ) ) ;
#14125 = EDGE_CURVE ( 'NONE', #17153, #14862, #9978, .T. ) ;
#14126 = CARTESIAN_POINT ( 'NONE',  ( 3.135527875058820690, 216.4958274776887492, 61.40113791807857524 ) ) ;
#14127 = CARTESIAN_POINT ( 'NONE',  ( 10.00000000000000711, 206.9523078486586201, 44.00113791807857666 ) ) ;
#14128 = DIRECTION ( 'NONE',  ( 1.000000000000000000, 0.000000000000000000, 0.000000000000000000 ) ) ;
#14129 = DIRECTION ( 'NONE',  ( 1.000000000000000000, 0.000000000000000000, 0.000000000000000000 ) ) ;
#14130 = CARTESIAN_POINT ( 'NONE',  ( 12.01549611932659367, 203.1486557965466773, 7.148862081921435241 ) ) ;
#14131 = CARTESIAN_POINT ( 'NONE',  ( 10.01549611932659367, 203.7984951890124421, 10.14886208192143435 ) ) ;
#14132 = CARTESIAN_POINT ( 'NONE',  ( 67.79999999453762882, 146.4771138417591203, -11.73074641843674470 ) ) ;
#14133 = VERTEX_POINT ( 'NONE', #19978 ) ;
#14134 = CARTESIAN_POINT ( 'NONE',  ( 3.753561863808689836, 218.3979405102790565, 49.40113791807856813 ) ) ;
#14135 = CARTESIAN_POINT ( 'NONE',  ( 4.903702542908601636, 200.1653181626581102, 71.45113791807854398 ) ) ;
#14136 = ADVANCED_FACE ( 'NONE', ( #24591 ), #14314, .T. ) ;
#14137 = CARTESIAN_POINT ( 'NONE',  ( 83.31132485994280046, 140.7341522555726669, -4.635254915624220651 ) ) ;
#14138 = CARTESIAN_POINT ( 'NONE',  ( -9.984503880673420539, 203.7031108863293980, 35.34886208192142476 ) ) ;
#14139 = CARTESIAN_POINT ( 'NONE',  ( -58.50000000000002132, 194.9217985566782829, -2.500000000000000000 ) ) ;
#14140 = ORIENTED_EDGE ( 'NONE', *, *, #8775, .T. ) ;
#14141 = CARTESIAN_POINT ( 'NONE',  ( 6.220909254589536808, 215.4770327129947702, 76.55113791807855250 ) ) ;
#14142 = ORIENTED_EDGE ( 'NONE', *, *, #26799, .F. ) ;
#14143 = DIRECTION ( 'NONE',  ( 0.000000000000000000, -1.000000000000000000, 0.000000000000000000 ) ) ;
#14144 = LINE ( 'NONE', #16527, #18726 ) ;
#14145 = EDGE_LOOP ( 'NONE', ( #3007, #22219 ) ) ;
#14146 = CARTESIAN_POINT ( 'NONE',  ( 7.984503880673485376, 204.3529502787953902, 20.15113791807856458 ) ) ;
#14147 = DIRECTION ( 'NONE',  ( 0.000000000000000000, -1.000000000000000000, 0.000000000000000000 ) ) ;
#14148 = CARTESIAN_POINT ( 'NONE',  ( 3.044812012439969795, 216.5253028482143520, 3.398862081921434797 ) ) ;
#14149 = CARTESIAN_POINT ( 'NONE',  ( 49.47499999726881725, 160.0630714827496206, -15.58253175000000823 ) ) ;
#14150 = ORIENTED_EDGE ( 'NONE', *, *, #17436, .T. ) ;
#14151 = CARTESIAN_POINT ( 'NONE',  ( 58.72499999726881015, 140.1801316387863778, -4.815267126137194431 ) ) ;
#14152 = CARTESIAN_POINT ( 'NONE',  ( -7.984503880673488041, 209.6470497212046098, 48.65113791807857524 ) ) ;
#14153 = DIRECTION ( 'NONE',  ( 0.000000000000000000, 0.000000000000000000, -1.000000000000000000 ) ) ;
#14154 = SURFACE_STYLE_USAGE ( .BOTH. , #17044 ) ;
#14155 = CARTESIAN_POINT ( 'NONE',  ( 27.50000000000000355, 15.87713240271469317, -18.00000000000000000 ) ) ;
#14156 = CARTESIAN_POINT ( 'NONE',  ( 3.044812012439969795, 216.5253028482143520, 93.39886208192143613 ) ) ;
#14157 = CARTESIAN_POINT ( 'NONE',  ( 61.77499999726881441, 169.8198683612136222, -4.815267126137197984 ) ) ;
#14158 = CARTESIAN_POINT ( 'NONE',  ( -6.220909254589537696, 198.5229672870051161, 18.05113791807856671 ) ) ;
#14159 = CARTESIAN_POINT ( 'NONE',  ( 0.000000000000000000, 0.000000000000000000, -9.974600000000000577 ) ) ;
#14160 = EDGE_CURVE ( 'NONE', #27762, #2264, #101, .T. ) ;
#14161 = EDGE_CURVE ( 'NONE', #31418, #19301, #3469, .T. ) ;
#14162 = CARTESIAN_POINT ( 'NONE',  ( 9.736236675708031640, 199.9851607334238963, 79.29886208192144181 ) ) ;
#14163 = AXIS2_PLACEMENT_3D ( 'NONE', #4785, #15178, #25571 ) ;
#14164 = CARTESIAN_POINT ( 'NONE',  ( 79.40000000000000568, 159.7113355953771077, 14.49999999999999289 ) ) ;
#14165 = CARTESIAN_POINT ( 'NONE',  ( 65.28867513459482552, 170.7719333635740497, -7.904646289410545231E-15 ) ) ;
#14166 = FACE_OUTER_BOUND ( 'NONE', #11806, .T. ) ;
#14167 = CARTESIAN_POINT ( 'NONE',  ( -3.044812012440131443, 216.5253028482142952, 94.10113791807857808 ) ) ;
#14168 = CARTESIAN_POINT ( 'NONE',  ( 6.837824896291514243, -3.947820044545437224, -6.564402953523717166 ) ) ;
#14169 = CARTESIAN_POINT ( 'NONE',  ( 43.17499999726881299, 145.8408176439707802, -12.60653300113719588 ) ) ;
#14170 = EDGE_CURVE ( 'NONE', #2840, #10102, #25600, .T. ) ;
#14171 = CARTESIAN_POINT ( 'NONE',  ( -3.135527875058821579, 197.5041725223112223, 41.90113791807856813 ) ) ;
#14172 = CARTESIAN_POINT ( 'NONE',  ( 77.92499999726881299, 164.1591823560292198, 12.60653300113718167 ) ) ;
#14173 = VECTOR ( 'NONE', #13615, 1000.000000000000114 ) ;
#14174 = ORIENTED_EDGE ( 'NONE', *, *, #21659, .F. ) ;
#14175 = CYLINDRICAL_SURFACE ( 'NONE', #5947, 17.00000000000000355 ) ;
#14176 = CARTESIAN_POINT ( 'NONE',  ( 44.49999999453763166, 170.2462022514548323, -7.872454543227099337E-15 ) ) ;
#14177 = CARTESIAN_POINT ( 'NONE',  ( 9.736236675707914401, 214.0148392665762458, 22.70113791807856529 ) ) ;
#14178 = ADVANCED_FACE ( 'NONE', ( #22877 ), #5534, .F. ) ;
#14179 = CARTESIAN_POINT ( 'NONE',  ( -10.66474937096564624, 207.8127639808361948, 102.7602103102857996 ) ) ;
#14180 = LINE ( 'NONE', #22689, #30278 ) ;
#14181 = ORIENTED_EDGE ( 'NONE', *, *, #25989, .T. ) ;
#14182 = CARTESIAN_POINT ( 'NONE',  ( 7.456977232089471386, 196.8216656703012006, 40.44886208192144039 ) ) ;
#14183 = LINE ( 'NONE', #26456, #29013 ) ;
#14184 = CARTESIAN_POINT ( 'NONE',  ( -6.139770520408369237, 215.5359834540460042, 54.95113791807856529 ) ) ;
#14185 = CARTESIAN_POINT ( 'NONE',  ( 2.426778023690075337, 214.6231898156240447, 18.39886208192143613 ) ) ;
#14186 = PRODUCT_DEFINITION_CONTEXT ( 'detailed design', #4855, 'design' ) ;
#14187 = CARTESIAN_POINT ( 'NONE',  ( 50.71132485994280614, 155.0000000000000000, 15.00000000000001243 ) ) ;
#14188 = AXIS2_PLACEMENT_3D ( 'NONE', #14957, #9335, #14446 ) ;
#14189 = ORIENTED_EDGE ( 'NONE', *, *, #19529, .T. ) ;
#14190 = CARTESIAN_POINT ( 'NONE',  ( -8.000000000000008882, 206.9523078486584780, 101.4988620819214304 ) ) ;
#14191 = DIRECTION ( 'NONE',  ( 1.000000000000000000, 0.000000000000000000, 0.000000000000000000 ) ) ;
#14192 = CARTESIAN_POINT ( 'NONE',  ( 0.05014649552807626948, 215.4116977939061144, 37.25113791807857666 ) ) ;
#14193 = CARTESIAN_POINT ( 'NONE',  ( 5.000000000000000000, 0.000000000000000000, 0.000000000000000000 ) ) ;
#14194 = ORIENTED_EDGE ( 'NONE', *, *, #11054, .F. ) ;
#14195 = CARTESIAN_POINT ( 'NONE',  ( 41.02499999726880731, 149.9369285172503510, -15.58253175000000823 ) ) ;
#14196 = CARTESIAN_POINT ( 'NONE',  ( -6.220909254589682469, 215.4770327129946850, 62.94886208192143329 ) ) ;
#14197 = CARTESIAN_POINT ( 'NONE',  ( 43.67499999726881299, 168.2552932293087906, -9.630534252274385310 ) ) ;
#14198 = DIRECTION ( 'NONE',  ( 1.000000000000000000, 0.000000000000000000, 0.000000000000000000 ) ) ;
#14199 = CARTESIAN_POINT ( 'NONE',  ( -2.426778023690262742, 214.6231898156240163, 97.10113791807857808 ) ) ;
#14200 = APPLICATION_CONTEXT ( 'automotive_design' ) ;
#14201 = CARTESIAN_POINT ( 'NONE',  ( 56.20000000000000284, 142.6655632788954620, -8.961492836873480528 ) ) ;
#14202 = CARTESIAN_POINT ( 'NONE',  ( 63.68867513459485252, 159.8737954434935489, 15.00000000000006040 ) ) ;
#14203 = CARTESIAN_POINT ( 'NONE',  ( -4.903702542908436435, 200.1653181626580249, 83.04886208192144181 ) ) ;
#14204 = DIRECTION ( 'NONE',  ( 1.000000000000000000, 0.000000000000000000, 0.000000000000000000 ) ) ;
#14205 = DIRECTION ( 'NONE',  ( 0.000000000000000000, 1.000000000000000000, -1.224646799147353207E-16 ) ) ;
#14206 = CARTESIAN_POINT ( 'NONE',  ( 57.92499999726881299, 164.1591823560292198, 12.60653300113718167 ) ) ;
#14208 = VERTEX_POINT ( 'NONE', #18271 ) ;
#14207 = CARTESIAN_POINT ( 'NONE',  ( 6.139770520408367460, 198.4640165459539389, 20.45113791807856174 ) ) ;
#14209 = DIRECTION ( 'NONE',  ( -1.000000000000000000, 0.000000000000000000, 0.000000000000000000 ) ) ;
#14210 = AXIS2_PLACEMENT_3D ( 'NONE', #17511, #33192, #20583 ) ;
#14211 = CARTESIAN_POINT ( 'NONE',  ( 82.97499999726881015, 140.1801316387863778, -4.815267126137194431 ) ) ;
#14212 = CARTESIAN_POINT ( 'NONE',  ( -3.662846001190052991, 218.4274158808045740, 88.10113791807857808 ) ) ;
#14213 = CARTESIAN_POINT ( 'NONE',  ( 0.05014649552810506589, 217.5146222423826714, 94.25113791807856956 ) ) ;
#14214 = CARTESIAN_POINT ( 'NONE',  ( 32.78867513459481842, 155.0000000000000000, -15.00000000000002487 ) ) ;
#14215 = ORIENTED_EDGE ( 'NONE', *, *, #32690, .F. ) ;
#14216 = CARTESIAN_POINT ( 'NONE',  ( 9.984503880673420539, 210.2968891136705167, 6.848862081921434530 ) ) ;
#14217 = CARTESIAN_POINT ( 'NONE',  ( 11.98450388067341876, 210.9467285061363953, 63.84886208192143187 ) ) ;
#14218 = CARTESIAN_POINT ( 'NONE',  ( -3.135527875058982783, 216.4958274776886924, 72.09886208192143897 ) ) ;
#14219 = CARTESIAN_POINT ( 'NONE',  ( 3.662846001189864698, 218.4274158808046593, 15.39886208192143613 ) ) ;
#14220 = CARTESIAN_POINT ( 'NONE',  ( -67.50001200000001234, 156.1126473981464642, -16.99999999999999645 ) ) ;
#14221 = CARTESIAN_POINT ( 'NONE',  ( 6.139770520408368348, 198.4640165459539674, 23.45113791807856884 ) ) ;
#14222 = CARTESIAN_POINT ( 'NONE',  ( 3.044812012439969795, 216.5253028482143520, 84.39886208192143613 ) ) ;
#14223 = ORIENTED_EDGE ( 'NONE', *, *, #11401, .F. ) ;
#14224 = CARTESIAN_POINT ( 'NONE',  ( -6.500000000000000000, -3.752776749732572803, -6.064240316920399998 ) ) ;
#14225 = ORIENTED_EDGE ( 'NONE', *, *, #10184, .T. ) ;
#14226 = DIRECTION ( 'NONE',  ( -0.000000000000000000, 0.000000000000000000, -1.000000000000000000 ) ) ;
#14227 =( BOUNDED_CURVE ( )  B_SPLINE_CURVE ( 2, ( #32878, #12439, #30162, #4428, #27590, #6993, #29993, #19929, #25049, #6650, #30326 ),
 .UNSPECIFIED., .F., .T. ) 
 B_SPLINE_CURVE_WITH_KNOTS ( ( 3, 2, 2, 2, 2, 3 ),
 ( 0.9107142857142858094, 0.9142857142857143682, 0.9178571428571429269, 0.9214285714285713746, 0.9250000000000000444, 0.9285714285714286031 ),
 .UNSPECIFIED. ) 
 CURVE ( )  GEOMETRIC_REPRESENTATION_ITEM ( )  RATIONAL_B_SPLINE_CURVE ( ( 0.9999999999999984457, 0.9510565162951549745, 1.000000000000000000, 0.9510565162951534202, 1.000000000000000000, 0.9510565162951534202, 1.000000000000000000, 0.9510565162951534202, 1.000000000000000000, 0.9510565162951534202, 1.000000000000000000 ) ) 
 REPRESENTATION_ITEM ( '' )  );
#14228 = CARTESIAN_POINT ( 'NONE',  ( -6.500168698208244500, 211.6636982574061676, 74.79886208192142760 ) ) ;
#14229 = VERTEX_POINT ( 'NONE', #2440 ) ;
#14230 = CARTESIAN_POINT ( 'NONE',  ( 81.12499999726881583, 155.0000000000000000, -15.58253175000000823 ) ) ;
#14231 = ORIENTED_EDGE ( 'NONE', *, *, #12635, .T. ) ;
#14232 = CARTESIAN_POINT ( 'NONE',  ( 68.71132485994280614, 155.0000000000000000, 15.00000000000001243 ) ) ;
#14233 = TOROIDAL_SURFACE ( 'NONE', #25670, 70.00000000000001421, 27.99999999999999645 ) ;
#14234 = CARTESIAN_POINT ( 'NONE',  ( 79.12499999726881583, 155.0000000000000000, -15.58253175000000823 ) ) ;
#14235 = CARTESIAN_POINT ( 'NONE',  ( 2.426778023690261410, 199.3768101843759837, 71.60113791807857808 ) ) ;
#14236 = CARTESIAN_POINT ( 'NONE',  ( 87.49999999999998579, 169.2633224522697333, 5.220106800459117125 ) ) ;
#14237 = AXIS2_PLACEMENT_3D ( 'NONE', #6919, #17310, #14244 ) ;
#14238 = CARTESIAN_POINT ( 'NONE',  ( 34.60000000000000142, 159.7113355953771077, -14.50000000000000888 ) ) ;
#14239 = CARTESIAN_POINT ( 'NONE',  ( -4.984841277089891776, 213.7757310962905990, 44.94886208192144039 ) ) ;
#14240 = CARTESIAN_POINT ( 'NONE',  ( -8.062137200540920645, 212.9164362838581894, 93.80113791807858092 ) ) ;
#14241 = CARTESIAN_POINT ( 'NONE',  ( 9.984503880673470277, 203.7031108863295401, 71.15113791807857524 ) ) ;
#14242 = DIRECTION ( 'NONE',  ( 0.000000000000000000, 0.000000000000000000, 1.000000000000000000 ) ) ;
#14243 = CARTESIAN_POINT ( 'NONE',  ( 130.2500000000000284, -0.6872233929727383783, 35.00001200000001234 ) ) ;
#14244 = DIRECTION ( 'NONE',  ( 0.000000000000000000, 0.000000000000000000, -1.000000000000000000 ) ) ;
#14245 = CARTESIAN_POINT ( 'NONE',  ( 48.82499999726881157, 141.7447067706911810, -9.630534252274387086 ) ) ;
#14246 = CARTESIAN_POINT ( 'NONE',  ( 9.736236675707914401, 214.0148392665762458, 52.70113791807856529 ) ) ;
#14247 = CARTESIAN_POINT ( 'NONE',  ( 41.41132485994280898, 142.2402378747194405, -9.270509831248439525 ) ) ;
#14248 = CARTESIAN_POINT ( 'NONE',  ( 3.753561863808689836, 218.3979405102790565, 4.401137918078566358 ) ) ;
#14249 = EDGE_CURVE ( 'NONE', #15028, #5679, #1735, .T. ) ;
#14250 = CARTESIAN_POINT ( 'NONE',  ( 10.01549611932653860, 210.2015048109876716, 64.85113791807857808 ) ) ;
#14251 = CARTESIAN_POINT ( 'NONE',  ( 12.01549611932659367, 203.1486557965466773, 28.14886208192143968 ) ) ;
#14252 = CARTESIAN_POINT ( 'NONE',  ( -0.05014649552828402690, 217.5146222423826714, 48.24886208192143044 ) ) ;
#14253 = AXIS2_PLACEMENT_3D ( 'NONE', #1387, #30693, #11775 ) ;
#14254 = CARTESIAN_POINT ( 'NONE',  ( 8.542937654374687995, 1.046208125374536008E-15, -6.800000000000000711 ) ) ;
#14255 = CARTESIAN_POINT ( 'NONE',  ( -12.01549611932652972, 203.1486557965464499, 75.35113791807856387 ) ) ;
#14256 = CARTESIAN_POINT ( 'NONE',  ( 6.444103211791042618, 202.2591342207267644, 101.3011379180785951 ) ) ;
#14257 = CARTESIAN_POINT ( 'NONE',  ( 3.135527875058981895, 197.5041725223112792, 55.59886208192143187 ) ) ;
#14258 = CARTESIAN_POINT ( 'NONE',  ( 101.3062541159399075, 155.0000000000000000, 12.00000000000001066 ) ) ;
#14259 = ORIENTED_EDGE ( 'NONE', *, *, #28476, .F. ) ;
#14260 = CARTESIAN_POINT ( 'NONE',  ( -0.05014649552828442242, 219.6175466908591716, 60.24886208192143755 ) ) ;
#14261 = ORIENTED_EDGE ( 'NONE', *, *, #28028, .F. ) ;
#14262 = CARTESIAN_POINT ( 'NONE',  ( 74.67499999726879878, 141.7447067706911810, 9.630534252274376428 ) ) ;
#14263 = CARTESIAN_POINT ( 'NONE',  ( 4.903702542908435547, 213.8346818373419751, 45.54886208192144181 ) ) ;
#14264 = VECTOR ( 'NONE', #13841, 1000.000000000000000 ) ;
#14265 = VERTEX_POINT ( 'NONE', #13157 ) ;
#14266 = CARTESIAN_POINT ( 'NONE',  ( 81.27499999726877888, 149.9369285172503510, -15.58253175000000823 ) ) ;
#14267 = DIRECTION ( 'NONE',  ( 0.000000000000000000, 0.000000000000000000, 1.000000000000000000 ) ) ;
#14268 = CARTESIAN_POINT ( 'NONE',  ( -5.699988423468465015, -4.591578518468254266, -6.344710093416085606 ) ) ;
#14269 = CARTESIAN_POINT ( 'NONE',  ( 7.984503880673485376, 204.3529502787953902, 47.15113791807857524 ) ) ;
#14270 =( NAMED_UNIT ( * ) PLANE_ANGLE_UNIT ( ) SI_UNIT ( $, .RADIAN. ) );
#14271 = CARTESIAN_POINT ( 'NONE',  ( -6.220909254589682469, 215.4770327129946850, 32.94886208192144039 ) ) ;
#14272 = CARTESIAN_POINT ( 'NONE',  ( 70.67499999726881299, 141.7447067706911810, 9.630534252274376428 ) ) ;
#14273 = ORIENTED_EDGE ( 'NONE', *, *, #29256, .F. ) ;
#14274 = DIRECTION ( 'NONE',  ( 0.5000000000000006661, 0.8660254037844383745, -0.000000000000000000 ) ) ;
#14275 = AXIS2_PLACEMENT_3D ( 'NONE', #20117, #24084, #14332 ) ;
#14276 = CARTESIAN_POINT ( 'NONE',  ( 60.00000000000000000, 7.347880794884118356E-15, -20.00000000000000355 ) ) ;
#14277 = CARTESIAN_POINT ( 'NONE',  ( -64.50000000000000000, 0.000000000000000000, -20.00000000000000000 ) ) ;
#14278 = CARTESIAN_POINT ( 'NONE',  ( 8.000000000000008882, 207.0476921513415220, 15.99886208192143577 ) ) ;
#14279 = CARTESIAN_POINT ( 'NONE',  ( 6.139770520408368348, 198.4640165459539674, 62.45113791807857950 ) ) ;
#14280 = CARTESIAN_POINT ( 'NONE',  ( 3.044812012440130555, 197.4746971517856764, 38.60113791807857098 ) ) ;
#14281 = CARTESIAN_POINT ( 'NONE',  ( 87.97499999726882436, 169.8198683612136222, 4.815267126137181997 ) ) ;
#14282 = CARTESIAN_POINT ( 'NONE',  ( -4.984841277089891776, 213.7757310962905990, 101.9488620819214475 ) ) ;
#14283 = AXIS2_PLACEMENT_3D ( 'NONE', #22217, #30230, #6885 ) ;
#14284 = CARTESIAN_POINT ( 'NONE',  ( 48.12499999726880873, 155.0000000000000000, 15.58253174999999402 ) ) ;
#14285 = FACE_OUTER_BOUND ( 'NONE', #26171, .T. ) ;
#14286 = CARTESIAN_POINT ( 'NONE',  ( 34.12499999726881583, 155.0000000000000000, 15.58253174999999402 ) ) ;
#14287 = CARTESIAN_POINT ( 'NONE',  ( 9.680171189290831535, 199.9079932115568852, 17.30113791807856671 ) ) ;
#14288 = DIRECTION ( 'NONE',  ( 1.000000000000000000, 0.000000000000000000, 0.000000000000000000 ) ) ;
#14289 = CIRCLE ( 'NONE', #19179, 32.00000000000002842 ) ;
#14290 = CARTESIAN_POINT ( 'NONE',  ( -6.220909254589537696, 198.5229672870051161, 63.05113791807858092 ) ) ;
#14291 = EDGE_CURVE ( 'NONE', #22951, #22562, #31386, .T. ) ;
#14292 = CARTESIAN_POINT ( 'NONE',  ( -8.118202686958039038, 201.1607312380087080, 42.20113791807857240 ) ) ;
#14293 = CARTESIAN_POINT ( 'NONE',  ( 32.50000000000000000, 155.0000000000000000, -6.938893903907228378E-15 ) ) ;
#14294 = DIRECTION ( 'NONE',  ( 1.000000000000000000, 0.000000000000000000, 0.000000000000000000 ) ) ;
#14295 = CARTESIAN_POINT ( 'NONE',  ( 3.753561863808876797, 195.6020594897209719, 7.598862081921434530 ) ) ;
#14296 = CARTESIAN_POINT ( 'NONE',  ( 9.984503880673420539, 210.2968891136705736, 12.84886208192143364 ) ) ;
#14297 = CARTESIAN_POINT ( 'NONE',  ( 68.69999999453763451, 167.3344367211045096, 8.961492836873468093 ) ) ;
#14298 = VERTEX_POINT ( 'NONE', #10111 ) ;
#14299 = CARTESIAN_POINT ( 'NONE',  ( 9.736236675707914401, 214.0148392665762458, 46.70113791807857240 ) ) ;
#14300 = EDGE_CURVE ( 'NONE', #536, #8949, #11520, .T. ) ;
#14301 = CARTESIAN_POINT ( 'NONE',  ( -7.984503880673488041, 209.6470497212046098, 72.65113791807856103 ) ) ;
#14302 = CARTESIAN_POINT ( 'NONE',  ( -10.00000000000000711, 206.9523078486584495, 26.49886208192143755 ) ) ;
#14303 = SURFACE_SIDE_STYLE ('',( #17371 ) ) ;
#14304 = ORIENTED_EDGE ( 'NONE', *, *, #8147, .F. ) ;
#14305 = EDGE_CURVE ( 'NONE', #4416, #15275, #25875, .T. ) ;
#14306 = AXIS2_PLACEMENT_3D ( 'NONE', #8358, #3739, #18748 ) ;
#14307 = CARTESIAN_POINT ( 'NONE',  ( 3.135527875058820690, 216.4958274776887492, 88.40113791807857524 ) ) ;
#14308 = ORIENTED_EDGE ( 'NONE', *, *, #8275, .F. ) ;
#14309 = FACE_OUTER_BOUND ( 'NONE', #30119, .T. ) ;
#14310 = DIRECTION ( 'NONE',  ( 0.000000000000000000, 1.000000000000000000, 0.000000000000000000 ) ) ;
#14311 = VERTEX_POINT ( 'NONE', #28159 ) ;
#14312 = AXIS2_PLACEMENT_3D ( 'NONE', #23395, #7564, #20829 ) ;
#14313 = CARTESIAN_POINT ( 'NONE',  ( -0.05014649552807731031, 198.5883022060938572, 26.75113791807856956 ) ) ;
#14314 = TOROIDAL_SURFACE ( 'NONE', #8267, 9.624472924841564136, 1.000000000000000444 ) ;
#14315 = CIRCLE ( 'NONE', #7251, 12.00000000000001066 ) ;
#14316 = ADVANCED_FACE ( 'NONE', ( #10288 ), #20667, .T. ) ;
#14317 = DIRECTION ( 'NONE',  ( 0.000000000000000000, -0.04769215134144316748, 0.9988620819214356628 ) ) ;
#14318 = CARTESIAN_POINT ( 'NONE',  ( -10.01549611932659722, 210.2015048109875011, 2.648862081921434797 ) ) ;
#14319 = AXIS2_PLACEMENT_3D ( 'NONE', #2096, #9578, #6859 ) ;
#14320 = CARTESIAN_POINT ( 'NONE',  ( 52.97499999726881015, 140.1801316387863778, -4.815267126137194431 ) ) ;
#14321 = ORIENTED_EDGE ( 'NONE', *, *, #16565, .F. ) ;
#14322 = CARTESIAN_POINT ( 'NONE',  ( -8.000000000000008882, 207.0476921513413515, 51.50113791807856956 ) ) ;
#14323 = CYLINDRICAL_SURFACE ( 'NONE', #10210, 3.499999999999996891 ) ;
#14324 =( NAMED_UNIT ( * ) SI_UNIT ( $, .STERADIAN. ) SOLID_ANGLE_UNIT ( ) );
#14325 = DIRECTION ( 'NONE',  ( -1.000000000000000000, 0.000000000000000000, 0.000000000000000000 ) ) ;
#14326 = CARTESIAN_POINT ( 'NONE',  ( -10.00000000000000711, 206.9523078486584495, 86.49886208192144466 ) ) ;
#14327 = ADVANCED_FACE ( 'NONE', ( #4990 ), #10449, .F. ) ;
#14328 = CARTESIAN_POINT ( 'NONE',  ( 61.17499999726882010, 145.8408176439707802, -12.60653300113719588 ) ) ;
#14329 = CARTESIAN_POINT ( 'NONE',  ( -10.00000000000000711, 207.0476921513413515, 30.50113791807856600 ) ) ;
#14330 = DIRECTION ( 'NONE',  ( 1.000000000000000000, 0.000000000000000000, 0.000000000000000000 ) ) ;
#14331 = CARTESIAN_POINT ( 'NONE',  ( 7.456977232089471386, 196.8216656703012006, 76.44886208192143329 ) ) ;
#14332 = DIRECTION ( 'NONE',  ( 0.000000000000000000, -0.7071067811865437980, 0.7071067811865512365 ) ) ;
#14333 = CIRCLE ( 'NONE', #26299, 10.39117206796836079 ) ;
#14334 = CARTESIAN_POINT ( 'NONE',  ( 78.40000000000000568, 150.2886644046228639, -14.50000000000000888 ) ) ;
#14335 = CARTESIAN_POINT ( 'NONE',  ( -6.830473686658677934E-14, -4.041451884327390331, -2.587392608830344720 ) ) ;
#14336 = PLANE ( 'NONE',  #17516 ) ;
#14337 = STYLED_ITEM ( 'NONE', ( #94 ), #26255 ) ;
#14338 = CARTESIAN_POINT ( 'NONE',  ( -10.00000000000000711, 207.0476921513413515, 99.50113791807856956 ) ) ;
#14339 = DIRECTION ( 'NONE',  ( -1.000000000000000000, 0.000000000000000000, 0.000000000000000000 ) ) ;
#14340 = CARTESIAN_POINT ( 'NONE',  ( 46.27499999726881441, 160.0630714827496206, 15.58253174999999402 ) ) ;
#14341 = CARTESIAN_POINT ( 'NONE',  ( 3.044812012440130555, 197.4746971517856764, 32.60113791807857098 ) ) ;
#14342 = CARTESIAN_POINT ( 'NONE',  ( 80.32499999726880446, 145.8408176439707802, 12.60653300113718345 ) ) ;
#14343 = VERTEX_POINT ( 'NONE', #12995 ) ;
#14344 = CARTESIAN_POINT ( 'NONE',  ( -65.20000000000000284, -7.347880794884118356E-15, -19.30000000000003979 ) ) ;
#14345 = CARTESIAN_POINT ( 'NONE',  ( 49.11132485994281183, 140.7341522555726669, 4.635254915624211769 ) ) ;
#14346 = AXIS2_PLACEMENT_3D ( 'NONE', #9383, #20115, #30507 ) ;
#14347 = CARTESIAN_POINT ( 'NONE',  ( 44.69999999453762030, 167.3344367211045096, 8.961492836873468093 ) ) ;
#14348 = CARTESIAN_POINT ( 'NONE',  ( 12.01549611932652972, 210.8513442034534933, 16.85113791807856742 ) ) ;
#14349 = CIRCLE ( 'NONE', #4548, 100.0000000000000000 ) ;
#14350 = FACE_OUTER_BOUND ( 'NONE', #13024, .T. ) ;
#14351 = CIRCLE ( 'NONE', #4010, 98.00000000000002842 ) ;
#14352 = CARTESIAN_POINT ( 'NONE',  ( -67.50000000000000000, 122.1366465496900275, 17.00000000000001421 ) ) ;
#14353 = ORIENTED_EDGE ( 'NONE', *, *, #18063, .T. ) ;
#14354 = CARTESIAN_POINT ( 'NONE',  ( -7.375838497908014268, 196.7627149292498530, 38.04886208192144181 ) ) ;
#14355 = CARTESIAN_POINT ( 'NONE',  ( -10.01549611932653860, 203.7984951890123284, 0.3511379180785655363 ) ) ;
#14356 = CARTESIAN_POINT ( 'NONE',  ( -10.00000000000000711, 207.0476921513413515, 63.50113791807856956 ) ) ;
#14357 = CARTESIAN_POINT ( 'NONE',  ( 8.000000000000008882, 207.0476921513415220, 12.99886208192143400 ) ) ;
#14358 = ADVANCED_FACE ( 'NONE', ( #15874 ), #11017, .F. ) ;
#14359 = AXIS2_PLACEMENT_3D ( 'NONE', #29535, #584, #914 ) ;
#14360 = DIRECTION ( 'NONE',  ( 0.000000000000000000, 0.000000000000000000, 1.000000000000000000 ) ) ;
#14361 = ORIENTED_EDGE ( 'NONE', *, *, #28569, .F. ) ;
#14362 = CARTESIAN_POINT ( 'NONE',  ( -8.050845014156799095, 215.4811768934071665, 104.9910338291041114 ) ) ;
#14363 = EDGE_CURVE ( 'NONE', #13342, #4045, #3388, .T. ) ;
#14364 = FACE_OUTER_BOUND ( 'NONE', #3535, .T. ) ;
#14365 = CARTESIAN_POINT ( 'NONE',  ( -0.05014649552807731031, 198.5883022060938572, 41.75113791807856956 ) ) ;
#14366 = DIRECTION ( 'NONE',  ( 1.000000000000000000, 0.000000000000000000, 0.000000000000000000 ) ) ;
#14367 = ORIENTED_EDGE ( 'NONE', *, *, #28754, .F. ) ;
#14368 = CARTESIAN_POINT ( 'NONE',  ( 37.42499999726881299, 168.2552932293087906, -9.630534252274385310 ) ) ;
#14369 = CARTESIAN_POINT ( 'NONE',  ( 99.17200000000002547, 6.123233995736768255E-16, -5.000000000000000888 ) ) ;
#14370 = AXIS2_PLACEMENT_3D ( 'NONE', #26903, #21784, #21957 ) ;
#14371 = CARTESIAN_POINT ( 'NONE',  ( -0.05014649552828403384, 217.5146222423826714, 63.24886208192143755 ) ) ;
#14372 = AXIS2_PLACEMENT_3D ( 'NONE', #5795, #16695, #13809 ) ;
#14373 = EDGE_CURVE ( 'NONE', #25209, #8611, #31872, .T. ) ;
#14374 = CARTESIAN_POINT ( 'NONE',  ( 39.67499999726881299, 168.2552932293087906, -9.630534252274385310 ) ) ;
#14375 = CARTESIAN_POINT ( 'NONE',  ( 42.50000000000000000, -103.0000000000000142, 20.00000000000000355 ) ) ;
#14376 = CARTESIAN_POINT ( 'NONE',  ( -10.00000000000000711, 207.0476921513413515, 6.501137918078566003 ) ) ;
#14377 = CARTESIAN_POINT ( 'NONE',  ( 63.50000000000000000, 155.0000000000000000, 14.49999999999999467 ) ) ;
#14378 = CARTESIAN_POINT ( 'NONE',  ( -125.0000000000000000, 0.000000000000000000, 35.00200000000000244 ) ) ;
#14379 = CARTESIAN_POINT ( 'NONE',  ( 7.984503880673422316, 209.6470497212048372, 81.84886208192142476 ) ) ;
#14380 = CARTESIAN_POINT ( 'NONE',  ( 4.000000000000000000, -1.759474945355381958, 3.047500000000001208 ) ) ;
#14381 = LINE ( 'NONE', #7054, #26988 ) ;
#14382 =( BOUNDED_CURVE ( )  B_SPLINE_CURVE ( 2, ( #14560, #19169, #11508, #32445, #19674, #940, #11174, #24623, #26832, #1449, #11842 ),
 .UNSPECIFIED., .F., .T. ) 
 B_SPLINE_CURVE_WITH_KNOTS ( ( 3, 2, 2, 2, 2, 3 ),
 ( 0.5178571428571429047, 0.5214285714285714635, 0.5250000000000000222, 0.5285714285714284699, 0.5321428571428570287, 0.5357142857142855874 ),
 .UNSPECIFIED. ) 
 CURVE ( )  GEOMETRIC_REPRESENTATION_ITEM ( )  RATIONAL_B_SPLINE_CURVE ( ( 1.000000000000000000, 0.9510565162951534202, 1.000000000000000000, 0.9510565162951534202, 1.000000000000000000, 0.9510565162951534202, 1.000000000000000000, 0.9510565162951534202, 1.000000000000000000, 0.9510565162951549745, 0.9999999999999984457 ) ) 
 REPRESENTATION_ITEM ( '' )  );
#14383 = CARTESIAN_POINT ( 'NONE',  ( 62.42499999726881299, 141.7447067706911810, 9.630534252274376428 ) ) ;
#14385 = ORIENTED_EDGE ( 'NONE', *, *, #17675, .T. ) ;
#14384 = CARTESIAN_POINT ( 'NONE',  ( 3.135527875058820690, 216.4958274776887492, 22.40113791807856458 ) ) ;
#14386 = FACE_OUTER_BOUND ( 'NONE', #21182, .T. ) ;
#14387 = CARTESIAN_POINT ( 'NONE',  ( 85.47499999726879594, 160.0630714827496206, -15.58253175000000823 ) ) ;
#14388 = CARTESIAN_POINT ( 'NONE',  ( -11.98450388067348804, 210.9467285061362247, 87.65113791807857524 ) ) ;
#14389 = CARTESIAN_POINT ( 'NONE',  ( 71.88867513459481984, 150.1262045565060816, 14.99999999999978328 ) ) ;
#14390 = CARTESIAN_POINT ( 'NONE',  ( 53.38867513459481984, 169.2658477444273331, 4.635254915624208216 ) ) ;
#14391 = ORIENTED_EDGE ( 'NONE', *, *, #9678, .T. ) ;
#14392 = CARTESIAN_POINT ( 'NONE',  ( -3.662846001189865142, 195.5725841191952838, 70.89886208192143613 ) ) ;
#14393 = CARTESIAN_POINT ( 'NONE',  ( -0.05014649552828402690, 217.5146222423826714, 81.24886208192141623 ) ) ;
#14394 = CONICAL_SURFACE ( 'NONE', #31792, 11.99999999999998224, 0.1047197551197030924 ) ;
#14395 = CARTESIAN_POINT ( 'NONE',  ( 3.662846001189864698, 218.4274158808046593, 12.39886208192143613 ) ) ;
#14396 = DIRECTION ( 'NONE',  ( -0.000000000000000000, -0.000000000000000000, -1.000000000000000000 ) ) ;
#14397 = CARTESIAN_POINT ( 'NONE',  ( -10.01549611932653860, 203.7984951890123284, 24.35113791807855677 ) ) ;
#14398 = CARTESIAN_POINT ( 'NONE',  ( -10.00000000000000711, 206.9523078486584495, 89.49886208192144466 ) ) ;
#14399 = EDGE_CURVE ( 'NONE', #2009, #8990, #19099, .T. ) ;
#14400 = CARTESIAN_POINT ( 'NONE',  ( 2.141486166123590884, -6.269165884987830673, -0.07763482564821427845 ) ) ;
#14401 = ORIENTED_EDGE ( 'NONE', *, *, #12476, .T. ) ;
#14402 = DIRECTION ( 'NONE',  ( -1.000000000000000000, -0.000000000000000000, -0.000000000000000000 ) ) ;
#14403 = CARTESIAN_POINT ( 'NONE',  ( 8.000000000000008882, 207.0476921513415220, 75.99886208192144466 ) ) ;
#14404 = EDGE_LOOP ( 'NONE', ( #19552, #16194, #32392, #30522 ) ) ;
#14405 = ADVANCED_FACE ( 'NONE', ( #373 ), #25155, .F. ) ;
#14406 = CARTESIAN_POINT ( 'NONE',  ( 82.32499999726880446, 145.8408176439707802, 12.60653300113718345 ) ) ;
#14407 = ORIENTED_EDGE ( 'NONE', *, *, #10231, .F. ) ;
#14408 = CARTESIAN_POINT ( 'NONE',  ( 79.22499999726879594, 160.0630714827496206, -15.58253175000000823 ) ) ;
#14409 = FACE_OUTER_BOUND ( 'NONE', #9837, .T. ) ;
#14410 = CARTESIAN_POINT ( 'NONE',  ( 2.517493886308900919, 214.5937144450984420, 64.40113791807856103 ) ) ;
#14411 = CARTESIAN_POINT ( 'NONE',  ( 87.50000000000004263, 170.3440178963778351, 0.6416442768189705159 ) ) ;
#14412 = CARTESIAN_POINT ( 'NONE',  ( 40.30000000000000426, 146.4771138417591203, -11.73074641843674470 ) ) ;
#14413 = CARTESIAN_POINT ( 'NONE',  ( -0.05014649552828365914, 215.4116977939061144, 51.24886208192144466 ) ) ;
#14414 = DIRECTION ( 'NONE',  ( 0.1045284632676459352, 0.000000000000000000, -0.9945218953682740670 ) ) ;
#14415 = FACE_OUTER_BOUND ( 'NONE', #24442, .T. ) ;
#14416 = CARTESIAN_POINT ( 'NONE',  ( 0.000000000000000000, 0.000000000000000000, -18.00000000000000000 ) ) ;
#14417 = CARTESIAN_POINT ( 'NONE',  ( 48.02499999726879309, 160.0630714827496206, 15.58253174999999224 ) ) ;
#14418 = CARTESIAN_POINT ( 'NONE',  ( 9.680171189290831535, 199.9079932115568852, 59.30113791807857382 ) ) ;
#14419 = CARTESIAN_POINT ( 'NONE',  ( -130.1133565525086908, -1.374176392886221620, 35.00001199999999812 ) ) ;
#14420 = CARTESIAN_POINT ( 'NONE',  ( -9.898309971686792608, 228.3698647632124334, 103.4854814124440452 ) ) ;
#14421 = CARTESIAN_POINT ( 'NONE',  ( 6.220909254589536808, 215.4770327129947987, 76.55113791807856671 ) ) ;
#14422 = CARTESIAN_POINT ( 'NONE',  ( -7.375838497908014268, 196.7627149292498530, 44.04886208192143471 ) ) ;
#14423 = CARTESIAN_POINT ( 'NONE',  ( -0.05014649552828402690, 217.5146222423826714, 45.24886208192143755 ) ) ;
#14424 = CARTESIAN_POINT ( 'NONE',  ( 84.99999999453764588, 155.0000000000000000, 14.49999999999999467 ) ) ;
#14425 =( BOUNDED_SURFACE ( )  B_SPLINE_SURFACE ( 3, 2, ( 
 ( #7636, #17844, #18019 ),
 ( #4900, #23631, #10530 ),
 ( #12739, #12903, #31305 ),
 ( #28410, #23129, #7799 ),
 ( #7968, #10364, #28745 ),
 ( #5068, #20738, #15620 ),
 ( #5405, #31134, #15789 ),
 ( #18189, #5232, #7299 ) ),
 .UNSPECIFIED., .F., .F., .F. ) 
 B_SPLINE_SURFACE_WITH_KNOTS ( ( 4, 2, 2, 4 ),
 ( 3, 3 ),
 ( 0.03851319102641418551, 0.04314724750133520914, 0.04546427573879571749, 0.04778130397625623277 ),
 ( 0.000000000000000000, 1.000000000000000000 ),
 .UNSPECIFIED. ) 
 GEOMETRIC_REPRESENTATION_ITEM ( )  RATIONAL_B_SPLINE_SURFACE ( (
 ( 1.000000000000000000, 0.8047781573724569482, 1.000000000000000000),
 ( 1.000000000000000000, 0.8123768202405010630, 1.000000000000000000),
 ( 1.000000000000000000, 0.8190667609311549358, 1.000000000000000000),
 ( 1.000000000000000000, 0.8191933927154739781, 1.000000000000000000),
 ( 1.000000000000000000, 0.8176088169850088683, 1.000000000000000000),
 ( 1.000000000000000000, 0.8122958474542694152, 1.000000000000000000),
 ( 1.000000000000000000, 0.8086309703845098174, 1.000000000000000000),
 ( 1.000000000000000000, 0.8047712409910821041, 1.000000000000000000) ) ) 
 REPRESENTATION_ITEM ( '' )  SURFACE ( )  );
#14426 = CARTESIAN_POINT ( 'NONE',  ( -3.662846001190052991, 218.4274158808045740, 85.10113791807857808 ) ) ;
#14427 = CARTESIAN_POINT ( 'NONE',  ( -7.984503880673488041, 209.6470497212046098, 93.65113791807857524 ) ) ;
#14428 = CARTESIAN_POINT ( 'NONE',  ( -0.05014649552828403384, 217.5146222423826714, 57.24886208192144466 ) ) ;
#14429 = CYLINDRICAL_SURFACE ( 'NONE', #16140, 15.00000000000001776 ) ;
#14430 = ORIENTED_EDGE ( 'NONE', *, *, #30538, .F. ) ;
#14431 = CARTESIAN_POINT ( 'NONE',  ( -7.456977232089471386, 217.1783343296987709, 65.94886208192144750 ) ) ;
#14432 = ORIENTED_EDGE ( 'NONE', *, *, #30843, .F. ) ;
#14433 = CARTESIAN_POINT ( 'NONE',  ( 72.87499999726881583, 138.6155565068815463, -3.929120461958505118E-15 ) ) ;
#14434 = CARTESIAN_POINT ( 'NONE',  ( -0.05014649552828365914, 215.4116977939061144, 39.24886208192144466 ) ) ;
#14435 = ORIENTED_EDGE ( 'NONE', *, *, #12185, .F. ) ;
#14436 = ADVANCED_FACE ( 'NONE', ( #5806 ), #26269, .F. ) ;
#14437 = CARTESIAN_POINT ( 'NONE',  ( 82.07499999726880446, 168.2552932293087906, 9.630534252274372875 ) ) ;
#14438 = FACE_OUTER_BOUND ( 'NONE', #20866, .T. ) ;
#14439 = CARTESIAN_POINT ( 'NONE',  ( 125.5000000000000000, 155.0000000000010800, 106.0000000000000142 ) ) ;
#14440 = CARTESIAN_POINT ( 'NONE',  ( -7.984503880673488041, 209.6470497212046098, 60.65113791807856813 ) ) ;
#14441 = LINE ( 'NONE', #11893, #9093 ) ;
#14442 = CARTESIAN_POINT ( 'NONE',  ( -6.139770520408224463, 198.4640165459539389, 47.04886208192142050 ) ) ;
#14443 = ORIENTED_EDGE ( 'NONE', *, *, #17799, .F. ) ;
#14444 = CYLINDRICAL_SURFACE ( 'NONE', #21085, 24.99999999999999289 ) ;
#14445 = CARTESIAN_POINT ( 'NONE',  ( 48.78867513459482552, 155.0000000000000000, -15.00000000000002487 ) ) ;
#14446 = DIRECTION ( 'NONE',  ( 0.000000000000000000, 0.000000000000000000, 1.000000000000000000 ) ) ;
#14447 = CARTESIAN_POINT ( 'NONE',  ( -2.426778023690076225, 199.3768101843759553, 25.89886208192143613 ) ) ;
#14448 = CARTESIAN_POINT ( 'NONE',  ( 10.01549611932653860, 210.2015048109876716, 58.85113791807856387 ) ) ;
#14449 = CARTESIAN_POINT ( 'NONE',  ( 8.118202686958039038, 212.8392687619912635, 43.70113791807857240 ) ) ;
#14450 = CARTESIAN_POINT ( 'NONE',  ( 71.21132485994279193, 139.2280666364260071, -4.041636747397287284E-15 ) ) ;
#14451 = CARTESIAN_POINT ( 'NONE',  ( -6.220909254589537696, 198.5229672870051161, 21.05113791807855961 ) ) ;
#14452 = CARTESIAN_POINT ( 'NONE',  ( 4.903702542908435547, 213.8346818373419751, 102.5488620819214560 ) ) ;
#14453 = CARTESIAN_POINT ( 'NONE',  ( 42.72499999726881015, 140.1801316387863778, -4.815267126137194431 ) ) ;
#14454 = DIRECTION ( 'NONE',  ( -0.000000000000000000, -0.000000000000000000, 1.000000000000000000 ) ) ;
#14455 = CARTESIAN_POINT ( 'NONE',  ( 9.736236675707914401, 214.0148392665762458, 25.70113791807857240 ) ) ;
#14456 = CARTESIAN_POINT ( 'NONE',  ( 111.1125082318798007, 155.0000000000000000, 0.000000000000000000 ) ) ;
#14457 = CARTESIAN_POINT ( 'NONE',  ( -10.01549611932653860, 203.7984951890123284, 78.35113791807857808 ) ) ;
#14458 = CARTESIAN_POINT ( 'NONE',  ( 8.118202686958039038, 212.8392687619912635, 46.70113791807857240 ) ) ;
#14459 = DIRECTION ( 'NONE',  ( 1.000000000000000000, 0.000000000000000000, 0.000000000000000000 ) ) ;
#14460 = CARTESIAN_POINT ( 'NONE',  ( 60.63708498984762940, 120.3589838486224437, 20.00000000000000000 ) ) ;
#14461 = CARTESIAN_POINT ( 'NONE',  ( -11.94915498584342295, 219.8409957184640291, 102.9933096652613642 ) ) ;
#14462 = CARTESIAN_POINT ( 'NONE',  ( 0.05014649552828275014, 196.4853777576173002, 19.74886208192143400 ) ) ;
#14463 = CARTESIAN_POINT ( 'NONE',  ( 69.39999999453763735, 141.2096805137202580, 4.480746418436733158 ) ) ;
#14464 = ORIENTED_EDGE ( 'NONE', *, *, #30138, .F. ) ;
#14465 = CARTESIAN_POINT ( 'NONE',  ( -3.753561863808691168, 195.6020594897209435, 59.90113791807856103 ) ) ;
#14466 = CARTESIAN_POINT ( 'NONE',  ( -7.984503880673488041, 209.6470497212046098, 66.65113791807856103 ) ) ;
#14467 = CARTESIAN_POINT ( 'NONE',  ( 9.984503880673420539, 210.2968891136705167, 27.84886208192143187 ) ) ;
#14468 = AXIS2_PLACEMENT_3D ( 'NONE', #25147, #20210, #9480 ) ;
#14469 = PRESENTATION_STYLE_ASSIGNMENT (( #24704 ) ) ;
#14470 = ORIENTED_EDGE ( 'NONE', *, *, #9834, .T. ) ;
#14471 = CARTESIAN_POINT ( 'NONE',  ( -0.05014649552810635652, 196.4853777576173002, 86.75113791807858377 ) ) ;
#14472 = ORIENTED_EDGE ( 'NONE', *, *, #12896, .T. ) ;
#14473 = DIRECTION ( 'NONE',  ( 0.000000000000000000, 0.000000000000000000, -1.000000000000000000 ) ) ;
#14474 = DIRECTION ( 'NONE',  ( 0.000000000000000000, 0.000000000000000000, 1.000000000000000000 ) ) ;
#14475 = EDGE_LOOP ( 'NONE', ( #11050, #28246, #11436, #23536 ) ) ;
#14476 = CARTESIAN_POINT ( 'NONE',  ( -6.500168698208129925, 202.3363017425936050, 30.20113791807856529 ) ) ;
#14477 = PLANE ( 'NONE',  #18872 ) ;
#14478 = ADVANCED_FACE ( 'NONE', ( #23712 ), #10777, .T. ) ;
#14479 = CARTESIAN_POINT ( 'NONE',  ( -0.05014649552828403384, 217.5146222423826714, 18.24886208192143755 ) ) ;
#14480 = CARTESIAN_POINT ( 'NONE',  ( 48.47499999726881015, 149.9369285172503510, 15.58253174999999580 ) ) ;
#14481 = ORIENTED_EDGE ( 'NONE', *, *, #31027, .F. ) ;
#14482 = CARTESIAN_POINT ( 'NONE',  ( -4.903702542908602524, 213.8346818373418898, 51.95113791807857240 ) ) ;
#14483 = CARTESIAN_POINT ( 'NONE',  ( 78.00000000000001421, 0.000000000000000000, 0.000000000000000000 ) ) ;
#14484 = CARTESIAN_POINT ( 'NONE',  ( 125.5000000000000000, 155.0000000000000000, -6.938893903907228378E-15 ) ) ;
#14485 = CARTESIAN_POINT ( 'NONE',  ( -9.984503880673420539, 203.7031108863293980, 86.34886208192143897 ) ) ;
#14486 = CARTESIAN_POINT ( 'NONE',  ( 59.07499999726880446, 141.7447067706911810, -9.630534252274385310 ) ) ;
#14487 = CARTESIAN_POINT ( 'NONE',  ( -8.062137200540920645, 212.9164362838581894, 33.80113791807857382 ) ) ;
#14488 = CARTESIAN_POINT ( 'NONE',  ( 69.98867513459484258, 146.1832212156128890, 12.13525491562421976 ) ) ;
#14489 = CARTESIAN_POINT ( 'NONE',  ( 8.118202686958039038, 212.8392687619912635, 22.70113791807856884 ) ) ;
#14490 = AXIS2_PLACEMENT_3D ( 'NONE', #8731, #33673, #11292 ) ;
#14491 = DIRECTION ( 'NONE',  ( 0.000000000000000000, 0.7071067811865487940, 0.7071067811865463515 ) ) ;
#14492 = EDGE_CURVE ( 'NONE', #31949, #20089, #10495, .T. ) ;
#14493 = AXIS2_PLACEMENT_3D ( 'NONE', #22390, #7408, #20353 ) ;
#14494 = CARTESIAN_POINT ( 'NONE',  ( 77.70000000000000284, 146.4771138417591203, 11.73074641843673227 ) ) ;
#14495 = DIRECTION ( 'NONE',  ( 1.000000000000000000, 0.000000000000000000, 0.000000000000000000 ) ) ;
#14496 = CARTESIAN_POINT ( 'NONE',  ( 8.062137200540920645, 201.0835637161417822, 92.30113791807858092 ) ) ;
#14497 = CARTESIAN_POINT ( 'NONE',  ( 101.3062541159399075, 155.0000000000000000, 0.000000000000000000 ) ) ;
#14498 = CARTESIAN_POINT ( 'NONE',  ( 42.67499999726880588, 141.7447067706911810, 9.630534252274376428 ) ) ;
#14499 = CARTESIAN_POINT ( 'NONE',  ( -3.135527875058821579, 197.5041725223112223, 47.90113791807857524 ) ) ;
#14500 = VECTOR ( 'NONE', #2942, 1000.000000000000000 ) ;
#14501 = CARTESIAN_POINT ( 'NONE',  ( 85.92499999726881299, 164.1591823560292198, 12.60653300113718167 ) ) ;
#14502 = DIRECTION ( 'NONE',  ( -1.000000000000000000, -0.000000000000000000, -0.000000000000000000 ) ) ;
#14503 = DIRECTION ( 'NONE',  ( 0.000000000000000000, 0.000000000000000000, -1.000000000000000000 ) ) ;
#14504 = CARTESIAN_POINT ( 'NONE',  ( 50.09999999453762598, 159.7113355953771077, -14.50000000000000888 ) ) ;
#14505 = ORIENTED_EDGE ( 'NONE', *, *, #31181, .F. ) ;
#14506 = CARTESIAN_POINT ( 'NONE',  ( -12.01549611932652972, 203.1486557965464499, 21.35113791807856742 ) ) ;
#14507 = CARTESIAN_POINT ( 'NONE',  ( -31.74999999999995737, 0.000000000000000000, 0.000000000000000000 ) ) ;
#14508 = CARTESIAN_POINT ( 'NONE',  ( 5.000000000000000888, 0.000000000000000000, 0.000000000000000000 ) ) ;
#14509 = ORIENTED_EDGE ( 'NONE', *, *, #21802, .T. ) ;
#14510 = CARTESIAN_POINT ( 'NONE',  ( 9.736236675708031640, 199.9851607334238963, 43.29886208192143471 ) ) ;
#14511 = DIRECTION ( 'NONE',  ( 0.000000000000000000, 0.000000000000000000, -1.000000000000000000 ) ) ;
#14512 = CARTESIAN_POINT ( 'NONE',  ( -8.118202686958039038, 201.1607312380087080, 60.20113791807857240 ) ) ;
#14513 = ADVANCED_FACE ( 'NONE', ( #29155 ), #23516, .F. ) ;
#14514 = CARTESIAN_POINT ( 'NONE',  ( -8.015496119326597224, 209.5516654185217362, 26.64886208192143968 ) ) ;
#14515 = VECTOR ( 'NONE', #543, 1000.000000000000000 ) ;
#14516 = CARTESIAN_POINT ( 'NONE',  ( 49.88867513459483405, 150.1262045565061385, 14.99999999999982947 ) ) ;
#14517 = ORIENTED_EDGE ( 'NONE', *, *, #31606, .F. ) ;
#14518 = CARTESIAN_POINT ( 'NONE',  ( 2.426778023690075337, 214.6231898156240447, 99.39886208192146455 ) ) ;
#14519 = ADVANCED_FACE ( 'NONE', ( #6143 ), #28993, .T. ) ;
#14520 = PLANE ( 'NONE',  #23576 ) ;
#14521 = CARTESIAN_POINT ( 'NONE',  ( 6.444103211791042618, 202.2591342207267644, 38.30113791807856671 ) ) ;
#14522 = CARTESIAN_POINT ( 'NONE',  ( -64.50000000000000000, 155.0000000000000000, 40.00000000000001421 ) ) ;
#14524 = EDGE_LOOP ( 'NONE', ( #25857, #13422, #15369, #32731 ) ) ;
#14523 = AXIS2_PLACEMENT_3D ( 'NONE', #267, #15919, #10984 ) ;
#14525 = CARTESIAN_POINT ( 'NONE',  ( 34.92499999726881299, 145.8408176439707802, -12.60653300113719588 ) ) ;
#14526 = DIRECTION ( 'NONE',  ( 1.000000000000000000, 0.000000000000000000, 0.000000000000000000 ) ) ;
#14527 = CARTESIAN_POINT ( 'NONE',  ( -8.118202686958039038, 201.1607312380087080, 3.201137918078566180 ) ) ;
#14528 = CARTESIAN_POINT ( 'NONE',  ( -0.05014649552828403384, 217.5146222423826714, 57.24886208192144466 ) ) ;
#14529 = CARTESIAN_POINT ( 'NONE',  ( 39.17499999726881299, 145.8408176439707802, -12.60653300113719588 ) ) ;
#14530 = FACE_OUTER_BOUND ( 'NONE', #2688, .T. ) ;
#14531 = CARTESIAN_POINT ( 'NONE',  ( 10.00000000000000711, 206.9523078486586201, 2.001137918078565558 ) ) ;
#14532 = CARTESIAN_POINT ( 'NONE',  ( -18.40782811468575986, -21.12650028821925829, -0.2827231011780881320 ) ) ;
#14533 = EDGE_CURVE ( 'NONE', #28972, #4473, #10940, .T. ) ;
#14534 = CARTESIAN_POINT ( 'NONE',  ( 58.10000000000000142, 141.2096805137202580, -4.480746418436742040 ) ) ;
#14535 = CARTESIAN_POINT ( 'NONE',  ( -27.50000000000000000, -15.87713240271474824, -2.456200930618646971 ) ) ;
#14536 = CARTESIAN_POINT ( 'NONE',  ( -2.517493886309087880, 214.5937144450984135, 78.09886208192142476 ) ) ;
#14537 = AXIS2_PLACEMENT_3D ( 'NONE', #17210, #12104, #4265 ) ;
#14538 = CARTESIAN_POINT ( 'NONE',  ( -4.599534470795546781, 6.460478697738500031, -7.590212325761530821 ) ) ;
#14539 = DIRECTION ( 'NONE',  ( -1.000000000000000000, 0.000000000000000000, 0.000000000000000000 ) ) ;
#14540 = CONICAL_SURFACE ( 'NONE', #946, 3.499999999999999556, 1.047197551196589638 ) ;
#14541 = CARTESIAN_POINT ( 'NONE',  ( 67.02499999726882152, 149.9369285172503510, -15.58253175000000823 ) ) ;
#14542 = AXIS2_PLACEMENT_3D ( 'NONE', #23298, #13072, #30800 ) ;
#14544 = EDGE_LOOP ( 'NONE', ( #6648, #11753, #9236, #16023, #11588 ) ) ;
#14543 = CARTESIAN_POINT ( 'NONE',  ( -10.00000000000000711, 207.0476921513413515, 18.50113791807856956 ) ) ;
#14545 = CIRCLE ( 'NONE', #6860, 2.149999999999985256 ) ;
#14546 = CARTESIAN_POINT ( 'NONE',  ( 6.938893903907228378E-15, 31.75426480542944319, -2.456200930618646971 ) ) ;
#14547 = CARTESIAN_POINT ( 'NONE',  ( 83.37499999726881583, 155.0000000000000000, -15.58253175000000823 ) ) ;
#14548 = CARTESIAN_POINT ( 'NONE',  ( 3.753561863808689836, 218.3979405102790565, 82.40113791807856103 ) ) ;
#14549 = EDGE_CURVE ( 'NONE', #20617, #24401, #16203, .T. ) ;
#14550 = CARTESIAN_POINT ( 'NONE',  ( 5.000000000000000000, 0.000000000000000000, 0.000000000000000000 ) ) ;
#14551 = AXIS2_PLACEMENT_3D ( 'NONE', #17434, #4487, #25272 ) ;
#14552 = ORIENTED_EDGE ( 'NONE', *, *, #7998, .T. ) ;
#14553 = CARTESIAN_POINT ( 'NONE',  ( -7.456977232089471386, 217.1783343296987709, 71.94886208192144750 ) ) ;
#14554 = CARTESIAN_POINT ( 'NONE',  ( 3.135527875058981895, 197.5041725223112792, 79.59886208192143897 ) ) ;
#14555 = CARTESIAN_POINT ( 'NONE',  ( 3.753561863808876797, 195.6020594897209719, 16.59886208192143187 ) ) ;
#14556 = CARTESIAN_POINT ( 'NONE',  ( -27.50000000000000000, -15.87713240271474824, -15.54379906938135214 ) ) ;
#14557 = CARTESIAN_POINT ( 'NONE',  ( 10.01549611932653860, 210.2015048109876716, 31.85113791807857453 ) ) ;
#14558 = DIRECTION ( 'NONE',  ( 1.000000000000000000, -0.000000000000000000, -0.000000000000000000 ) ) ;
#14559 = CARTESIAN_POINT ( 'NONE',  ( 0.05014649552828275708, 196.4853777576173002, 85.74886208192140202 ) ) ;
#14560 = CARTESIAN_POINT ( 'NONE',  ( 62.71132485994281325, 155.0000000000000000, 15.00000000000001243 ) ) ;
#14561 = VERTEX_POINT ( 'NONE', #21488 ) ;
#14562 = DIRECTION ( 'NONE',  ( -1.000000000000000000, -1.804112415015879625E-16, 0.000000000000000000 ) ) ;
#14563 = CARTESIAN_POINT ( 'NONE',  ( -6.500168698208244500, 211.6636982574061676, 71.79886208192142760 ) ) ;
#14564 = CIRCLE ( 'NONE', #4221, 2.149999999999985256 ) ;
#14565 = VERTEX_POINT ( 'NONE', #26592 ) ;
#14566 = AXIS2_PLACEMENT_3D ( 'NONE', #538, #5794, #16192 ) ;
#14567 = CARTESIAN_POINT ( 'NONE',  ( 86.02499999726880731, 160.0630714827496206, 15.58253174999999224 ) ) ;
#14568 = ORIENTED_EDGE ( 'NONE', *, *, #17275, .T. ) ;
#14569 = CARTESIAN_POINT ( 'NONE',  ( 69.48867513459482836, 167.7597621252805880, 9.270509831248428867 ) ) ;
#14570 = CARTESIAN_POINT ( 'NONE',  ( 74.72499999726881015, 140.1801316387863778, -4.815267126137194431 ) ) ;
#14571 = CARTESIAN_POINT ( 'NONE',  ( -7.500000000000001776, 0.000000000000000000, 0.000000000000000000 ) ) ;
#14572 =( BOUNDED_CURVE ( )  B_SPLINE_CURVE ( 2, ( #20046, #14756, #28048, #4374, #32360, #4709, #2165, #12548, #32985, #33335, #3749 ),
 .UNSPECIFIED., .F., .T. ) 
 B_SPLINE_CURVE_WITH_KNOTS ( ( 3, 2, 2, 2, 2, 3 ),
 ( 0.2321428571428568455, 0.2357142857142854042, 0.2392857142857139352, 0.2428571428571424939, 0.2464285714285710249, 0.2499999999999996947 ),
 .UNSPECIFIED. ) 
 CURVE ( )  GEOMETRIC_REPRESENTATION_ITEM ( )  RATIONAL_B_SPLINE_CURVE ( ( 1.000000000000003331, 0.9510565162951499785, 1.000000000000000000, 0.9510565162951534202, 1.000000000000000000, 0.9510565162951534202, 1.000000000000000000, 0.9510565162951534202, 1.000000000000000000, 0.9510565162951576390, 0.9999999999999957812 ) ) 
 REPRESENTATION_ITEM ( '' )  );
#14573 = CARTESIAN_POINT ( 'NONE',  ( 6.444103211791042618, 202.2591342207267644, 77.30113791807858092 ) ) ;
#14574 = CARTESIAN_POINT ( 'NONE',  ( 75.38867513459481984, 169.2658477444273331, 4.635254915624208216 ) ) ;
#14575 = AXIS2_PLACEMENT_3D ( 'NONE', #25907, #2410, #23186 ) ;
#14576 = CARTESIAN_POINT ( 'NONE',  ( 40.60000000000000142, 159.7113355953771077, -14.50000000000000888 ) ) ;
#14577 = CARTESIAN_POINT ( 'NONE',  ( 4.903702542908435547, 213.8346818373419751, 54.54886208192144181 ) ) ;
#14578 = EDGE_CURVE ( 'NONE', #10439, #4473, #21316, .T. ) ;
#14579 = EDGE_CURVE ( 'NONE', #10396, #33071, #7765, .T. ) ;
#14580 = CARTESIAN_POINT ( 'NONE',  ( 6.746887896521486461, 3.895317543251989534, -6.526184258131364935 ) ) ;
#14581 = CARTESIAN_POINT ( 'NONE',  ( 78.38867513459481984, 140.7341522555726669, -4.635254915624220651 ) ) ;
#14582 = FACE_OUTER_BOUND ( 'NONE', #32428, .T. ) ;
#14583 = CARTESIAN_POINT ( 'NONE',  ( 52.82499999726880446, 141.7447067706911810, -9.630534252274387086 ) ) ;
#14584 = CARTESIAN_POINT ( 'NONE',  ( 66.57499999726881867, 145.8408176439707802, 12.60653300113718345 ) ) ;
#14585 = CARTESIAN_POINT ( 'NONE',  ( 3.753561863808689836, 218.3979405102790565, 61.40113791807856103 ) ) ;
#14586 = CARTESIAN_POINT ( 'NONE',  ( -125.0000000000000000, -25.00000000000000000, -20.00000000000000000 ) ) ;
#14587 = AXIS2_PLACEMENT_3D ( 'NONE', #8095, #8251, #5518 ) ;
#14588 = EDGE_CURVE ( 'NONE', #26664, #17299, #24039, .T. ) ;
#14589 = PRODUCT_DEFINITION ( 'UNKNOWN', '', #3379, #13851 ) ;
#14590 = CARTESIAN_POINT ( 'NONE',  ( 9.680171189290831535, 199.9079932115568852, 5.301137918078565825 ) ) ;
#14591 = EDGE_CURVE ( 'NONE', #5506, #20133, #16536, .T. ) ;
#14592 = CARTESIAN_POINT ( 'NONE',  ( 3.044812012440130555, 197.4746971517856764, 80.60113791807857808 ) ) ;
#14593 = CIRCLE ( 'NONE', #5357, 1.535500000000000087 ) ;
#14594 = CARTESIAN_POINT ( 'NONE',  ( 3.662846001189864698, 218.4274158808046593, 42.39886208192144323 ) ) ;
#14595 = CARTESIAN_POINT ( 'NONE',  ( -3.135527875058982783, 216.4958274776886924, 45.09886208192143897 ) ) ;
#14596 = CYLINDRICAL_SURFACE ( 'NONE', #8570, 2.000000000000000888 ) ;
#14597 = CARTESIAN_POINT ( 'NONE',  ( 7.375838497908181246, 196.7627149292499666, 89.45113791807857240 ) ) ;
#14598 = CARTESIAN_POINT ( 'NONE',  ( 6.220909254589536808, 215.4770327129947702, 7.551137918078564049 ) ) ;
#14599 = EDGE_CURVE ( 'NONE', #24712, #948, #33171, .T. ) ;
#14600 = CARTESIAN_POINT ( 'NONE',  ( -10.00000000000000711, 206.9523078486584495, 62.49886208192143755 ) ) ;
#14601 = AXIS2_PLACEMENT_3D ( 'NONE', #11531, #24646, #7097 ) ;
#14602 = ORIENTED_EDGE ( 'NONE', *, *, #27889, .F. ) ;
#14603 = CARTESIAN_POINT ( 'NONE',  ( 7.375838497908012492, 217.2372850707501186, 69.54886208192141339 ) ) ;
#14604 = EDGE_LOOP ( 'NONE', ( #26103, #10322, #9330, #12811 ) ) ;
#14605 = CARTESIAN_POINT ( 'NONE',  ( 69.67499999726878457, 168.2552932293087906, -9.630534252274385310 ) ) ;
#14606 = CARTESIAN_POINT ( 'NONE',  ( 0.05014649552828262524, 198.5883022060938572, 46.74886208192144466 ) ) ;
#14607 = ORIENTED_EDGE ( 'NONE', *, *, #17512, .T. ) ;
#14608 = CARTESIAN_POINT ( 'NONE',  ( 80.47499999726881015, 149.9369285172503510, 15.58253174999999580 ) ) ;
#14609 = CARTESIAN_POINT ( 'NONE',  ( 32.50000000000000000, 155.0000000000000000, -6.938893903907228378E-15 ) ) ;
#14610 = DIRECTION ( 'NONE',  ( 0.000000000000000000, 0.000000000000000000, 1.000000000000000000 ) ) ;
#14611 = CARTESIAN_POINT ( 'NONE',  ( -8.000000000000008882, 207.0476921513413515, 63.50113791807856956 ) ) ;
#14612 = DIRECTION ( 'NONE',  ( 0.000000000000000000, 0.000000000000000000, 1.000000000000000000 ) ) ;
#14613 = VECTOR ( 'NONE', #26176, 1000.000000000000000 ) ;
#14614 = CARTESIAN_POINT ( 'NONE',  ( -3.044812012439970683, 197.4746971517856196, 43.89886208192142902 ) ) ;
#14615 = ORIENTED_EDGE ( 'NONE', *, *, #7494, .T. ) ;
#14616 = CARTESIAN_POINT ( 'NONE',  ( 64.50000000000000000, -103.0000000000000000, 30.00000000000000000 ) ) ;
#14617 = CIRCLE ( 'NONE', #30955, 12.00000000000000355 ) ;
#14618 = CARTESIAN_POINT ( 'NONE',  ( -31.74999999999995737, 4.898587196589413815E-16, -4.000000000000000888 ) ) ;
#14619 = DIRECTION ( 'NONE',  ( -0.000000000000000000, -0.000000000000000000, 1.000000000000000000 ) ) ;
#14620 = CARTESIAN_POINT ( 'NONE',  ( 7.984503880673422316, 209.6470497212048372, 24.84886208192143897 ) ) ;
#14621 = CARTESIAN_POINT ( 'NONE',  ( 6.139770520408368348, 198.4640165459539674, 65.45113791807857240 ) ) ;
#14622 = CARTESIAN_POINT ( 'NONE',  ( 8.062137200540920645, 201.0835637161417822, 50.30113791807857382 ) ) ;
#14623 = CARTESIAN_POINT ( 'NONE',  ( 38.01132485994281041, 167.7597621252805880, -9.270509831248443078 ) ) ;
#14624 = CONTEXT_DEPENDENT_SHAPE_REPRESENTATION ( #33162, #20955 ) ;
#14625 = CARTESIAN_POINT ( 'NONE',  ( 6.220909254589536808, 215.4770327129947702, 13.55113791807856849 ) ) ;
#14626 = CARTESIAN_POINT ( 'NONE',  ( 2.426778023690261410, 199.3768101843759837, 8.601137918078565647 ) ) ;
#14627 = CARTESIAN_POINT ( 'NONE',  ( 43.12499999726881583, 155.0000000000000000, -15.58253175000000823 ) ) ;
#14628 = CARTESIAN_POINT ( 'NONE',  ( -3.250000000000004441, 5.629165124598849879, 0.000000000000000000 ) ) ;
#14629 = CARTESIAN_POINT ( 'NONE',  ( 34.52499999726880731, 140.1801316387863778, 4.815267126137185549 ) ) ;
#14630 = CARTESIAN_POINT ( 'NONE',  ( -3.662846001190052991, 218.4274158808045740, 28.10113791807856742 ) ) ;
#14631 = CYLINDRICAL_SURFACE ( 'NONE', #26018, 13.50000000000001066 ) ;
#14632 = CARTESIAN_POINT ( 'NONE',  ( 3.135527875058820690, 216.4958274776887492, 73.40113791807857524 ) ) ;
#14633 = CARTESIAN_POINT ( 'NONE',  ( -10.00000000000000711, 207.0476921513413515, 45.50113791807857666 ) ) ;
#14634 = FACE_OUTER_BOUND ( 'NONE', #2563, .T. ) ;
#14635 = DIRECTION ( 'NONE',  ( 0.000000000000000000, 1.000000000000000000, -1.224646799147353207E-16 ) ) ;
#14636 = CARTESIAN_POINT ( 'NONE',  ( -3.753561863808878130, 218.3979405102790281, 18.09886208192143187 ) ) ;
#14637 = CARTESIAN_POINT ( 'NONE',  ( -3.135527875058982783, 216.4958274776886924, 21.09886208192143897 ) ) ;
#14638 = CARTESIAN_POINT ( 'NONE',  ( 64.39999999453763735, 168.7903194862797420, -4.480746418436745593 ) ) ;
#14639 = ORIENTED_EDGE ( 'NONE', *, *, #4607, .F. ) ;
#14640 = CARTESIAN_POINT ( 'NONE',  ( -7.375838497908182134, 217.2372850707499765, 60.95113791807857240 ) ) ;
#14641 = AXIS2_PLACEMENT_3D ( 'NONE', #13174, #7225, #22894 ) ;
#14642 = CARTESIAN_POINT ( 'NONE',  ( -0.05014649552807731031, 198.5883022060938572, 68.75113791807856956 ) ) ;
#14643 = CARTESIAN_POINT ( 'NONE',  ( 0.05014649552828275708, 196.4853777576173002, 28.74886208192144110 ) ) ;
#14644 = CARTESIAN_POINT ( 'NONE',  ( 76.61132485994281183, 159.8737954434937478, 14.99999999999991651 ) ) ;
#14645 = EDGE_LOOP ( 'NONE', ( #2698, #25469, #24037, #14505, #26092, #4858 ) ) ;
#14646 = ORIENTED_EDGE ( 'NONE', *, *, #20300, .F. ) ;
#14647 = CARTESIAN_POINT ( 'NONE',  ( 10.00000000000000711, 206.9523078486586201, 92.00113791807858377 ) ) ;
#14648 = ORIENTED_EDGE ( 'NONE', *, *, #2945, .T. ) ;
#14649 = CARTESIAN_POINT ( 'NONE',  ( -3.956728429394472002, 206.4109532238489351, -6.000000000000015099 ) ) ;
#14650 = DIRECTION ( 'NONE',  ( 0.000000000000000000, 0.000000000000000000, 1.000000000000000000 ) ) ;
#14651 = ORIENTED_EDGE ( 'NONE', *, *, #31606, .T. ) ;
#14652 = CARTESIAN_POINT ( 'NONE',  ( 6.500168698208129925, 211.6636982574063381, 34.70113791807857240 ) ) ;
#14653 = DIRECTION ( 'NONE',  ( -0.000000000000000000, -0.000000000000000000, 1.000000000000000000 ) ) ;
#14654 = CARTESIAN_POINT ( 'NONE',  ( -6.220909254589682469, 215.4770327129946850, 14.94886208192143151 ) ) ;
#14655 = CARTESIAN_POINT ( 'NONE',  ( 58.87499999726880873, 138.6155565068815747, -3.929120461958505118E-15 ) ) ;
#14656 = EDGE_LOOP ( 'NONE', ( #15201, #11633, #19223, #9201 ) ) ;
#14657 = CARTESIAN_POINT ( 'NONE',  ( 0.05014649552807626948, 215.4116977939061144, 46.25113791807857666 ) ) ;
#14658 = FACE_OUTER_BOUND ( 'NONE', #15498, .T. ) ;
#14659 = CARTESIAN_POINT ( 'NONE',  ( 10.00000000000000178, 0.000000000000000000, 0.000000000000000000 ) ) ;
#14660 = TOROIDAL_SURFACE ( 'NONE', #15756, 4.999999999999990230, 2.500000000000000000 ) ;
#14661 = CARTESIAN_POINT ( 'NONE',  ( 6.139770520408223575, 215.5359834540460611, 99.54886208192144181 ) ) ;
#14662 = CARTESIAN_POINT ( 'NONE',  ( 65.57499999726881867, 164.1591823560292198, -12.60653300113719766 ) ) ;
#14663 = CARTESIAN_POINT ( 'NONE',  ( -8.062137200540920645, 212.9164362838581894, 27.80113791807856671 ) ) ;
#14664 = SURFACE_SIDE_STYLE ('',( #4271 ) ) ;
#14665 = CARTESIAN_POINT ( 'NONE',  ( 8.118202686958039038, 212.8392687619912635, 16.70113791807856529 ) ) ;
#14666 = DIRECTION ( 'NONE',  ( 0.000000000000000000, 0.7071067811865536790, 0.7071067811865413555 ) ) ;
#14667 = CARTESIAN_POINT ( 'NONE',  ( 81.00000000000001421, 170.2462022514548323, -7.872454543227099337E-15 ) ) ;
#14668 = CARTESIAN_POINT ( 'NONE',  ( -56.08018104464575515, 194.9950560901275480, -0.6488614982153378952 ) ) ;
#14669 = DIRECTION ( 'NONE',  ( 1.000000000000000000, -0.000000000000000000, -0.000000000000000000 ) ) ;
#14670 = CARTESIAN_POINT ( 'NONE',  ( -11.98450388067348804, 210.9467285061362247, 3.651137918078566358 ) ) ;
#14671 = CARTESIAN_POINT ( 'NONE',  ( 5.000000000000000000, -2.342598717236903383, 4.057500000000001883 ) ) ;
#14672 = CARTESIAN_POINT ( 'NONE',  ( 42.77499999726880731, 140.1801316387863778, 4.815267126137185549 ) ) ;
#14673 = CARTESIAN_POINT ( 'NONE',  ( 3.044812012440130555, 197.4746971517856764, 47.60113791807857098 ) ) ;
#14674 = CARTESIAN_POINT ( 'NONE',  ( 80.62499999726880162, 138.6155565068815463, -3.929120461958505118E-15 ) ) ;
#14675 = DIRECTION ( 'NONE',  ( -1.000000000000000000, -0.000000000000000000, -0.000000000000000000 ) ) ;
#14676 = CYLINDRICAL_SURFACE ( 'NONE', #11371, 2.000000000000000888 ) ;
#14677 = CARTESIAN_POINT ( 'NONE',  ( 44.99999999453763166, 155.0000000000000000, 14.49999999999999467 ) ) ;
#14678 = EDGE_LOOP ( 'NONE', ( #27216, #24799, #6219, #6392 ) ) ;
#14679 = CARTESIAN_POINT ( 'NONE',  ( -3.662846001190052991, 218.4274158808045740, 28.10113791807856742 ) ) ;
#14680 = FACE_OUTER_BOUND ( 'NONE', #14645, .T. ) ;
#14681 = B_SPLINE_CURVE_WITH_KNOTS ( 'NONE', 3,
 ( #21838, #16228, #11133, #31572, #3614, #8237, #18959, #26452, #11460 ),
 .UNSPECIFIED., .F., .F.,
 ( 4, 2, 1, 2, 4 ),
 ( 6.245710625686469831E-20, 0.002165063509461098365, 0.004330127018922195863, 0.006495190528383293360, 0.008660254037844389990 ),
 .UNSPECIFIED. ) ;
#14682 = EDGE_CURVE ( 'NONE', #14133, #25683, #22601, .T. ) ;
#14683 = CARTESIAN_POINT ( 'NONE',  ( 66.61132485994281183, 159.8737954434938615, 14.99999999999982592 ) ) ;
#14684 = ORIENTED_EDGE ( 'NONE', *, *, #12524, .F. ) ;
#14685 = CARTESIAN_POINT ( 'NONE',  ( 6.220909254589536808, 215.4770327129947702, 1.551137918078565825 ) ) ;
#14686 = CARTESIAN_POINT ( 'NONE',  ( -0.05014649552810635652, 196.4853777576173002, 56.75113791807855534 ) ) ;
#14687 = CARTESIAN_POINT ( 'NONE',  ( 4.903702542908435547, 213.8346818373419751, 18.54886208192143116 ) ) ;
#14688 = DIRECTION ( 'NONE',  ( 0.000000000000000000, 0.000000000000000000, 1.000000000000000000 ) ) ;
#14689 = ORIENTED_EDGE ( 'NONE', *, *, #12085, .T. ) ;
#14690 = CARTESIAN_POINT ( 'NONE',  ( -8.015496119326531499, 204.4483345814780364, 0.3511379180785659249 ) ) ;
#14691 = DIRECTION ( 'NONE',  ( 1.000000000000000000, -0.000000000000000000, -0.000000000000000000 ) ) ;
#14692 = CARTESIAN_POINT ( 'NONE',  ( -12.01549611932659722, 210.8513442034533227, 89.64886208192142192 ) ) ;
#14693 = CARTESIAN_POINT ( 'NONE',  ( 34.27499999726880731, 160.0630714827496206, 15.58253174999999224 ) ) ;
#14694 = ORIENTED_EDGE ( 'NONE', *, *, #13689, .T. ) ;
#14695 = CARTESIAN_POINT ( 'NONE',  ( 42.42499999726881299, 141.7447067706911810, 9.630534252274376428 ) ) ;
#14696 = LINE ( 'NONE', #9253, #3902 ) ;
#14697 = CARTESIAN_POINT ( 'NONE',  ( 54.71132485994280614, 155.0000000000000000, 15.00000000000001243 ) ) ;
#14698 = CARTESIAN_POINT ( 'NONE',  ( -3.044812012439970683, 197.4746971517856196, 70.89886208192143613 ) ) ;
#14699 = CARTESIAN_POINT ( 'NONE',  ( 40.87499999726880873, 138.6155565068815463, -3.929120461958505118E-15 ) ) ;
#14700 = DIRECTION ( 'NONE',  ( 1.000000000000000000, 0.000000000000000000, 0.000000000000000000 ) ) ;
#14701 = CARTESIAN_POINT ( 'NONE',  ( -8.118202686958039038, 201.1607312380087080, 6.201137918078566180 ) ) ;
#14702 = CARTESIAN_POINT ( 'NONE',  ( -3.500000000000001332, 2.020725942163676070, -0.3126073911696459207 ) ) ;
#14703 = CARTESIAN_POINT ( 'NONE',  ( 62.10000000000000142, 141.2096805137202580, -4.480746418436742040 ) ) ;
#14704 = CARTESIAN_POINT ( 'NONE',  ( 63.71132485994279904, 155.0000000000000000, -15.00000000000002487 ) ) ;
#14705 = CARTESIAN_POINT ( 'NONE',  ( -4.984841277089891776, 213.7757310962905990, 86.94886208192144750 ) ) ;
#14706 = FACE_OUTER_BOUND ( 'NONE', #1958, .T. ) ;
#14707 = CARTESIAN_POINT ( 'NONE',  ( 0.000000000000000000, 0.000000000000000000, -8.000000000000000000 ) ) ;
#14708 = CARTESIAN_POINT ( 'NONE',  ( 9.736236675708031640, 199.9851607334238963, 88.29886208192142760 ) ) ;
#14709 = CARTESIAN_POINT ( 'NONE',  ( 63.72499999726881015, 169.8198683612136222, 4.815267126137181997 ) ) ;
#14711 = EDGE_LOOP ( 'NONE', ( #25632, #32836, #25712 ) ) ;
#14710 = CARTESIAN_POINT ( 'NONE',  ( -8.062137200540920645, 212.9164362838581894, 15.80113791807856849 ) ) ;
#14712 = DIRECTION ( 'NONE',  ( 0.000000000000000000, -0.04769215134144316748, 0.9988620819214356628 ) ) ;
#14713 = CARTESIAN_POINT ( 'NONE',  ( 83.07499999726880446, 141.7447067706911810, -9.630534252274385310 ) ) ;
#14714 = CARTESIAN_POINT ( 'NONE',  ( 7.456977232089302632, 217.1783343296989131, 85.55113791807858092 ) ) ;
#14715 = CARTESIAN_POINT ( 'NONE',  ( -10.07879766094112384, 205.9536517436126530, 104.4468559609856158 ) ) ;
#14716 = EDGE_CURVE ( 'NONE', #22749, #14059, #3925, .T. ) ;
#14717 = ORIENTED_EDGE ( 'NONE', *, *, #19154, .F. ) ;
#14718 = CARTESIAN_POINT ( 'NONE',  ( -3.753561863808878130, 218.3979405102790281, 72.09886208192142476 ) ) ;
#14719 = CARTESIAN_POINT ( 'NONE',  ( 6.139770520408223575, 215.5359834540460611, 78.54886208192144181 ) ) ;
#14720 = AXIS2_PLACEMENT_3D ( 'NONE', #15506, #2566, #23350 ) ;
#14721 = CARTESIAN_POINT ( 'NONE',  ( -11.98450388067341876, 203.0532714938636047, 11.34886208192143542 ) ) ;
#14722 = PLANE ( 'NONE',  #7229 ) ;
#14723 = CARTESIAN_POINT ( 'NONE',  ( -0.05014649552810635652, 196.4853777576173002, 35.75113791807857666 ) ) ;
#14724 = LINE ( 'NONE', #22568, #30859 ) ;
#14725 = CARTESIAN_POINT ( 'NONE',  ( 6.139770520408223575, 215.5359834540460611, 99.54886208192144181 ) ) ;
#14726 = EDGE_CURVE ( 'NONE', #895, #615, #152, .T. ) ;
#14727 = DIRECTION ( 'NONE',  ( 1.000000000000000000, 0.000000000000000000, 0.000000000000000000 ) ) ;
#14728 = VERTEX_POINT ( 'NONE', #21907 ) ;
#14729 = CARTESIAN_POINT ( 'NONE',  ( -2.249320974685042440, -30.45561873520117757, -16.29357272760981701 ) ) ;
#14730 = CARTESIAN_POINT ( 'NONE',  ( -8.000000000000008882, 206.9523078486584780, 77.49886208192144466 ) ) ;
#14731 = VERTEX_POINT ( 'NONE', #16797 ) ;
#14732 = CARTESIAN_POINT ( 'NONE',  ( 84.52499999726880731, 140.1801316387863778, 4.815267126137185549 ) ) ;
#14733 = ORIENTED_EDGE ( 'NONE', *, *, #18880, .T. ) ;
#14734 = DIRECTION ( 'NONE',  ( 1.000000000000000000, 0.000000000000000000, 0.000000000000000000 ) ) ;
#14735 = CARTESIAN_POINT ( 'NONE',  ( 75.82499999726881867, 168.2552932293087906, 9.630534252274372875 ) ) ;
#14736 = ADVANCED_FACE ( 'NONE', ( #18852 ), #31798, .F. ) ;
#14737 = DIRECTION ( 'NONE',  ( 1.000000000000000000, 0.000000000000000000, 0.000000000000000000 ) ) ;
#14738 = CARTESIAN_POINT ( 'NONE',  ( -6.444103211791042618, 211.7408657792732356, 81.80113791807858092 ) ) ;
#14739 = CARTESIAN_POINT ( 'NONE',  ( 87.50000000000004263, 170.2753832955869484, 1.322035671867324513 ) ) ;
#14740 = CARTESIAN_POINT ( 'NONE',  ( 42.00000000000000000, 139.7537977485451393, -4.138211985947621020E-15 ) ) ;
#14741 = CARTESIAN_POINT ( 'NONE',  ( -6.500168698208244500, 211.6636982574061676, 50.79886208192144892 ) ) ;
#14742 = EDGE_CURVE ( 'NONE', #10143, #16190, #1766, .T. ) ;
#14743 = DIRECTION ( 'NONE',  ( -1.000000000000000000, 0.000000000000000000, -0.000000000000000000 ) ) ;
#14744 = CARTESIAN_POINT ( 'NONE',  ( 78.08867513459483689, 142.2402378747194405, 9.270509831248432420 ) ) ;
#14745 = CARTESIAN_POINT ( 'NONE',  ( 2.000000000000000000, -0.8865213383406685965, 1.535500000000000531 ) ) ;
#14746 = CARTESIAN_POINT ( 'NONE',  ( 52.52499999726881441, 140.1801316387863778, 4.815267126137185549 ) ) ;
#14747 = CARTESIAN_POINT ( 'NONE',  ( 62.57499999726881867, 145.8408176439707802, 12.60653300113718345 ) ) ;
#14748 = CARTESIAN_POINT ( 'NONE',  ( 3.662846001190051659, 195.5725841191953691, 62.60113791807857808 ) ) ;
#14749 = DIRECTION ( 'NONE',  ( 0.000000000000000000, 0.000000000000000000, -1.000000000000000000 ) ) ;
#14750 = CARTESIAN_POINT ( 'NONE',  ( 3.662846001190051659, 195.5725841191953691, -0.3988620819214345747 ) ) ;
#14751 = CARTESIAN_POINT ( 'NONE',  ( -9.984503880673475606, 210.2968891136704315, 81.65113791807857524 ) ) ;
#14752 = CARTESIAN_POINT ( 'NONE',  ( -3.662846001189865142, 195.5725841191952838, 43.89886208192143613 ) ) ;
#14753 = CARTESIAN_POINT ( 'NONE',  ( -8.062137200540822946, 201.0835637161416400, 47.19886208192143329 ) ) ;
#14754 = LINE ( 'NONE', #4543, #17195 ) ;
#14755 = CARTESIAN_POINT ( 'NONE',  ( -12.00000000000000711, 207.0476921513413515, 87.50113791807856956 ) ) ;
#14756 = CARTESIAN_POINT ( 'NONE',  ( 74.68867513459483121, 150.1262045565067069, -15.00000000000023981 ) ) ;
#14757 = CARTESIAN_POINT ( 'NONE',  ( 9.984503880673470277, 203.7031108863295401, 5.151137918078567246 ) ) ;
#14758 = CARTESIAN_POINT ( 'NONE',  ( -9.984503880673420539, 203.7031108863293980, 74.34886208192143897 ) ) ;
#14759 = DIRECTION ( 'NONE',  ( 4.625929269271485914E-16, -1.000000000000000000, 0.000000000000000000 ) ) ;
#14760 = ORIENTED_EDGE ( 'NONE', *, *, #13490, .F. ) ;
#14761 = CARTESIAN_POINT ( 'NONE',  ( 3.753561863808876797, 195.6020594897209719, 73.59886208192142476 ) ) ;
#14762 = VECTOR ( 'NONE', #6710, 1000.000000000000000 ) ;
#14763 = ORIENTED_EDGE ( 'NONE', *, *, #3681, .F. ) ;
#14764 = CARTESIAN_POINT ( 'NONE',  ( 78.67499999726879878, 141.7447067706911810, 9.630534252274376428 ) ) ;
#14765 = CARTESIAN_POINT ( 'NONE',  ( 6.500168698208244500, 202.3363017425938324, 40.29886208192144181 ) ) ;
#14766 = ORIENTED_EDGE ( 'NONE', *, *, #26879, .F. ) ;
#14767 =( BOUNDED_CURVE ( )  B_SPLINE_CURVE ( 2, ( #26364, #11193, #6066, #475, #13911, #18535, #31964, #28917, #3518, #10872, #13248 ),
 .UNSPECIFIED., .F., .T. ) 
 B_SPLINE_CURVE_WITH_KNOTS ( ( 3, 2, 2, 2, 2, 3 ),
 ( 0.4821428571428570398, 0.4857142857142855985, 0.4892857142857141572, 0.4928571428571427715, 0.4964285714285713302, 0.4999999999999998890 ),
 .UNSPECIFIED. ) 
 CURVE ( )  GEOMETRIC_REPRESENTATION_ITEM ( )  RATIONAL_B_SPLINE_CURVE ( ( 1.000000000000000666, 0.9510565162951526430, 1.000000000000000000, 0.9510565162951534202, 1.000000000000000000, 0.9510565162951534202, 1.000000000000000000, 0.9510565162951534202, 1.000000000000000000, 0.9510565162951541973, 0.9999999999999992228 ) ) 
 REPRESENTATION_ITEM ( '' )  );
#14768 = ADVANCED_FACE ( 'NONE', ( #8966 ), #673, .T. ) ;
#14769 = EDGE_CURVE ( 'NONE', #27125, #31583, #16979, .T. ) ;
#14770 = CARTESIAN_POINT ( 'NONE',  ( 83.47499999726881015, 160.0630714827496206, -15.58253175000000823 ) ) ;
#14771 = CARTESIAN_POINT ( 'NONE',  ( 56.71132485994280614, 155.0000000000000000, 15.00000000000001243 ) ) ;
#14772 = DIRECTION ( 'NONE',  ( 1.000000000000000000, 0.000000000000000000, 0.000000000000000000 ) ) ;
#14773 = CARTESIAN_POINT ( 'NONE',  ( 59.62499999726882294, 171.3844434931184253, -7.942151717890132712E-15 ) ) ;
#14774 = ADVANCED_FACE ( 'NONE', ( #3346 ), #126, .T. ) ;
#14775 = DIRECTION ( 'NONE',  ( 1.000000000000000000, 0.000000000000000000, 0.000000000000000000 ) ) ;
#14776 = CARTESIAN_POINT ( 'NONE',  ( -8.062137200540822946, 201.0835637161416400, 38.19886208192143329 ) ) ;
#14777 = VERTEX_POINT ( 'NONE', #472 ) ;
#14778 = DIRECTION ( 'NONE',  ( 0.000000000000000000, 0.000000000000000000, -1.000000000000000000 ) ) ;
#14779 = CARTESIAN_POINT ( 'NONE',  ( 4.424031367840750129, -4.951337798339555007, -6.056431503347240231 ) ) ;
#14780 = CARTESIAN_POINT ( 'NONE',  ( 85.91132485994280898, 163.8167787843871110, -12.13525491562423397 ) ) ;
#14781 = CARTESIAN_POINT ( 'NONE',  ( 8.015496119326595448, 204.4483345814782638, 28.14886208192143968 ) ) ;
#14782 = ADVANCED_FACE ( 'NONE', ( #19356, #29248, #11361, #23968, #29085 ), #32131, .T. ) ;
#14783 = CARTESIAN_POINT ( 'NONE',  ( -8.118202686958039038, 201.1607312380087080, 63.20113791807857240 ) ) ;
#14784 = CARTESIAN_POINT ( 'NONE',  ( 0.05014649552810505201, 217.5146222423826714, 46.25113791807855534 ) ) ;
#14785 = CONTEXT_DEPENDENT_SHAPE_REPRESENTATION ( #25750, #3278 ) ;
#14786 = CARTESIAN_POINT ( 'NONE',  ( -3.135527875058821579, 197.5041725223112223, 17.90113791807856458 ) ) ;
#14787 = CARTESIAN_POINT ( 'NONE',  ( -2.517493886308901807, 199.4062855549015012, 5.901137918078568134 ) ) ;
#14788 = CARTESIAN_POINT ( 'NONE',  ( 47.42499999726879878, 168.2552932293087906, -9.630534252274385310 ) ) ;
#14789 = CARTESIAN_POINT ( 'NONE',  ( 1.452965002680449924, -3.202582148906760739, -2.899999999999980815 ) ) ;
#14790 = CARTESIAN_POINT ( 'NONE',  ( 33.62499999726880873, 171.3844434931184253, -7.942151717890134290E-15 ) ) ;
#14791 = CARTESIAN_POINT ( 'NONE',  ( -3.753561863808691168, 195.6020594897209435, 32.90113791807856813 ) ) ;
#14792 = DIRECTION ( 'NONE',  ( 0.000000000000000000, 0.000000000000000000, -1.000000000000000000 ) ) ;
#14793 = CARTESIAN_POINT ( 'NONE',  ( -3.135527875058821579, 197.5041725223112223, 71.90113791807857524 ) ) ;
#14794 = CARTESIAN_POINT ( 'NONE',  ( 10.01549611932653860, 210.2015048109876716, 52.85113791807856387 ) ) ;
#14795 = UNCERTAINTY_MEASURE_WITH_UNIT (LENGTH_MEASURE( 1.000000000000000082E-05 ), #17725, 'distance_accuracy_value', 'NONE');
#14796 = CARTESIAN_POINT ( 'NONE',  ( 5.040301471719072168, 5.750234626350511746, -0.09933465333851003443 ) ) ;
#14797 = CARTESIAN_POINT ( 'NONE',  ( 54.08867513459482979, 142.2402378747194405, 9.270509831248432420 ) ) ;
#14798 = CARTESIAN_POINT ( 'NONE',  ( -12.00000000000000711, 206.9523078486584780, 14.49886208192143577 ) ) ;
#14799 = CARTESIAN_POINT ( 'NONE',  ( -3.044812012439970683, 197.4746971517856196, 19.89886208192143613 ) ) ;
#14800 = CARTESIAN_POINT ( 'NONE',  ( 71.09999999453761177, 150.2886644046228639, 14.49999999999999645 ) ) ;
#14801 = AXIS2_PLACEMENT_3D ( 'NONE', #26685, #14075, #32303 ) ;
#14802 = ORIENTED_EDGE ( 'NONE', *, *, #7261, .F. ) ;
#14803 = CARTESIAN_POINT ( 'NONE',  ( 3.662846001190051659, 195.5725841191953691, 62.60113791807857808 ) ) ;
#14804 = CARTESIAN_POINT ( 'NONE',  ( 6.444103211791042618, 202.2591342207267644, 80.30113791807858092 ) ) ;
#14805 = CARTESIAN_POINT ( 'NONE',  ( 6.139770520408223575, 215.5359834540460611, 30.54886208192142760 ) ) ;
#14806 =( NAMED_UNIT ( * ) SI_UNIT ( $, .STERADIAN. ) SOLID_ANGLE_UNIT ( ) );
#14807 = ORIENTED_EDGE ( 'NONE', *, *, #8459, .F. ) ;
#14808 = VERTEX_POINT ( 'NONE', #5900 ) ;
#14809 = EDGE_LOOP ( 'NONE', ( #26267, #17366, #29347, #31334 ) ) ;
#14810 = ADVANCED_FACE ( 'NONE', ( #16294 ), #30052, .T. ) ;
#14811 = CARTESIAN_POINT ( 'NONE',  ( 57.78867513459481842, 155.0000000000000000, 15.00000000000001243 ) ) ;
#14812 = AXIS2_PLACEMENT_3D ( 'NONE', #4101, #14491, #1551 ) ;
#14813 = PLANE ( 'NONE',  #19798 ) ;
#14814 = ORIENTED_EDGE ( 'NONE', *, *, #20351, .T. ) ;
#14815 = CARTESIAN_POINT ( 'NONE',  ( 4.984841277089725686, 213.7757310962907411, 31.55113791807857382 ) ) ;
#14816 = DIRECTION ( 'NONE',  ( 1.000000000000000000, -0.000000000000000000, -0.000000000000000000 ) ) ;
#14817 = CARTESIAN_POINT ( 'NONE',  ( 0.05014649552828275708, 196.4853777576173002, 13.74886208192143400 ) ) ;
#14818 = CARTESIAN_POINT ( 'NONE',  ( 54.97499999726881015, 140.1801316387863778, -4.815267126137194431 ) ) ;
#14819 = EDGE_LOOP ( 'NONE', ( #13716, #5264, #30491, #6563 ) ) ;
#14820 = CARTESIAN_POINT ( 'NONE',  ( -4.903702542908602524, 213.8346818373418898, 48.95113791807857240 ) ) ;
#14821 = LINE ( 'NONE', #19934, #11819 ) ;
#14822 = AXIS2_PLACEMENT_3D ( 'NONE', #29586, #8464, #23800 ) ;
#14823 = DIRECTION ( 'NONE',  ( -0.000000000000000000, -0.000000000000000000, 1.000000000000000000 ) ) ;
#14824 = CARTESIAN_POINT ( 'NONE',  ( -10.01549611932659722, 210.2015048109875011, 101.6488620819214361 ) ) ;
#14825 = AXIS2_PLACEMENT_3D ( 'NONE', #32440, #6040, #16431 ) ;
#14826 = CARTESIAN_POINT ( 'NONE',  ( 65.27499999726880731, 149.9369285172503510, -15.58253175000000823 ) ) ;
#14827 = CARTESIAN_POINT ( 'NONE',  ( 8.118202686958039038, 212.8392687619912635, 31.70113791807856884 ) ) ;
#14828 = CARTESIAN_POINT ( 'NONE',  ( 70.58867513459482268, 146.1832212156128890, -12.13525491562423042 ) ) ;
#14829 = CARTESIAN_POINT ( 'NONE',  ( -9.984503880673473830, 210.2968891136704315, 21.65113791807856458 ) ) ;
#14830 = DIRECTION ( 'NONE',  ( 1.000000000000000000, 0.000000000000000000, 0.000000000000000000 ) ) ;
#14831 = CARTESIAN_POINT ( 'NONE',  ( 81.50000000000000000, 155.0000000000000000, 14.49999999999999467 ) ) ;
#14832 = CARTESIAN_POINT ( 'NONE',  ( -56.25248981486732447, 194.9849645003486387, 1.107065583161625621 ) ) ;
#14833 = DIRECTION ( 'NONE',  ( 1.000000000000000000, 0.000000000000000000, 0.000000000000000000 ) ) ;
#14834 = CARTESIAN_POINT ( 'NONE',  ( -12.00000000000000711, 207.0476921513413515, 3.501137918078566003 ) ) ;
#14835 = CARTESIAN_POINT ( 'NONE',  ( 7.331804101520335523E-16, -31.75426480542945740, -18.00000000000000000 ) ) ;
#14836 = CARTESIAN_POINT ( 'NONE',  ( 49.87499999726880162, 171.3844434931184253, -7.942151717890132712E-15 ) ) ;
#14837 = CARTESIAN_POINT ( 'NONE',  ( 6.220909254589536808, 215.4770327129947702, 43.55113791807857382 ) ) ;
#14838 = CARTESIAN_POINT ( 'NONE',  ( 80.92499999726882720, 145.8408176439707802, -12.60653300113719588 ) ) ;
#14839 = VECTOR ( 'NONE', #5952, 1000.000000000000000 ) ;
#14840 = CARTESIAN_POINT ( 'NONE',  ( -65.20000000000000284, -0.9203920079924744480, -19.30000000000004690 ) ) ;
#14841 = CARTESIAN_POINT ( 'NONE',  ( 4.000000000000000000, 0.000000000000000000, 0.000000000000000000 ) ) ;
#14842 = CARTESIAN_POINT ( 'NONE',  ( 53.09999999453761887, 150.2886644046228639, 14.49999999999999645 ) ) ;
#14843 = ORIENTED_EDGE ( 'NONE', *, *, #28282, .T. ) ;
#14844 = CARTESIAN_POINT ( 'NONE',  ( -7.375838497908182134, 217.2372850707499765, 30.95113791807857595 ) ) ;
#14845 = CARTESIAN_POINT ( 'NONE',  ( 61.51132485994280330, 146.1832212156128890, -12.13525491562423042 ) ) ;
#14846 = CARTESIAN_POINT ( 'NONE',  ( 3.135527875058981895, 197.5041725223112792, 1.598862081921434530 ) ) ;
#14847 = APPLICATION_CONTEXT ( 'automotive_design' ) ;
#14848 = CARTESIAN_POINT ( 'NONE',  ( 7.500000000000000000, 4.330127018922190096, -10.00000000000000000 ) ) ;
#14849 = VERTEX_POINT ( 'NONE', #631 ) ;
#14850 = AXIS2_PLACEMENT_3D ( 'NONE', #12535, #31442, #28210 ) ;
#14851 = CARTESIAN_POINT ( 'NONE',  ( 8.062137200540920645, 201.0835637161417822, -0.6988620819214342861 ) ) ;
#14852 = CARTESIAN_POINT ( 'NONE',  ( -6.220909254589537696, 198.5229672870051161, 66.05113791807858092 ) ) ;
#14853 = ORIENTED_EDGE ( 'NONE', *, *, #21057, .F. ) ;
#14854 = CARTESIAN_POINT ( 'NONE',  ( -4.903702542908436435, 200.1653181626580249, 20.04886208192143471 ) ) ;
#14855 = AXIS2_PLACEMENT_3D ( 'NONE', #5722, #29869, #24921 ) ;
#14856 = CARTESIAN_POINT ( 'NONE',  ( 125.5000000000000000, 78.52640161467446944, -73.43303922622258995 ) ) ;
#14857 = ORIENTED_EDGE ( 'NONE', *, *, #15294, .F. ) ;
#14858 = CARTESIAN_POINT ( 'NONE',  ( 2.517493886308900919, 214.5937144450984420, 1.401137918078566136 ) ) ;
#14859 = LINE ( 'NONE', #25255, #3985 ) ;
#14860 = CARTESIAN_POINT ( 'NONE',  ( 7.375838497908012492, 217.2372850707501186, 84.54886208192144181 ) ) ;
#14861 = CARTESIAN_POINT ( 'NONE',  ( 37.37499999726881583, 155.0000000000000000, -15.58253175000000823 ) ) ;
#14862 = VERTEX_POINT ( 'NONE', #19025 ) ;
#14863 = CARTESIAN_POINT ( 'NONE',  ( 44.42499999726881299, 141.7447067706911810, 9.630534252274376428 ) ) ;
#14864 = DIRECTION ( 'NONE',  ( 0.000000000000000000, 0.000000000000000000, 1.000000000000000000 ) ) ;
#14865 = CARTESIAN_POINT ( 'NONE',  ( 54.61132485994280472, 159.8737954434937478, 14.99999999999991651 ) ) ;
#14866 = CARTESIAN_POINT ( 'NONE',  ( 10.01549611932659545, 203.7984951890123853, 70.14886208192139350 ) ) ;
#14867 = CARTESIAN_POINT ( 'NONE',  ( 46.17499999726881299, 164.1591823560292198, 12.60653300113718167 ) ) ;
#14868 = CARTESIAN_POINT ( 'NONE',  ( 10.39117206796836257, 0.000000000000000000, -8.499999999999998224 ) ) ;
#14869 = CARTESIAN_POINT ( 'NONE',  ( 8.062137200540920645, 201.0835637161417822, -0.6988620819214342861 ) ) ;
#14870 = PRODUCT ( 'socket head cap screw_iso_ISO 4762 M4 x 12 - 12N', 'socket head cap screw_iso_ISO 4762 M4 x 12 - 12N', '', ( #10581 ) ) ;
#14871 = DIRECTION ( 'NONE',  ( 0.000000000000000000, -1.000000000000000000, 0.000000000000000000 ) ) ;
#14872 = ADVANCED_FACE ( 'NONE', ( #6414 ), #29413, .F. ) ;
#14873 = CIRCLE ( 'NONE', #9977, 2.149999999999979483 ) ;
#14874 = CARTESIAN_POINT ( 'NONE',  ( 62.79999999999999716, 167.3344367211045096, -8.961492836873482304 ) ) ;
#14875 = CARTESIAN_POINT ( 'NONE',  ( 3.044812012440130555, 197.4746971517856764, 92.60113791807857808 ) ) ;
#14876 = CARTESIAN_POINT ( 'NONE',  ( 60.00000000000000000, 7.347880794884118356E-15, -20.00000000000000355 ) ) ;
#14877 = CARTESIAN_POINT ( 'NONE',  ( 3.044812012440130555, 197.4746971517856764, 74.60113791807856387 ) ) ;
#14878 = CARTESIAN_POINT ( 'NONE',  ( -6.486836893983275232, 4.915077010913945443, -7.231838333420560261 ) ) ;
#14879 = TOROIDAL_SURFACE ( 'NONE', #31214, 4.999999999999990230, 2.500000000000000000 ) ;
#14880 = DIRECTION ( 'NONE',  ( -0.1461455375466716444, 0.9854922318508084755, -0.08629335326029916042 ) ) ;
#14881 = CARTESIAN_POINT ( 'NONE',  ( 9.680171189290716072, 214.0920067884432854, 90.69886208192143329 ) ) ;
#14882 = AXIS2_PLACEMENT_3D ( 'NONE', #5300, #30524, #12467 ) ;
#14883 = CARTESIAN_POINT ( 'NONE',  ( 63.92499999726880588, 164.1591823560292198, 12.60653300113718167 ) ) ;
#14885 = ORIENTED_EDGE ( 'NONE', *, *, #31107, .F. ) ;
#14884 = CARTESIAN_POINT ( 'NONE',  ( -6.220909254589537696, 198.5229672870051445, 21.05113791807856671 ) ) ;
#14886 = CARTESIAN_POINT ( 'NONE',  ( 43.01132485994281751, 142.2402378747194405, 9.270509831248432420 ) ) ;
#14887 = CARTESIAN_POINT ( 'NONE',  ( 81.97499999726881015, 169.8198683612136222, 4.815267126137181997 ) ) ;
#14888 = CARTESIAN_POINT ( 'NONE',  ( -12.00000000000000711, 207.0476921513413515, 84.50113791807856956 ) ) ;
#14889 = DIRECTION ( 'NONE',  ( 0.000000000000000000, 0.000000000000000000, -1.000000000000000000 ) ) ;
#14890 = ORIENTED_EDGE ( 'NONE', *, *, #23368, .T. ) ;
#14891 = CARTESIAN_POINT ( 'NONE',  ( 7.456977232089471386, 196.8216656703012006, 70.44886208192144750 ) ) ;
#14892 = AXIS2_PLACEMENT_3D ( 'NONE', #1090, #16580, #13359 ) ;
#14893 = CARTESIAN_POINT ( 'NONE',  ( -8.062137200540822946, 201.0835637161416400, 74.19886208192143329 ) ) ;
#14894 = CARTESIAN_POINT ( 'NONE',  ( -11.98450388067341876, 203.0532714938636047, 14.34886208192143364 ) ) ;
#14895 = DIRECTION ( 'NONE',  ( 1.000000000000000000, -0.000000000000000000, -0.000000000000000000 ) ) ;
#14896 = CARTESIAN_POINT ( 'NONE',  ( -10.00000000000000711, 207.0476921513413515, 36.50113791807857666 ) ) ;
#14897 = EDGE_LOOP ( 'NONE', ( #10059, #26063, #20439, #1622 ) ) ;
#14898 = CARTESIAN_POINT ( 'NONE',  ( -9.984503880673420539, 203.7031108863293980, 95.34886208192142476 ) ) ;
#14899 = DIRECTION ( 'NONE',  ( -0.5000000000000061062, 1.060575238724902601E-16, -0.8660254037844351549 ) ) ;
#14900 = VECTOR ( 'NONE', #26767, 1000.000000000000000 ) ;
#14901 = ORIENTED_EDGE ( 'NONE', *, *, #2242, .F. ) ;
#14902 = CARTESIAN_POINT ( 'NONE',  ( 16.00000000000000000, 0.000000000000000000, 1.610000000000000098 ) ) ;
#14903 = CARTESIAN_POINT ( 'NONE',  ( 0.05014649552828262524, 198.5883022060938572, 79.74886208192143044 ) ) ;
#14904 = VECTOR ( 'NONE', #28941, 1000.000000000000000 ) ;
#14905 = ORIENTED_EDGE ( 'NONE', *, *, #9402, .F. ) ;
#14906 = DIRECTION ( 'NONE',  ( 0.000000000000000000, 0.000000000000000000, -1.000000000000000000 ) ) ;
#14907 = ORIENTED_EDGE ( 'NONE', *, *, #6797, .F. ) ;
#14908 = CARTESIAN_POINT ( 'NONE',  ( 7.968863443239234456, 4.547634245050474533, -8.057411785091787237 ) ) ;
#14909 = ADVANCED_BREP_SHAPE_REPRESENTATION ( '', ( #672, #2404 ), #27952 ) ;
#14910 = CARTESIAN_POINT ( 'NONE',  ( 73.07499999726880446, 141.7447067706911810, -9.630534252274387086 ) ) ;
#14911 = CARTESIAN_POINT ( 'NONE',  ( 79.72499999726881015, 169.8198683612136222, 4.815267126137181997 ) ) ;
#14912 = DIRECTION ( 'NONE',  ( 0.000000000000000000, 0.000000000000000000, 1.000000000000000000 ) ) ;
#14913 = CARTESIAN_POINT ( 'NONE',  ( -4.903702542908602524, 213.8346818373418898, 81.95113791807858661 ) ) ;
#14914 = FACE_OUTER_BOUND ( 'NONE', #18832, .T. ) ;
#14915 = EDGE_CURVE ( 'NONE', #21869, #9926, #1204, .T. ) ;
#14916 = COLOUR_RGB ( '', 0.09019608, 0.27058824, 0.51372549) ;
#14917 = CARTESIAN_POINT ( 'NONE',  ( 42.79999999999999716, 167.3344367211045096, -8.961492836873482304 ) ) ;
#14918 = CARTESIAN_POINT ( 'NONE',  ( 8.000000000000008882, 207.0476921513415220, 51.99886208192144466 ) ) ;
#14919 = EDGE_CURVE ( 'NONE', #6813, #3136, #7200, .T. ) ;
#14920 = EDGE_CURVE ( 'NONE', #14849, #3157, #27194, .T. ) ;
#14921 = CARTESIAN_POINT ( 'NONE',  ( -6.500000000000000000, -3.752776749732573247, -0.8000000000000003775 ) ) ;
#14922 = CARTESIAN_POINT ( 'NONE',  ( -67.50000000000000000, -92.00000000000000000, 270.4495957273638282 ) ) ;
#14923 = AXIS2_PLACEMENT_3D ( 'NONE', #4404, #6967, #27907 ) ;
#14924 = DIRECTION ( 'NONE',  ( -1.000000000000000000, -0.000000000000000000, -0.000000000000000000 ) ) ;
#14925 = CARTESIAN_POINT ( 'NONE',  ( 54.92499999726881299, 145.8408176439707802, -12.60653300113719588 ) ) ;
#14926 = CARTESIAN_POINT ( 'NONE',  ( 62.67499999726879878, 141.7447067706911810, 9.630534252274376428 ) ) ;
#14927 = CARTESIAN_POINT ( 'NONE',  ( 11.98450388067348271, 203.0532714938637753, 59.15113791807857524 ) ) ;
#14928 = CARTESIAN_POINT ( 'NONE',  ( -128.2263702798682630, -4.198250922590447409, 35.00001199999999812 ) ) ;
#14929 = CARTESIAN_POINT ( 'NONE',  ( -9.736236675707914401, 199.9851607334237542, 3.201137918078565736 ) ) ;
#14930 = CARTESIAN_POINT ( 'NONE',  ( 10.01549611932653860, 210.2015048109876716, 82.85113791807856387 ) ) ;
#14931 = CARTESIAN_POINT ( 'NONE',  ( 3.753561863808876797, 195.6020594897209719, 46.59886208192143187 ) ) ;
#14932 = CARTESIAN_POINT ( 'NONE',  ( -8.062137200540822946, 201.0835637161416400, 44.19886208192143329 ) ) ;
#14933 = FACE_OUTER_BOUND ( 'NONE', #17664, .T. ) ;
#14934 = CARTESIAN_POINT ( 'NONE',  ( 7.456977232089302632, 217.1783343296989131, 85.55113791807858092 ) ) ;
#14935 = DIRECTION ( 'NONE',  ( -1.000000000000000000, -0.000000000000000000, -0.000000000000000000 ) ) ;
#14936 = CARTESIAN_POINT ( 'NONE',  ( -10.01549611932653860, 203.7984951890123284, 6.351137918078566535 ) ) ;
#14937 = CARTESIAN_POINT ( 'NONE',  ( -0.05014649552828403384, 217.5146222423826714, 69.24886208192144466 ) ) ;
#14938 = DIRECTION ( 'NONE',  ( -1.000000000000000000, -0.000000000000000000, -0.000000000000000000 ) ) ;
#14939 = ORIENTED_EDGE ( 'NONE', *, *, #18522, .F. ) ;
#14940 = CARTESIAN_POINT ( 'NONE',  ( -9.680171189290716072, 199.9079932115567146, 68.19886208192143329 ) ) ;
#14941 = MECHANICAL_DESIGN_GEOMETRIC_PRESENTATION_REPRESENTATION (  '', ( #245 ), #20931 ) ;
#14942 = ORIENTED_EDGE ( 'NONE', *, *, #28872, .T. ) ;
#14943 = CARTESIAN_POINT ( 'NONE',  ( 75.67499999726881299, 168.2552932293087906, -9.630534252274385310 ) ) ;
#14944 = CARTESIAN_POINT ( 'NONE',  ( 4.903702542908435547, 213.8346818373419751, 48.54886208192144181 ) ) ;
#14945 = EDGE_CURVE ( 'NONE', #10227, #27344, #237, .T. ) ;
#14946 = ORIENTED_EDGE ( 'NONE', *, *, #13835, .T. ) ;
#14947 = CARTESIAN_POINT ( 'NONE',  ( 70.12499999726881583, 155.0000000000000000, 15.58253174999999402 ) ) ;
#14948 = CARTESIAN_POINT ( 'NONE',  ( 6.499999999999999112, -3.752776749732576356, -0.8000000000000003775 ) ) ;
#14949 = CARTESIAN_POINT ( 'NONE',  ( -67.50000000000000000, 122.1366465496900275, 17.00000000000001421 ) ) ;
#14950 = CARTESIAN_POINT ( 'NONE',  ( 57.12499999726880873, 155.0000000000000000, -15.58253175000000823 ) ) ;
#14951 = DIRECTION ( 'NONE',  ( -1.000000000000000000, 0.000000000000000000, 0.000000000000000000 ) ) ;
#14952 = EDGE_CURVE ( 'NONE', #6511, #11008, #24607, .T. ) ;
#14953 = CARTESIAN_POINT ( 'NONE',  ( 0.05014649552828275708, 196.4853777576173002, 43.74886208192141623 ) ) ;
#14954 = ORIENTED_EDGE ( 'NONE', *, *, #23067, .F. ) ;
#14955 = FACE_OUTER_BOUND ( 'NONE', #3915, .T. ) ;
#14956 = CARTESIAN_POINT ( 'NONE',  ( -64.50000000000000000, 0.000000000000000000, -20.00000000000000000 ) ) ;
#14957 = CARTESIAN_POINT ( 'NONE',  ( 0.000000000000000000, 0.000000000000000000, 0.000000000000000000 ) ) ;
#14958 = CARTESIAN_POINT ( 'NONE',  ( 8.000000000000008882, 207.0476921513415220, 24.99886208192143400 ) ) ;
#14959 = CARTESIAN_POINT ( 'NONE',  ( 6.139770520408368348, 198.4640165459539674, 74.45113791807857240 ) ) ;
#14960 = PLANE ( 'NONE',  #22353 ) ;
#14961 = CARTESIAN_POINT ( 'NONE',  ( -0.05014649552810635652, 196.4853777576173002, 50.75113791807856956 ) ) ;
#14962 = CARTESIAN_POINT ( 'NONE',  ( -10.01549611932653860, 203.7984951890123284, 21.35113791807855677 ) ) ;
#14963 = CARTESIAN_POINT ( 'NONE',  ( -8.000000000000008882, 207.0476921513413515, 6.501137918078566891 ) ) ;
#14964 = CARTESIAN_POINT ( 'NONE',  ( 32.50000000000000000, 155.0000000000000000, -6.938893903907228378E-15 ) ) ;
#14965 = DIRECTION ( 'NONE',  ( 1.000000000000000000, 0.000000000000000000, 0.000000000000000000 ) ) ;
#14966 = CARTESIAN_POINT ( 'NONE',  ( 9.680171189290831535, 199.9079932115568852, 29.30113791807857027 ) ) ;
#14967 = CARTESIAN_POINT ( 'NONE',  ( 104.9083388212530537, 155.0000000000000000, 32.00000000000000000 ) ) ;
#14968 = ADVANCED_FACE ( 'NONE', ( #9299 ), #9636, .F. ) ;
#14969 = CARTESIAN_POINT ( 'NONE',  ( -0.05014649552810635652, 196.4853777576173002, 77.75113791807856956 ) ) ;
#14970 = CARTESIAN_POINT ( 'NONE',  ( -10.00000000000000711, 207.0476921513413515, 51.50113791807857666 ) ) ;
#14971 = B_SPLINE_CURVE_WITH_KNOTS ( 'NONE', 3,
 ( #26642, #13688, #24601, #1262, #24088, #11657, #22040, #19486, #27654, #12158 ),
 .UNSPECIFIED., .F., .F.,
 ( 4, 2, 2, 2, 4 ),
 ( 0.000000000000000000, 0.001989602278884364858, 0.003979204557768729715, 0.005968806836653094139, 0.007958409115537459430 ),
 .UNSPECIFIED. ) ;
#14972 = LINE ( 'NONE', #22812, #23046 ) ;
#14973 = DIRECTION ( 'NONE',  ( -1.000000000000000000, 0.000000000000000000, 0.000000000000000000 ) ) ;
#14974 = CARTESIAN_POINT ( 'NONE',  ( 7.375838497908012492, 217.2372850707501186, 9.548862081921432932 ) ) ;
#14975 = CARTESIAN_POINT ( 'NONE',  ( 6.220909254589680693, 198.5229672870052582, 22.44886208192143329 ) ) ;
#14976 = CARTESIAN_POINT ( 'NONE',  ( 74.79999999453762882, 163.5228861582408797, 11.73074641843673049 ) ) ;
#14977 = ORIENTED_EDGE ( 'NONE', *, *, #9158, .F. ) ;
#14978 = CARTESIAN_POINT ( 'NONE',  ( -0.05014649552807705357, 194.3824533091408000, 56.75113791807857666 ) ) ;
#14979 = CARTESIAN_POINT ( 'NONE',  ( 8.015496119326531499, 209.5516654185219636, 76.85113791807856387 ) ) ;
#14980 = EDGE_CURVE ( 'NONE', #29217, #6439, #17646, .T. ) ;
#14981 = CARTESIAN_POINT ( 'NONE',  ( -6.220909254589682469, 215.4770327129946850, 44.94886208192143329 ) ) ;
#14982 = CARTESIAN_POINT ( 'NONE',  ( 75.61132485994281183, 150.1262045565064227, -15.00000000000002665 ) ) ;
#14983 = ORIENTED_EDGE ( 'NONE', *, *, #4964, .F. ) ;
#14984 = VERTEX_POINT ( 'NONE', #25310 ) ;
#14985 = EDGE_CURVE ( 'NONE', #33036, #30420, #24065, .T. ) ;
#14986 = ORIENTED_EDGE ( 'NONE', *, *, #19919, .F. ) ;
#14987 = CARTESIAN_POINT ( 'NONE',  ( -64.50000000000000000, -95.00000000000000000, -20.00000000000000000 ) ) ;
#14988 = CARTESIAN_POINT ( 'NONE',  ( 1.049032378833991030, 6.899894373156697291, -0.3607371497494544221 ) ) ;
#14989 = VERTEX_POINT ( 'NONE', #11862 ) ;
#14990 = CARTESIAN_POINT ( 'NONE',  ( -0.05014649552807731031, 198.5883022060938572, 35.75113791807857666 ) ) ;
#14991 = DIRECTION ( 'NONE',  ( 0.000000000000000000, 0.000000000000000000, -1.000000000000000000 ) ) ;
#14992 = CARTESIAN_POINT ( 'NONE',  ( -8.118202686958138514, 212.8392687619910930, 14.79886208192143648 ) ) ;
#14993 = CARTESIAN_POINT ( 'NONE',  ( 53.97499999726881015, 169.8198683612136222, 4.815267126137181997 ) ) ;
#14994 = EDGE_LOOP ( 'NONE', ( #4493, #20807, #17620, #3205 ) ) ;
#14995 = CARTESIAN_POINT ( 'NONE',  ( 8.000000000000008882, 206.9523078486586485, 59.00113791807857666 ) ) ;
#14996 = CARTESIAN_POINT ( 'NONE',  ( 0.000000000000000000, 0.000000000000000000, -17.97459999999999525 ) ) ;
#14997 = CARTESIAN_POINT ( 'NONE',  ( -63.49999999999884892, 215.0000000000000000, -2.500000000000000000 ) ) ;
#14998 = CARTESIAN_POINT ( 'NONE',  ( -10.00000000000000711, 206.9523078486584495, 95.49886208192144466 ) ) ;
#14999 = CARTESIAN_POINT ( 'NONE',  ( 65.07499999726881867, 141.7447067706911810, -9.630534252274385310 ) ) ;
#15000 = CARTESIAN_POINT ( 'NONE',  ( -10.01549611932653860, 203.7984951890123284, 36.35113791807857098 ) ) ;
#15001 = CYLINDRICAL_SURFACE ( 'NONE', #6188, 19.99999999999998934 ) ;
#15002 = CARTESIAN_POINT ( 'NONE',  ( 10.00000000000000711, 206.9523078486586201, 20.00113791807856600 ) ) ;
#15003 = DIRECTION ( 'NONE',  ( 1.224646799147353207E-16, -4.064521778635712183E-50, -1.000000000000000000 ) ) ;
#15004 = CARTESIAN_POINT ( 'NONE',  ( 84.00000000000000000, 139.7537977485451393, -4.138211985947621020E-15 ) ) ;
#15005 = PRESENTATION_STYLE_ASSIGNMENT (( #33238 ) ) ;
#15006 = DIRECTION ( 'NONE',  ( -1.000000000000000000, 0.000000000000000000, 0.000000000000000000 ) ) ;
#15007 = CARTESIAN_POINT ( 'NONE',  ( -7.375838497908182134, 217.2372850707499765, 3.951137918078565736 ) ) ;
#15008 = CARTESIAN_POINT ( 'NONE',  ( 117.5000000000000000, 258.9084171661918958, -28.95509836041982510 ) ) ;
#15009 = CARTESIAN_POINT ( 'NONE',  ( 49.27499999726880020, 149.9369285172503510, -15.58253175000000823 ) ) ;
#15010 = ADVANCED_FACE ( 'NONE', ( #9132 ), #25725, .T. ) ;
#15011 = CARTESIAN_POINT ( 'NONE',  ( 9.984503880673470277, 203.7031108863295401, 50.15113791807855392 ) ) ;
#15012 = ADVANCED_FACE ( 'NONE', ( #6917 ), #22584, .T. ) ;
#15013 = CARTESIAN_POINT ( 'NONE',  ( 84.52499999726880731, 140.1801316387863778, 4.815267126137185549 ) ) ;
#15014 = LINE ( 'NONE', #19956, #32568 ) ;
#15015 = CARTESIAN_POINT ( 'NONE',  ( 54.49999999453761745, 170.2462022514548323, -7.872454543227099337E-15 ) ) ;
#15016 = ORIENTED_EDGE ( 'NONE', *, *, #6413, .T. ) ;
#15017 =( BOUNDED_CURVE ( )  B_SPLINE_CURVE ( 2, ( #24051, #21829, #3435, #32060, #8722, #558, #10951, #6156, #16550, #3604, #13998 ),
 .UNSPECIFIED., .F., .F. ) 
 B_SPLINE_CURVE_WITH_KNOTS ( ( 3, 2, 2, 2, 2, 3 ),
 ( 0.9642857142857140795, 0.9678571428571427493, 0.9714285714285713080, 0.9749999999999999778, 0.9785714285714285365, 0.9821428571428570953 ),
 .UNSPECIFIED. ) 
 CURVE ( )  GEOMETRIC_REPRESENTATION_ITEM ( )  RATIONAL_B_SPLINE_CURVE ( ( 1.000000000000001554, 0.9510565162951518658, 1.000000000000000000, 0.9510565162951534202, 1.000000000000000000, 0.9510565162951534202, 1.000000000000000000, 0.9510565162951534202, 1.000000000000000000, 0.9510565162951534202, 1.000000000000000000 ) ) 
 REPRESENTATION_ITEM ( '' )  );
#15018 = CARTESIAN_POINT ( 'NONE',  ( -7.456977232089304408, 196.8216656703010301, 33.05113791807856671 ) ) ;
#15019 = ADVANCED_FACE ( 'NONE', ( #4022 ), #1632, .T. ) ;
#15020 = FACE_OUTER_BOUND ( 'NONE', #20013, .T. ) ;
#15021 = CARTESIAN_POINT ( 'NONE',  ( -6.220909254589682469, 215.4770327129946850, 11.94886208192143684 ) ) ;
#15022 = DIRECTION ( 'NONE',  ( 0.000000000000000000, 0.000000000000000000, -1.000000000000000000 ) ) ;
#15023 = EDGE_LOOP ( 'NONE', ( #19499, #17582, #11267, #26931 ) ) ;
#15024 = CARTESIAN_POINT ( 'NONE',  ( 3.135527875058820690, 216.4958274776887492, 4.401137918078565470 ) ) ;
#15025 = CARTESIAN_POINT ( 'NONE',  ( 9.984503880673470277, 203.7031108863295401, 59.15113791807858235 ) ) ;
#15026 = ORIENTED_EDGE ( 'NONE', *, *, #14599, .F. ) ;
#15027 = CARTESIAN_POINT ( 'NONE',  ( 2.517493886309087436, 199.4062855549015865, 25.59886208192143897 ) ) ;
#15028 = VERTEX_POINT ( 'NONE', #22079 ) ;
#15029 = CARTESIAN_POINT ( 'NONE',  ( -6.500168698208129925, 202.3363017425936050, 3.201137918078566624 ) ) ;
#15030 = DIRECTION ( 'NONE',  ( 0.000000000000000000, 0.000000000000000000, 1.000000000000000000 ) ) ;
#15031 = CARTESIAN_POINT ( 'NONE',  ( -11.98450388067341876, 203.0532714938636047, 92.34886208192143897 ) ) ;
#15032 = CARTESIAN_POINT ( 'NONE',  ( 39.67499999726881299, 168.2552932293087906, -9.630534252274387086 ) ) ;
#15033 = EDGE_LOOP ( 'NONE', ( #6372, #1524 ) ) ;
#15034 = CARTESIAN_POINT ( 'NONE',  ( 45.72499999726881015, 169.8198683612136222, 4.815267126137181997 ) ) ;
#15035 = DIRECTION ( 'NONE',  ( -1.000000000000000000, -0.000000000000000000, -0.000000000000000000 ) ) ;
#15036 = CARTESIAN_POINT ( 'NONE',  ( 10.01549611932653860, 210.2015048109876716, 1.851137918078565203 ) ) ;
#15037 = CARTESIAN_POINT ( 'NONE',  ( -3.135527875058982783, 216.4958274776886924, 75.09886208192143897 ) ) ;
#15038 = CARTESIAN_POINT ( 'NONE',  ( 48.47499999726880304, 149.9369285172503510, 15.58253174999999580 ) ) ;
#15039 = CARTESIAN_POINT ( 'NONE',  ( 117.5000000000000000, 207.9999999999998010, -93.94869280115065635 ) ) ;
#15040 = CARTESIAN_POINT ( 'NONE',  ( -0.05014649552810635652, 196.4853777576173002, 2.751137918078565114 ) ) ;
#15041 = DIRECTION ( 'NONE',  ( -0.000000000000000000, -0.000000000000000000, 1.000000000000000000 ) ) ;
#15042 = AXIS2_PLACEMENT_3D ( 'NONE', #7804, #465, #7975 ) ;
#15043 = CARTESIAN_POINT ( 'NONE',  ( 59.10000000000000142, 168.7903194862797420, 4.480746418436729606 ) ) ;
#15044 = CARTESIAN_POINT ( 'NONE',  ( 9.984503880673470277, 203.7031108863295401, 86.15113791807857524 ) ) ;
#15045 = FACE_OUTER_BOUND ( 'NONE', #7580, .T. ) ;
#15046 = CARTESIAN_POINT ( 'NONE',  ( -3.044812012440131443, 216.5253028482142952, 73.10113791807857808 ) ) ;
#15047 = CARTESIAN_POINT ( 'NONE',  ( -7.169303301815100227, 4.521054846639364300, -7.349897473154783256 ) ) ;
#15048 = DIRECTION ( 'NONE',  ( 1.000000000000000000, -0.000000000000000000, -0.000000000000000000 ) ) ;
#15049 = CARTESIAN_POINT ( 'NONE',  ( -12.00000000000000711, 206.9523078486584780, 89.49886208192144466 ) ) ;
#15050 = CARTESIAN_POINT ( 'NONE',  ( 63.02499999726882152, 149.9369285172503510, -15.58253175000000823 ) ) ;
#15052 = ORIENTED_EDGE ( 'NONE', *, *, #13490, .T. ) ;
#15051 = CARTESIAN_POINT ( 'NONE',  ( -3.044812012440131443, 216.5253028482142952, 34.10113791807857808 ) ) ;
#15053 = CARTESIAN_POINT ( 'NONE',  ( -58.66318290517560996, 194.9217985566783113, -2.499999999999999556 ) ) ;
#15054 = CARTESIAN_POINT ( 'NONE',  ( 34.29999999453762882, 167.3344367211045096, -8.961492836873482304 ) ) ;
#15055 = CARTESIAN_POINT ( 'NONE',  ( -3.753561863808691168, 195.6020594897209435, 95.90113791807857524 ) ) ;
#15056 = CARTESIAN_POINT ( 'NONE',  ( -10.15808088729814074, 205.9638919399499457, 104.4339049140729543 ) ) ;
#15057 = ORIENTED_EDGE ( 'NONE', *, *, #12519, .F. ) ;
#15058 = AXIS2_PLACEMENT_3D ( 'NONE', #31339, #33396, #7 ) ;
#15059 = CARTESIAN_POINT ( 'NONE',  ( 3.044812012439969795, 216.5253028482143520, 87.39886208192143613 ) ) ;
#15060 = CARTESIAN_POINT ( 'NONE',  ( -11.98450388067341876, 203.0532714938636047, 26.34886208192143897 ) ) ;
#15061 = FACE_OUTER_BOUND ( 'NONE', #25886, .T. ) ;
#15062 = CARTESIAN_POINT ( 'NONE',  ( 10.00000000000000711, 206.9523078486586201, 32.00113791807856956 ) ) ;
#15063 = CARTESIAN_POINT ( 'NONE',  ( 110.1179863365115636, 155.0000000000000000, 0.000000000000000000 ) ) ;
#15064 = CARTESIAN_POINT ( 'NONE',  ( 10.00000000000000711, 207.0476921513415220, 99.99886208192143044 ) ) ;
#15065 = VECTOR ( 'NONE', #3887, 1000.000000000000114 ) ;
#15066 = CARTESIAN_POINT ( 'NONE',  ( 115.4999999999999858, 102.0000000000001990, 89.64869280115065919 ) ) ;
#15067 = EDGE_LOOP ( 'NONE', ( #13939, #6984 ) ) ;
#15068 = CARTESIAN_POINT ( 'NONE',  ( 70.31132485994280046, 169.2658477444273331, 4.635254915624208216 ) ) ;
#15069 = CARTESIAN_POINT ( 'NONE',  ( -4.903702542908436435, 200.1653181626580249, 80.04886208192144181 ) ) ;
#15070 = ORIENTED_EDGE ( 'NONE', *, *, #27364, .F. ) ;
#15071 = CARTESIAN_POINT ( 'NONE',  ( 69.71132485994280614, 155.0000000000000000, -15.00000000000002487 ) ) ;
#15072 = ORIENTED_EDGE ( 'NONE', *, *, #23977, .T. ) ;
#15073 = DIRECTION ( 'NONE',  ( 1.000000000000000000, 0.000000000000000000, -0.000000000000000000 ) ) ;
#15074 = VECTOR ( 'NONE', #19432, 1000.000000000000000 ) ;
#15075 = CARTESIAN_POINT ( 'NONE',  ( 83.72499999726882436, 169.8198683612136222, 4.815267126137181997 ) ) ;
#15076 = CARTESIAN_POINT ( 'NONE',  ( 0.1999999999999987899, 0.000000000000000000, 0.000000000000000000 ) ) ;
#15077 = CARTESIAN_POINT ( 'NONE',  ( -6.500168698208129925, 202.3363017425936050, 78.20113791807857240 ) ) ;
#15078 = CARTESIAN_POINT ( 'NONE',  ( 112.4999999999999858, 155.0000000000000000, -6.938893903907228378E-15 ) ) ;
#15079 = VECTOR ( 'NONE', #7330, 1000.000000000000000 ) ;
#15080 = VECTOR ( 'NONE', #28582, 1000.000000000000000 ) ;
#15081 = B_SPLINE_CURVE_WITH_KNOTS ( 'NONE', 3,
 ( #27024, #5902, #24642, #26687, #16126, #3348, #14077, #31963 ),
 .UNSPECIFIED., .F., .F.,
 ( 4, 2, 2, 4 ),
 ( 0.04438889715320012280, 0.04840678451617882322, 0.05242467187915753057, 0.06046044660511493141 ),
 .UNSPECIFIED. ) ;
#15082 = CARTESIAN_POINT ( 'NONE',  ( 39.59999999999999432, 150.2886644046228639, 14.49999999999999645 ) ) ;
#15083 = CARTESIAN_POINT ( 'NONE',  ( 7.984503880673422316, 209.6470497212048372, 51.84886208192144608 ) ) ;
#15084 = CIRCLE ( 'NONE', #13457, 3.499999999999999556 ) ;
#15085 = CARTESIAN_POINT ( 'NONE',  ( -10.00000000000000711, 207.0476921513413515, 3.501137918078566003 ) ) ;
#15086 = CARTESIAN_POINT ( 'NONE',  ( 115.4999999999999858, 207.9999999999998010, -93.94869280115064214 ) ) ;
#15087 = CARTESIAN_POINT ( 'NONE',  ( -31.74999999999995737, 0.000000000000000000, 0.000000000000000000 ) ) ;
#15088 = CARTESIAN_POINT ( 'NONE',  ( 56.62499999726880162, 138.6155565068815747, -3.929120461958505118E-15 ) ) ;
#15089 = CARTESIAN_POINT ( 'NONE',  ( 70.87499999726878741, 138.6155565068815463, -3.929120461958505118E-15 ) ) ;
#15090 = CARTESIAN_POINT ( 'NONE',  ( -0.05014649552807705357, 194.3824533091408000, 62.75113791807856245 ) ) ;
#15091 = CARTESIAN_POINT ( 'NONE',  ( 45.81132485994281467, 159.8737954434936910, -14.99999999999998046 ) ) ;
#15092 = CARTESIAN_POINT ( 'NONE',  ( -9.680171189290831535, 214.0920067884431148, 6.801137918078565825 ) ) ;
#15093 = CARTESIAN_POINT ( 'NONE',  ( 10.00000000000000711, 206.9523078486586201, 77.00113791807858377 ) ) ;
#15094 = CARTESIAN_POINT ( 'NONE',  ( -11.98450388067341876, 203.0532714938636047, 41.34886208192143187 ) ) ;
#15095 = CARTESIAN_POINT ( 'NONE',  ( -6.220909254589682469, 215.4770327129947134, 53.94886208192143329 ) ) ;
#15096 = CARTESIAN_POINT ( 'NONE',  ( -6.500000000000000888, 0.6470732608156811727, -0.01945970098673090176 ) ) ;
#15097 = CARTESIAN_POINT ( 'NONE',  ( -0.05014649552807705357, 194.3824533091408000, 89.75113791807858377 ) ) ;
#15098 = DIRECTION ( 'NONE',  ( 1.000000000000000000, 0.000000000000000000, 0.000000000000000000 ) ) ;
#15099 = AXIS2_PLACEMENT_3D ( 'NONE', #18525, #31791, #19183 ) ;
#15100 = CARTESIAN_POINT ( 'NONE',  ( -10.00000000000000711, 207.0476921513413515, 0.5011379180785656695 ) ) ;
#15101 = CARTESIAN_POINT ( 'NONE',  ( -3.135527875058982783, 216.4958274776886924, 66.09886208192143897 ) ) ;
#15102 = EDGE_CURVE ( 'NONE', #31012, #6694, #10520, .T. ) ;
#15103 = AXIS2_PLACEMENT_3D ( 'NONE', #19338, #30069, #29732 ) ;
#15104 = DIRECTION ( 'NONE',  ( 1.000000000000000000, 4.625929269271485914E-16, 0.000000000000000000 ) ) ;
#15105 = VERTEX_POINT ( 'NONE', #24641 ) ;
#15106 = CARTESIAN_POINT ( 'NONE',  ( -3.753561863808878130, 218.3979405102790281, 69.09886208192143897 ) ) ;
#15107 = ORIENTED_EDGE ( 'NONE', *, *, #8334, .T. ) ;
#15108 = CARTESIAN_POINT ( 'NONE',  ( 78.17499999726881299, 164.1591823560292198, 12.60653300113718167 ) ) ;
#15109 = CARTESIAN_POINT ( 'NONE',  ( -6.500168698208244500, 211.6636982574061676, 56.79886208192143471 ) ) ;
#15110 = ORIENTED_EDGE ( 'NONE', *, *, #17467, .F. ) ;
#15111 = CONICAL_SURFACE ( 'NONE', #15676, 12.00000000000001066, 0.1047197551196740739 ) ;
#15112 = CARTESIAN_POINT ( 'NONE',  ( 69.42499999726881299, 168.2552932293087906, -9.630534252274387086 ) ) ;
#15113 = LINE ( 'NONE', #30626, #20041 ) ;
#15114 = CARTESIAN_POINT ( 'NONE',  ( 0.000000000000000000, 2.342598717236900718, -4.057500000000001883 ) ) ;
#15115 = CARTESIAN_POINT ( 'NONE',  ( 65.52499999726880731, 169.8198683612136222, -4.815267126137197984 ) ) ;
#15116 = CARTESIAN_POINT ( 'NONE',  ( 4.000000000000000000, -3.518949890710769246, 3.686287386450715076E-15 ) ) ;
#15117 = CARTESIAN_POINT ( 'NONE',  ( 10.01549611932659545, 203.7984951890123853, 43.14886208192142192 ) ) ;
#15118 = EDGE_LOOP ( 'NONE', ( #26429, #13888, #3111, #28199 ) ) ;
#15119 = PLANE ( 'NONE',  #24905 ) ;
#15120 =( LENGTH_UNIT ( ) NAMED_UNIT ( * ) SI_UNIT ( .MILLI., .METRE. ) );
#15121 = CARTESIAN_POINT ( 'NONE',  ( 6.781345014477444089, -3.590342129888862921, -6.122077150241852728 ) ) ;
#15122 = CARTESIAN_POINT ( 'NONE',  ( 86.31132485994280046, 169.2658477444273331, 4.635254915624208216 ) ) ;
#15123 = CARTESIAN_POINT ( 'NONE',  ( -2.517493886309087880, 214.5937144450984135, 27.09886208192143897 ) ) ;
#15124 = CARTESIAN_POINT ( 'NONE',  ( 6.220909254589536808, 215.4770327129947702, 70.55113791807856671 ) ) ;
#15125 = FACE_OUTER_BOUND ( 'NONE', #11427, .T. ) ;
#15126 = CARTESIAN_POINT ( 'NONE',  ( 0.05014649552810505201, 217.5146222423826714, 52.25113791807856245 ) ) ;
#15127 = VECTOR ( 'NONE', #28983, 1000.000000000000000 ) ;
#15128 = AXIS2_PLACEMENT_3D ( 'NONE', #25982, #20703, #12532 ) ;
#15129 = CARTESIAN_POINT ( 'NONE',  ( -3.044812012440131443, 216.5253028482142952, 22.10113791807856742 ) ) ;
#15130 = CARTESIAN_POINT ( 'NONE',  ( -6.444103211791042618, 211.7408657792732356, 9.801137918078564937 ) ) ;
#15131 = DIRECTION ( 'NONE',  ( 0.000000000000000000, 0.000000000000000000, -1.000000000000000000 ) ) ;
#15132 = CARTESIAN_POINT ( 'NONE',  ( 40.72499999726881725, 140.1801316387863778, -4.815267126137194431 ) ) ;
#15133 = CARTESIAN_POINT ( 'NONE',  ( -12.00000000000000711, 207.0476921513413515, 30.50113791807856600 ) ) ;
#15134 = CARTESIAN_POINT ( 'NONE',  ( 109.0104235265664272, 155.0000000000000000, -11.99999999999998224 ) ) ;
#15135 = EDGE_CURVE ( 'NONE', #320, #21727, #11632, .T. ) ;
#15136 = CARTESIAN_POINT ( 'NONE',  ( -9.984503880673473830, 210.2968891136704315, 75.65113791807858945 ) ) ;
#15137 = CARTESIAN_POINT ( 'NONE',  ( -3.135527875058821579, 197.5041725223112223, 50.90113791807856813 ) ) ;
#15138 = AXIS2_PLACEMENT_3D ( 'NONE', #15187, #18034, #10547 ) ;
#15139 = DIRECTION ( 'NONE',  ( 0.9945218953682689600, 0.000000000000000000, -0.1045284632676951458 ) ) ;
#15140 = CARTESIAN_POINT ( 'NONE',  ( 78.78867513459481131, 155.0000000000000000, -15.00000000000002487 ) ) ;
#15141 = CARTESIAN_POINT ( 'NONE',  ( -11.98450388067341876, 203.0532714938636047, 14.34886208192143364 ) ) ;
#15142 = CARTESIAN_POINT ( 'NONE',  ( -8.062137200540822946, 201.0835637161416400, 20.19886208192143684 ) ) ;
#15143 = CARTESIAN_POINT ( 'NONE',  ( 73.29999999453762882, 142.6655632788954620, 8.961492836873471646 ) ) ;
#15144 = ORIENTED_EDGE ( 'NONE', *, *, #26748, .T. ) ;
#15145 = CARTESIAN_POINT ( 'NONE',  ( -12.01549611932652972, 203.1486557965464499, 57.35113791807857098 ) ) ;
#15146 = CARTESIAN_POINT ( 'NONE',  ( -2.517493886308901807, 199.4062855549015012, 77.90113791807856103 ) ) ;
#15147 = CARTESIAN_POINT ( 'NONE',  ( -10.00000000000000711, 206.9523078486584495, 38.49886208192143755 ) ) ;
#15148 = ADVANCED_FACE ( 'NONE', ( #19857, #33154 ), #27523, .T. ) ;
#15149 = ORIENTED_EDGE ( 'NONE', *, *, #4528, .T. ) ;
#15150 = CARTESIAN_POINT ( 'NONE',  ( 9.680171189290716072, 214.0920067884432854, 45.69886208192143329 ) ) ;
#15151 = ORIENTED_EDGE ( 'NONE', *, *, #29706, .T. ) ;
#15152 = VECTOR ( 'NONE', #24808, 1000.000000000000000 ) ;
#15153 = ORIENTED_EDGE ( 'NONE', *, *, #20863, .F. ) ;
#15154 = PRODUCT_DEFINITION_SHAPE ( 'NONE', 'NONE',  #27705 ) ;
#15155 = CIRCLE ( 'NONE', #19507, 24.99999999999999289 ) ;
#15156 = DIRECTION ( 'NONE',  ( 0.000000000000000000, 0.000000000000000000, -1.000000000000000000 ) ) ;
#15157 = EDGE_CURVE ( 'NONE', #25537, #8808, #29926, .T. ) ;
#15158 = CARTESIAN_POINT ( 'NONE',  ( 60.63708498984762940, 155.0000000000000000, 6.938893903907228378E-15 ) ) ;
#15159 = EDGE_LOOP ( 'NONE', ( #20732, #24199, #6881, #28538 ) ) ;
#15160 = CARTESIAN_POINT ( 'NONE',  ( -6.444103211791042618, 211.7408657792732356, 27.80113791807857027 ) ) ;
#15161 = DIRECTION ( 'NONE',  ( 1.000000000000000000, -0.000000000000000000, -0.000000000000000000 ) ) ;
#15162 = CARTESIAN_POINT ( 'NONE',  ( -6.139770520408224463, 198.4640165459539389, 14.04886208192143648 ) ) ;
#15163 = CARTESIAN_POINT ( 'NONE',  ( 55.67499999726880588, 168.2552932293087906, -9.630534252274387086 ) ) ;
#15165 = ORIENTED_EDGE ( 'NONE', *, *, #19799, .T. ) ;
#15164 = CONICAL_SURFACE ( 'NONE', #18457, 27.50000000000000355, 1.047197551196595411 ) ;
#15166 = CARTESIAN_POINT ( 'NONE',  ( -4.903702542908602524, 213.8346818373418898, 57.95113791807855819 ) ) ;
#15167 = PLANE ( 'NONE',  #4198 ) ;
#15168 = DIRECTION ( 'NONE',  ( -1.000000000000000000, 0.000000000000000000, 0.000000000000000000 ) ) ;
#15169 = CARTESIAN_POINT ( 'NONE',  ( 8.062137200540822946, 212.9164362838583315, 96.69886208192143329 ) ) ;
#15170 = CARTESIAN_POINT ( 'NONE',  ( 66.77499999726880731, 140.1801316387863778, 4.815267126137185549 ) ) ;
#15171 = CARTESIAN_POINT ( 'NONE',  ( -6.139770520408369237, 215.5359834540460042, 45.95113791807857950 ) ) ;
#15172 = CARTESIAN_POINT ( 'NONE',  ( 69.78867513459482552, 155.0000000000000000, 15.00000000000001243 ) ) ;
#15173 = EDGE_CURVE ( 'NONE', #20186, #16641, #4184, .T. ) ;
#15174 = CARTESIAN_POINT ( 'NONE',  ( -0.05014649552810635652, 196.4853777576173002, 20.75113791807855890 ) ) ;
#15175 = CARTESIAN_POINT ( 'NONE',  ( 32.50000000000000000, 155.0000000000000000, -6.938893903907228378E-15 ) ) ;
#15176 = CARTESIAN_POINT ( 'NONE',  ( 84.19999999999998863, 142.6655632788954620, -8.961492836873480528 ) ) ;
#15177 = DIRECTION ( 'NONE',  ( 0.000000000000000000, 0.000000000000000000, 1.000000000000000000 ) ) ;
#15178 = DIRECTION ( 'NONE',  ( 1.000000000000000000, 0.000000000000000000, 0.000000000000000000 ) ) ;
#15179 = CARTESIAN_POINT ( 'NONE',  ( -8.062137200540920645, 212.9164362838581894, 99.80113791807858092 ) ) ;
#15180 = FACE_BOUND ( 'NONE', #1039, .T. ) ;
#15181 = CARTESIAN_POINT ( 'NONE',  ( 48.07499999726881867, 168.2552932293087906, 9.630534252274372875 ) ) ;
#15182 = EDGE_CURVE ( 'NONE', #14808, #5021, #27698, .T. ) ;
#15183 = CARTESIAN_POINT ( 'NONE',  ( -3.135527875058821579, 197.5041725223112223, 44.90113791807857524 ) ) ;
#15184 = DIRECTION ( 'NONE',  ( 1.000000000000000000, 0.000000000000000000, 0.000000000000000000 ) ) ;
#15185 = CIRCLE ( 'NONE', #22247, 31.00000000000000000 ) ;
#15186 = CARTESIAN_POINT ( 'NONE',  ( 15.61000000000001364, 2.449293598294707400E-16, -2.000000000000000888 ) ) ;
#15187 = CARTESIAN_POINT ( 'NONE',  ( -31.74999999999995737, 0.000000000000000000, 0.000000000000000000 ) ) ;
#15188 = CYLINDRICAL_SURFACE ( 'NONE', #19515, 15.50000000000001066 ) ;
#15189 = CARTESIAN_POINT ( 'NONE',  ( 56.89999999453762314, 159.7113355953771077, 14.49999999999999289 ) ) ;
#15190 = ORIENTED_EDGE ( 'NONE', *, *, #32404, .F. ) ;
#15191 = CARTESIAN_POINT ( 'NONE',  ( 3.753561863808689836, 218.3979405102790565, 28.40113791807856813 ) ) ;
#15192 = CARTESIAN_POINT ( 'NONE',  ( 47.51132485994280330, 146.1832212156128890, -12.13525491562423042 ) ) ;
#15193 = CARTESIAN_POINT ( 'NONE',  ( 8.062137200540822946, 212.9164362838583315, 12.69886208192143506 ) ) ;
#15194 = DIRECTION ( 'NONE',  ( 0.000000000000000000, 0.000000000000000000, 1.000000000000000000 ) ) ;
#15195 = ORIENTED_EDGE ( 'NONE', *, *, #1070, .F. ) ;
#15196 = CARTESIAN_POINT ( 'NONE',  ( 8.062137200540920645, 201.0835637161417822, 8.301137918078566713 ) ) ;
#15197 = CARTESIAN_POINT ( 'NONE',  ( 10.01549611932653860, 210.2015048109876716, 73.85113791807857808 ) ) ;
#15198 = ORIENTED_EDGE ( 'NONE', *, *, #12602, .F. ) ;
#15199 = CARTESIAN_POINT ( 'NONE',  ( 2.426778023690075337, 214.6231898156240447, 24.39886208192143258 ) ) ;
#15200 = DIRECTION ( 'NONE',  ( 0.000000000000000000, 0.7071067811865442421, -0.7071067811865506814 ) ) ;
#15201 = ORIENTED_EDGE ( 'NONE', *, *, #17707, .F. ) ;
#15202 = CARTESIAN_POINT ( 'NONE',  ( 6.500168698208129925, 211.6636982574063381, 7.701137918078567068 ) ) ;
#15203 = EDGE_CURVE ( 'NONE', #8265, #253, #25136, .T. ) ;
#15204 = EDGE_CURVE ( 'NONE', #1664, #29281, #27346, .T. ) ;
#15205 = CARTESIAN_POINT ( 'NONE',  ( 9.680171189290716072, 214.0920067884432854, 93.69886208192144750 ) ) ;
#15206 = CARTESIAN_POINT ( 'NONE',  ( 40.07499999726880446, 168.2552932293087906, 9.630534252274372875 ) ) ;
#15207 = ORIENTED_EDGE ( 'NONE', *, *, #30439, .T. ) ;
#15208 = CARTESIAN_POINT ( 'NONE',  ( 46.22499999726880304, 149.9369285172503510, 15.58253174999999580 ) ) ;
#15209 = CARTESIAN_POINT ( 'NONE',  ( 7.500000000000000000, 4.330127018922199866, -1.000000000000000888 ) ) ;
#15210 = CARTESIAN_POINT ( 'NONE',  ( 6.139770520408368348, 198.4640165459539674, 2.451137918078566180 ) ) ;
#15211 = CARTESIAN_POINT ( 'NONE',  ( -8.062137200540822946, 201.0835637161416400, 74.19886208192143329 ) ) ;
#15212 = CARTESIAN_POINT ( 'NONE',  ( 45.07499999726880446, 141.7447067706911810, -9.630534252274385310 ) ) ;
#15213 = DIRECTION ( 'NONE',  ( -1.000000000000000000, -0.000000000000000000, -0.000000000000000000 ) ) ;
#15214 = CARTESIAN_POINT ( 'NONE',  ( -3.135527875058821579, 197.5041725223112223, 14.90113791807856636 ) ) ;
#15215 = CARTESIAN_POINT ( 'NONE',  ( -13.75000000000001243, -23.81569860407206107, 0.000000000000000000 ) ) ;
#15216 = EDGE_CURVE ( 'NONE', #14343, #4684, #7771, .T. ) ;
#15217 = CARTESIAN_POINT ( 'NONE',  ( 69.90000000000000568, 141.2096805137202580, 4.480746418436733158 ) ) ;
#15218 = CARTESIAN_POINT ( 'NONE',  ( -3.044812012440131443, 216.5253028482142952, 91.10113791807857808 ) ) ;
#15219 = DIRECTION ( 'NONE',  ( 0.000000000000000000, 0.4999999999999991118, -0.8660254037844391517 ) ) ;
#15220 = CARTESIAN_POINT ( 'NONE',  ( -10.00000000000000711, 207.0476921513413515, 72.50113791807858377 ) ) ;
#15221 = CARTESIAN_POINT ( 'NONE',  ( 0.3470952277635277472, 8.860649561028097310, -7.493596212620242447 ) ) ;
#15222 = CARTESIAN_POINT ( 'NONE',  ( 33.97499999726881725, 169.8198683612136222, 4.815267126137181997 ) ) ;
#15223 = EDGE_CURVE ( 'NONE', #17374, #11140, #30075, .T. ) ;
#15224 = CARTESIAN_POINT ( 'NONE',  ( -0.05014649552828442242, 219.6175466908591716, 87.24886208192144466 ) ) ;
#15225 = CARTESIAN_POINT ( 'NONE',  ( 70.32499999726881867, 145.8408176439707802, 12.60653300113718345 ) ) ;
#15227 = ORIENTED_EDGE ( 'NONE', *, *, #22513, .T. ) ;
#15226 = CARTESIAN_POINT ( 'NONE',  ( 10.00000000000000711, 206.9523078486586201, 29.00113791807856956 ) ) ;
#15228 = CARTESIAN_POINT ( 'NONE',  ( 43.61132485994281183, 150.1262045565064511, -15.00000000000005151 ) ) ;
#15229 = CARTESIAN_POINT ( 'NONE',  ( 35.89999999453763024, 150.2886644046228639, -14.50000000000000888 ) ) ;
#15230 = CARTESIAN_POINT ( 'NONE',  ( 7.375838497908181246, 196.7627149292499666, 98.45113791807858661 ) ) ;
#15231 = AXIS2_PLACEMENT_3D ( 'NONE', #27915, #12247, #31450 ) ;
#15232 = CARTESIAN_POINT ( 'NONE',  ( -10.30698760260085045, 206.0014576304403136, 104.3936231590492696 ) ) ;
#15233 = ORIENTED_EDGE ( 'NONE', *, *, #13835, .F. ) ;
#15234 = CARTESIAN_POINT ( 'NONE',  ( 0.05014649552828275014, 196.4853777576173002, 88.74886208192143044 ) ) ;
#15235 = CARTESIAN_POINT ( 'NONE',  ( 7.456977232089471386, 196.8216656703012006, 22.44886208192143329 ) ) ;
#15236 = DIRECTION ( 'NONE',  ( 0.000000000000000000, 0.000000000000000000, -1.000000000000000000 ) ) ;
#15237 = CARTESIAN_POINT ( 'NONE',  ( 9.984503880673470277, 203.7031108863295401, 35.15113791807856813 ) ) ;
#15238 = CARTESIAN_POINT ( 'NONE',  ( 66.68867513459485963, 150.1262045565066785, -15.00000000000021316 ) ) ;
#15239 = CARTESIAN_POINT ( 'NONE',  ( 0.05014649552828275708, 196.4853777576173002, 97.74886208192140202 ) ) ;
#15240 = CARTESIAN_POINT ( 'NONE',  ( 6.781345014477444977, 3.590342129888852263, -6.122077150241850951 ) ) ;
#15241 = ORIENTED_EDGE ( 'NONE', *, *, #4778, .F. ) ;
#15242 = DIRECTION ( 'NONE',  ( 0.000000000000000000, 0.000000000000000000, -1.000000000000000000 ) ) ;
#15243 = CARTESIAN_POINT ( 'NONE',  ( -8.000000000000008882, 206.9523078486584780, 83.49886208192144466 ) ) ;
#15244 = EDGE_LOOP ( 'NONE', ( #13895, #5879 ) ) ;
#15245 = CARTESIAN_POINT ( 'NONE',  ( 39.78867513459481842, 155.0000000000000000, 15.00000000000001243 ) ) ;
#15246 = ORIENTED_EDGE ( 'NONE', *, *, #4311, .F. ) ;
#15247 = PLANE ( 'NONE',  #4729 ) ;
#15248 = CARTESIAN_POINT ( 'NONE',  ( -4.984841277089726574, 200.2242689037092305, 57.05113791807856671 ) ) ;
#15249 = CARTESIAN_POINT ( 'NONE',  ( 81.82499999726879025, 168.2552932293087906, 9.630534252274372875 ) ) ;
#15250 = CARTESIAN_POINT ( 'NONE',  ( -5.007715329123872641E-16, -8.660254037844399733, -10.00000000000000000 ) ) ;
#15251 = CARTESIAN_POINT ( 'NONE',  ( -6.444103211791042618, 211.7408657792732356, 78.80113791807858092 ) ) ;
#15252 = DIRECTION ( 'NONE',  ( 0.000000000000000000, 0.000000000000000000, 1.000000000000000000 ) ) ;
#15253 = SURFACE_STYLE_FILL_AREA ( #28377 ) ;
#15254 = CARTESIAN_POINT ( 'NONE',  ( 46.10000000000000142, 141.2096805137202580, -4.480746418436742040 ) ) ;
#15255 = CARTESIAN_POINT ( 'NONE',  ( -4.984841277089891776, 213.7757310962905990, 59.94886208192144039 ) ) ;
#15256 = CARTESIAN_POINT ( 'NONE',  ( -54.30000000000002558, -88.00000000000000000, 20.00000000000000000 ) ) ;
#15257 = CARTESIAN_POINT ( 'NONE',  ( 3.044812012440130555, 197.4746971517856764, 2.601137918078566091 ) ) ;
#15258 = CARTESIAN_POINT ( 'NONE',  ( 50.71132485994280614, 155.0000000000000000, 15.00000000000001243 ) ) ;
#15259 = CONICAL_SURFACE ( 'NONE', #19614, 4.174999999999999822, 0.9599310885968795892 ) ;
#15260 = CARTESIAN_POINT ( 'NONE',  ( 97.30927364589244632, 155.0000000000000000, 0.000000000000000000 ) ) ;
#15261 = CARTESIAN_POINT ( 'NONE',  ( 57.92499999726881299, 164.1591823560292198, 12.60653300113718167 ) ) ;
#15262 = CARTESIAN_POINT ( 'NONE',  ( 67.47499999726879594, 160.0630714827496206, -15.58253175000000823 ) ) ;
#15263 = CARTESIAN_POINT ( 'NONE',  ( -0.05014649552807705357, 194.3824533091408000, 68.75113791807856956 ) ) ;
#15264 = DIRECTION ( 'NONE',  ( 0.000000000000000000, 1.000000000000000000, 0.000000000000000000 ) ) ;
#15265 = CARTESIAN_POINT ( 'NONE',  ( -7.456977232089304408, 196.8216656703010301, 12.05113791807856849 ) ) ;
#15266 = CARTESIAN_POINT ( 'NONE',  ( -9.984503880673475606, 210.2968891136704315, 90.65113791807856103 ) ) ;
#15267 = CARTESIAN_POINT ( 'NONE',  ( -7.456977232089471386, 217.1783343296987709, 47.94886208192143329 ) ) ;
#15268 = CARTESIAN_POINT ( 'NONE',  ( 6.139770520408223575, 215.5359834540460611, 54.54886208192144181 ) ) ;
#15269 = CARTESIAN_POINT ( 'NONE',  ( 112.4999999999999858, 155.0000000000000000, 11.99999999999999645 ) ) ;
#15270 = CARTESIAN_POINT ( 'NONE',  ( 9.680171189290831535, 199.9079932115568852, 98.30113791807858092 ) ) ;
#15271 = LINE ( 'NONE', #7279, #5589 ) ;
#15272 = CARTESIAN_POINT ( 'NONE',  ( 9.984503880673470277, 203.7031108863295401, 2.151137918078565914 ) ) ;
#15273 = CARTESIAN_POINT ( 'NONE',  ( 8.062137200540822946, 212.9164362838583315, 69.69886208192144750 ) ) ;
#15274 =( NAMED_UNIT ( * ) SI_UNIT ( $, .STERADIAN. ) SOLID_ANGLE_UNIT ( ) );
#15275 = VERTEX_POINT ( 'NONE', #13045 ) ;
#15276 = CARTESIAN_POINT ( 'NONE',  ( 12.00000000000000711, 207.0476921513415220, 78.99886208192144466 ) ) ;
#15277 = CARTESIAN_POINT ( 'NONE',  ( 6.139770520408368348, 198.4640165459539674, 86.45113791807854398 ) ) ;
#15278 = ORIENTED_EDGE ( 'NONE', *, *, #26799, .T. ) ;
#15279 = CARTESIAN_POINT ( 'NONE',  ( 75.77499999726880731, 169.8198683612136222, -4.815267126137197984 ) ) ;
#15280 = CARTESIAN_POINT ( 'NONE',  ( 0.05014649552828262524, 198.5883022060938572, 49.74886208192144466 ) ) ;
#15281 = EDGE_LOOP ( 'NONE', ( #20397, #26221, #9029, #8524 ) ) ;
#15282 = CARTESIAN_POINT ( 'NONE',  ( 69.52499999726880731, 169.8198683612136222, -4.815267126137197984 ) ) ;
#15283 = CARTESIAN_POINT ( 'NONE',  ( 6.499999999999398703, -1.392325603688425284, -6.058577540042510812 ) ) ;
#15284 = CARTESIAN_POINT ( 'NONE',  ( -5.040301471719076609, -5.750234626350520628, -0.09933465333851741741 ) ) ;
#15285 = CARTESIAN_POINT ( 'NONE',  ( 64.32499999726881867, 145.8408176439707802, 12.60653300113718345 ) ) ;
#15286 = CYLINDRICAL_SURFACE ( 'NONE', #24881, 4.199999999999988631 ) ;
#15287 = CARTESIAN_POINT ( 'NONE',  ( -3.135527875058982783, 216.4958274776886924, 51.09886208192143897 ) ) ;
#15288 = ORIENTED_EDGE ( 'NONE', *, *, #5814, .T. ) ;
#15289 = CARTESIAN_POINT ( 'NONE',  ( 0.000000000000000000, 0.000000000000000000, -18.00000000000000000 ) ) ;
#15290 = CARTESIAN_POINT ( 'NONE',  ( -15.79999999999999538, 1.934941942652817234E-15, -1.540456584061364431 ) ) ;
#15291 = CARTESIAN_POINT ( 'NONE',  ( -0.05014649552828365914, 215.4116977939061144, 30.24886208192143755 ) ) ;
#15292 = CARTESIAN_POINT ( 'NONE',  ( -3.135527875058821579, 197.5041725223112223, 71.90113791807857524 ) ) ;
#15293 = FACE_OUTER_BOUND ( 'NONE', #22138, .T. ) ;
#15294 = EDGE_CURVE ( 'NONE', #16034, #14731, #15395, .T. ) ;
#15295 = CARTESIAN_POINT ( 'NONE',  ( 3.135527875058820690, 216.4958274776887492, 52.40113791807857524 ) ) ;
#15296 =( REPRESENTATION_RELATIONSHIP ('NONE','NONE', #25663, #13706 ) REPRESENTATION_RELATIONSHIP_WITH_TRANSFORMATION ( #21454 )SHAPE_REPRESENTATION_RELATIONSHIP( ) );
#15297 = ITEM_DEFINED_TRANSFORMATION ( 'NONE', 'NONE', #4482,  #2404 ) ;
#15298 = CARTESIAN_POINT ( 'NONE',  ( -6.139770520408369237, 215.5359834540460042, 24.95113791807855819 ) ) ;
#15299 = CARTESIAN_POINT ( 'NONE',  ( 4.903702542908601636, 200.1653181626581102, 8.451137918078563516 ) ) ;
#15300 = DIRECTION ( 'NONE',  ( 1.000000000000000000, -0.000000000000000000, -0.000000000000000000 ) ) ;
#15301 = CARTESIAN_POINT ( 'NONE',  ( -64.50000000000000000, 2.605762844159070557, 20.00000000000000000 ) ) ;
#15302 = CARTESIAN_POINT ( 'NONE',  ( 35.62499999726881583, 171.3844434931184253, -7.942151717890134290E-15 ) ) ;
#15303 = CARTESIAN_POINT ( 'NONE',  ( 7.456977232089302632, 217.1783343296989131, 34.55113791807856671 ) ) ;
#15304 = DIRECTION ( 'NONE',  ( 0.000000000000000000, 0.000000000000000000, -1.000000000000000000 ) ) ;
#15305 = CARTESIAN_POINT ( 'NONE',  ( -6.139770520408369237, 215.5359834540460042, 84.95113791807858661 ) ) ;
#15306 = CARTESIAN_POINT ( 'NONE',  ( 8.062137200540920645, 201.0835637161417822, 62.30113791807858092 ) ) ;
#15307 = DIRECTION ( 'NONE',  ( 1.000000000000000000, 0.000000000000000000, 0.000000000000000000 ) ) ;
#15308 = CARTESIAN_POINT ( 'NONE',  ( 0.05014649552828288198, 194.3824533091408000, 13.74886208192143577 ) ) ;
#15309 = CARTESIAN_POINT ( 'NONE',  ( 10.01549611932659367, 203.7984951890124421, 25.14886208192143613 ) ) ;
#15310 = VECTOR ( 'NONE', #6836, 1000.000000000000000 ) ;
#15311 = CARTESIAN_POINT ( 'NONE',  ( 74.99999999453763166, 155.0000000000000000, 14.49999999999999467 ) ) ;
#15312 = VERTEX_POINT ( 'NONE', #25992 ) ;
#15313 = CARTESIAN_POINT ( 'NONE',  ( 0.05014649552807549926, 219.6175466908591716, 70.25113791807856956 ) ) ;
#15314 = CARTESIAN_POINT ( 'NONE',  ( -4.903702542908602524, 213.8346818373418898, 78.95113791807858661 ) ) ;
#15315 = CARTESIAN_POINT ( 'NONE',  ( 9.984503880673420539, 210.2968891136705167, 42.84886208192143897 ) ) ;
#15316 = DIRECTION ( 'NONE',  ( 1.000000000000000000, 0.000000000000000000, -0.000000000000000000 ) ) ;
#15317 = EDGE_LOOP ( 'NONE', ( #5102, #17532, #12838, #4566 ) ) ;
#15318 = CARTESIAN_POINT ( 'NONE',  ( 12.01549611932659367, 203.1486557965466773, 40.14886208192143613 ) ) ;
#15319 = ORIENTED_EDGE ( 'NONE', *, *, #18337, .T. ) ;
#15320 = ORIENTED_EDGE ( 'NONE', *, *, #31577, .T. ) ;
#15321 = DIRECTION ( 'NONE',  ( 1.000000000000000000, 0.000000000000000000, 0.000000000000000000 ) ) ;
#15322 = DIRECTION ( 'NONE',  ( -0.7071067811865314745, 8.659560562355128841E-17, -0.7071067811865635599 ) ) ;
#15323 = ORIENTED_EDGE ( 'NONE', *, *, #26257, .F. ) ;
#15324 =( BOUNDED_CURVE ( )  B_SPLINE_CURVE ( 2, ( #11769, #31717, #3428, #13991, #31878, #19106, #8389, #24387, #9045, #29841, #13824 ),
 .UNSPECIFIED., .F., .T. ) 
 B_SPLINE_CURVE_WITH_KNOTS ( ( 3, 2, 2, 2, 2, 3 ),
 ( 0.7142857142857140795, 0.7178571428571426383, 0.7214285714285711970, 0.7249999999999998668, 0.7285714285714284255, 0.7321428571428569843 ),
 .UNSPECIFIED. ) 
 CURVE ( )  GEOMETRIC_REPRESENTATION_ITEM ( )  RATIONAL_B_SPLINE_CURVE ( ( 1.000000000000001554, 0.9510565162951518658, 1.000000000000000000, 0.9510565162951534202, 1.000000000000000000, 0.9510565162951534202, 1.000000000000000000, 0.9510565162951534202, 1.000000000000000000, 0.9510565162951549745, 0.9999999999999984457 ) ) 
 REPRESENTATION_ITEM ( '' )  );
#15325 = CARTESIAN_POINT ( 'NONE',  ( 8.000000000000008882, 206.9523078486586485, 41.00113791807857666 ) ) ;
#15326 = CARTESIAN_POINT ( 'NONE',  ( 3.250000000000004441, 5.629165124598849879, 0.000000000000000000 ) ) ;
#15327 = CARTESIAN_POINT ( 'NONE',  ( 3.044812012439969795, 216.5253028482143520, 27.39886208192143613 ) ) ;
#15328 = CARTESIAN_POINT ( 'NONE',  ( 57.97499999726881015, 169.8198683612136222, 4.815267126137181997 ) ) ;
#15329 = ORIENTED_EDGE ( 'NONE', *, *, #6602, .T. ) ;
#15330 = CARTESIAN_POINT ( 'NONE',  ( -8.000000000000008882, 207.0476921513413515, 57.50113791807857666 ) ) ;
#15331 = LINE ( 'NONE', #28622, #33596 ) ;
#15332 = VECTOR ( 'NONE', #20792, 1000.000000000000000 ) ;
#15333 = B_SPLINE_CURVE_WITH_KNOTS ( 'NONE', 3,
 ( #16018, #18907, #16511, #350, #8843, #16342, #26736, #21130 ),
 .UNSPECIFIED., .F., .F.,
 ( 4, 2, 2, 4 ),
 ( 0.006061689441712453386, 0.007174127271521677299, 0.008286565101330901212, 0.01051144076094934904 ),
 .UNSPECIFIED. ) ;
#15334 = DIRECTION ( 'NONE',  ( 1.000000000000000000, 0.000000000000000000, 0.000000000000000000 ) ) ;
#15335 = CARTESIAN_POINT ( 'NONE',  ( -6.139770520408224463, 198.4640165459539389, 98.04886208192141339 ) ) ;
#15336 = CARTESIAN_POINT ( 'NONE',  ( -3.044812012440131443, 216.5253028482142952, 43.10113791807857808 ) ) ;
#15337 = SURFACE_SIDE_STYLE ('',( #26075 ) ) ;
#15338 = EDGE_CURVE ( 'NONE', #18219, #28735, #10904, .T. ) ;
#15339 = CARTESIAN_POINT ( 'NONE',  ( -6.220909254589537696, 198.5229672870051161, 24.05113791807855961 ) ) ;
#15340 = CARTESIAN_POINT ( 'NONE',  ( 0.000000000000000000, 0.000000000000000000, -9.999999999999998224 ) ) ;
#15341 =( LENGTH_UNIT ( ) NAMED_UNIT ( * ) SI_UNIT ( .MILLI., .METRE. ) );
#15342 = CARTESIAN_POINT ( 'NONE',  ( -2.426778023690076225, 199.3768101843759553, 82.89886208192143613 ) ) ;
#15343 = CIRCLE ( 'NONE', #28935, 4.000000000000000888 ) ;
#15344 = CARTESIAN_POINT ( 'NONE',  ( 86.90000000000000568, 168.7903194862797420, -4.480746418436745593 ) ) ;
#15345 =( LENGTH_UNIT ( ) NAMED_UNIT ( * ) SI_UNIT ( .MILLI., .METRE. ) );
#15346 = CARTESIAN_POINT ( 'NONE',  ( -4.174999999999999822, 5.112900386440199535E-16, -0.5776712190230133270 ) ) ;
#15347 = CARTESIAN_POINT ( 'NONE',  ( 12.00000000000000711, 206.9523078486586485, 5.001137918078565114 ) ) ;
#15348 = EDGE_CURVE ( 'NONE', #28367, #20140, #17113, .T. ) ;
#15349 = CARTESIAN_POINT ( 'NONE',  ( 48.28867513459482552, 139.2280666364260071, -4.041636747397287284E-15 ) ) ;
#15350 = CARTESIAN_POINT ( 'NONE',  ( 48.57499999726881157, 145.8408176439707802, 12.60653300113718345 ) ) ;
#15351 = CARTESIAN_POINT ( 'NONE',  ( 6.220909254589536808, 215.4770327129947702, 58.55113791807858092 ) ) ;
#15352 = CARTESIAN_POINT ( 'NONE',  ( 125.5000000000000000, 155.0000000000010800, 106.0000000000000142 ) ) ;
#15353 = EDGE_CURVE ( 'NONE', #2045, #10532, #4499, .T. ) ;
#15354 = CARTESIAN_POINT ( 'NONE',  ( 103.4083388212532810, 155.0000000000000000, 32.00000000000002842 ) ) ;
#15355 = CARTESIAN_POINT ( 'NONE',  ( -3.135527875058982783, 216.4958274776886924, 3.098862081921434974 ) ) ;
#15356 = CARTESIAN_POINT ( 'NONE',  ( 51.19999999453762740, 146.4771138417591203, 11.73074641843673227 ) ) ;
#15357 = ORIENTED_EDGE ( 'NONE', *, *, #8546, .F. ) ;
#15358 = CARTESIAN_POINT ( 'NONE',  ( -12.01549611932652972, 203.1486557965464499, 27.35113791807856742 ) ) ;
#15359 = CARTESIAN_POINT ( 'NONE',  ( 46.71132485994281325, 155.0000000000000000, 15.00000000000001243 ) ) ;
#15360 = CARTESIAN_POINT ( 'NONE',  ( 3.044812012439969795, 216.5253028482143520, 15.39886208192143613 ) ) ;
#15361 = VERTEX_POINT ( 'NONE', #19496 ) ;
#15362 = COLOUR_RGB ( '', 0.31764706, 0.68627451, 0.89019608) ;
#15363 = CARTESIAN_POINT ( 'NONE',  ( -10.00000000000000711, 207.0476921513413515, 12.50113791807856778 ) ) ;
#15364 = CARTESIAN_POINT ( 'NONE',  ( -10.00000000000000711, 207.0476921513413515, 72.50113791807858377 ) ) ;
#15365 = EDGE_CURVE ( 'NONE', #9072, #13192, #13750, .T. ) ;
#15366 = VERTEX_POINT ( 'NONE', #19665 ) ;
#15367 = CARTESIAN_POINT ( 'NONE',  ( 6.500168698208244500, 202.3363017425938324, 31.29886208192143826 ) ) ;
#15368 = CARTESIAN_POINT ( 'NONE',  ( 12.58016597185466168, -24.49110259512899290, -17.98559444045774569 ) ) ;
#15369 = ORIENTED_EDGE ( 'NONE', *, *, #31855, .T. ) ;
#15370 = CARTESIAN_POINT ( 'NONE',  ( -8.015496119326531499, 204.4483345814780364, 3.351137918078566535 ) ) ;
#15371 = ADVANCED_FACE ( 'NONE', ( #30568 ), #30056, .F. ) ;
#15372 = VECTOR ( 'NONE', #6728, 1000.000000000000000 ) ;
#15373 = CARTESIAN_POINT ( 'NONE',  ( 12.00000000000000711, 207.0476921513415220, 84.99886208192144466 ) ) ;
#15374 = CARTESIAN_POINT ( 'NONE',  ( 38.87499999726880873, 138.6155565068815747, -3.929120461958505118E-15 ) ) ;
#15375 = VERTEX_POINT ( 'NONE', #32607 ) ;
#15376 = CARTESIAN_POINT ( 'NONE',  ( 45.42499999726879878, 168.2552932293087906, -9.630534252274385310 ) ) ;
#15377 = CARTESIAN_POINT ( 'NONE',  ( 120.4126214611401480, 2.643999646947254423, 35.00001199999999812 ) ) ;
#15378 = CARTESIAN_POINT ( 'NONE',  ( -10.01549611932653860, 203.7984951890123284, 6.351137918078566535 ) ) ;
#15379 = CARTESIAN_POINT ( 'NONE',  ( -0.05014649552828403384, 217.5146222423826714, 69.24886208192144466 ) ) ;
#15380 = CARTESIAN_POINT ( 'NONE',  ( 48.27499999726880731, 160.0630714827496206, 15.58253174999999402 ) ) ;
#15381 = CARTESIAN_POINT ( 'NONE',  ( -67.50001199999998391, 152.7747327161067403, 16.89041650604971068 ) ) ;
#15382 = CARTESIAN_POINT ( 'NONE',  ( -10.00000000000000711, 207.0476921513413515, 9.501137918078566003 ) ) ;
#15383 = CARTESIAN_POINT ( 'NONE',  ( 44.68867513459483121, 150.1262045565065364, -15.00000000000012434 ) ) ;
#15384 = AXIS2_PLACEMENT_3D ( 'NONE', #11153, #25228, #12279 ) ;
#15385 = CARTESIAN_POINT ( 'NONE',  ( 68.20000000000001705, 142.6655632788954620, -8.961492836873480528 ) ) ;
#15386 = CARTESIAN_POINT ( 'NONE',  ( 6.139770520408368348, 198.4640165459539674, 101.4511379180785866 ) ) ;
#15387 = CARTESIAN_POINT ( 'NONE',  ( 14.33345751131668599, 23.47883925285266926, 5.014435047745465896E-16 ) ) ;
#15388 = CARTESIAN_POINT ( 'NONE',  ( -0.05014649552810635652, 196.4853777576173002, 71.75113791807858377 ) ) ;
#15389 = CARTESIAN_POINT ( 'NONE',  ( 57.78867513459481842, 155.0000000000000000, 15.00000000000001243 ) ) ;
#15390 = CARTESIAN_POINT ( 'NONE',  ( 34.27499999726880731, 160.0630714827496206, 15.58253174999999402 ) ) ;
#15391 = CARTESIAN_POINT ( 'NONE',  ( -0.05014649552828442242, 219.6175466908591716, 90.24886208192144466 ) ) ;
#15392 = CARTESIAN_POINT ( 'NONE',  ( 73.62499999726883004, 171.3844434931184253, -7.942151717890132712E-15 ) ) ;
#15393 = ORIENTED_EDGE ( 'NONE', *, *, #2722, .F. ) ;
#15394 = CARTESIAN_POINT ( 'NONE',  ( -60.02503143742045921, 194.9506873066471542, -1.987662087495396301 ) ) ;
#15395 = CIRCLE ( 'NONE', #14850, 13.00000000000001066 ) ;
#15396 = CARTESIAN_POINT ( 'NONE',  ( 36.59999999453762598, 168.7903194862797420, 4.480746418436729606 ) ) ;
#15397 = CARTESIAN_POINT ( 'NONE',  ( -7.375838497908182134, 217.2372850707499765, 99.95113791807860082 ) ) ;
#15398 = CONICAL_SURFACE ( 'NONE', #701, 12.00000000000001066, 0.1047197551196740739 ) ;
#15399 = EDGE_CURVE ( 'NONE', #26702, #21673, #22561, .T. ) ;
#15400 = CARTESIAN_POINT ( 'NONE',  ( -11.00000000000000711, 206.8801259629684921, 103.6040119011138358 ) ) ;
#15401 = ORIENTED_EDGE ( 'NONE', *, *, #23707, .T. ) ;
#15402 = CARTESIAN_POINT ( 'NONE',  ( -3.135527875058982783, 216.4958274776886924, 84.09886208192143897 ) ) ;
#15403 = CARTESIAN_POINT ( 'NONE',  ( 9.680171189290716072, 214.0920067884432854, 18.69886208192143684 ) ) ;
#15404 = CARTESIAN_POINT ( 'NONE',  ( 5.000000000000000000, 2.342598717236900718, -4.057500000000001883 ) ) ;
#15405 = CARTESIAN_POINT ( 'NONE',  ( 9.984503880673470277, 203.7031108863295401, 44.15113791807856813 ) ) ;
#15406 = ORIENTED_EDGE ( 'NONE', *, *, #9090, .F. ) ;
#15407 = EDGE_CURVE ( 'NONE', #7020, #30153, #28986, .T. ) ;
#15408 = CARTESIAN_POINT ( 'NONE',  ( -3.135527875058982783, 216.4958274776886924, 96.09886208192143897 ) ) ;
#15409 = VECTOR ( 'NONE', #26185, 1000.000000000000000 ) ;
#15410 = CARTESIAN_POINT ( 'NONE',  ( 107.5000000000000000, 155.0000000000000000, 100.0000000000000000 ) ) ;
#15411 = ORIENTED_EDGE ( 'NONE', *, *, #1054, .F. ) ;
#15412 = CARTESIAN_POINT ( 'NONE',  ( 4.903702542908435547, 213.8346818373419751, 81.54886208192144181 ) ) ;
#15413 = EDGE_CURVE ( 'NONE', #19088, #3486, #1606, .T. ) ;
#15414 = ORIENTED_EDGE ( 'NONE', *, *, #9678, .F. ) ;
#15415 = CARTESIAN_POINT ( 'NONE',  ( 34.11132485994280472, 169.2658477444273331, -4.635254915624224203 ) ) ;
#15416 = ORIENTED_EDGE ( 'NONE', *, *, #4558, .F. ) ;
#15417 = LINE ( 'NONE', #7417, #24319 ) ;
#15418 = CARTESIAN_POINT ( 'NONE',  ( 2.517493886308900919, 214.5937144450984420, 58.40113791807858235 ) ) ;
#15419 = VECTOR ( 'NONE', #9755, 1000.000000000000000 ) ;
#15420 = CARTESIAN_POINT ( 'NONE',  ( 85.52499999726880731, 169.8198683612136222, -4.815267126137197984 ) ) ;
#15421 = FACE_OUTER_BOUND ( 'NONE', #1073, .T. ) ;
#15422 = CARTESIAN_POINT ( 'NONE',  ( 4.984841277089725686, 213.7757310962907411, 85.55113791807858092 ) ) ;
#15423 = CARTESIAN_POINT ( 'NONE',  ( 77.50000000000000000, 155.0000000000000000, -6.938893903907228378E-15 ) ) ;
#15424 = SHAPE_REPRESENTATION_RELATIONSHIP ( 'NONE' , 'NONE' ,  #1289, #1878 ) ;
#15425 = CARTESIAN_POINT ( 'NONE',  ( 49.60000000000000853, 150.2886644046228639, 14.49999999999999645 ) ) ;
#15426 = CARTESIAN_POINT ( 'NONE',  ( -6.444103211790928043, 202.2591342207265939, 65.19886208192143329 ) ) ;
#15427 = DIRECTION ( 'NONE',  ( 0.000000000000000000, -0.000000000000000000, -1.000000000000000000 ) ) ;
#15428 = CARTESIAN_POINT ( 'NONE',  ( 53.62499999726881583, 171.3844434931184253, -7.942151717890132712E-15 ) ) ;
#15429 = AXIS2_PLACEMENT_3D ( 'NONE', #22579, #9810, #11689 ) ;
#15430 = CARTESIAN_POINT ( 'NONE',  ( 8.118202686958039038, 212.8392687619912635, 1.701137918078565736 ) ) ;
#15431 = CARTESIAN_POINT ( 'NONE',  ( 8.640141755188686545, 206.6086104956403915, 111.6972426105882477 ) ) ;
#15432 = CARTESIAN_POINT ( 'NONE',  ( 59.32499999726881157, 164.1591823560292198, -12.60653300113719766 ) ) ;
#15433 = CARTESIAN_POINT ( 'NONE',  ( 72.27499999726879309, 160.0630714827496206, 15.58253174999999402 ) ) ;
#15434 = CARTESIAN_POINT ( 'NONE',  ( 9.680171189290831535, 199.9079932115568852, 68.30113791807856671 ) ) ;
#15435 = CARTESIAN_POINT ( 'NONE',  ( 46.51132485994280330, 163.8167787843871110, 12.13525491562421621 ) ) ;
#15436 = PRODUCT_DEFINITION_SHAPE ( 'NONE', 'NONE',  #33689 ) ;
#15437 = CARTESIAN_POINT ( 'NONE',  ( 3.662846001190051659, 195.5725841191953691, 14.60113791807856742 ) ) ;
#15438 = EDGE_CURVE ( 'NONE', #23382, #17270, #31704, .T. ) ;
#15439 = CARTESIAN_POINT ( 'NONE',  ( -0.05014649552810635652, 196.4853777576173002, 89.75113791807856956 ) ) ;
#15440 = CARTESIAN_POINT ( 'NONE',  ( -7.375838497908014268, 196.7627149292498530, 50.04886208192142760 ) ) ;
#15441 = CARTESIAN_POINT ( 'NONE',  ( -10.01549611932659545, 210.2015048109875011, 56.64886208192143613 ) ) ;
#15442 = DIRECTION ( 'NONE',  ( 1.000000000000000000, 0.000000000000000000, 0.000000000000000000 ) ) ;
#15443 = CARTESIAN_POINT ( 'NONE',  ( -11.98450388067348804, 210.9467285061362247, 93.65113791807857524 ) ) ;
#15444 = CARTESIAN_POINT ( 'NONE',  ( -67.50001199999999812, 171.8904165060497178, -2.225267283893245907 ) ) ;
#15445 = CARTESIAN_POINT ( 'NONE',  ( 0.05014649552810505201, 217.5146222423826714, 16.25113791807856600 ) ) ;
#15446 = CIRCLE ( 'NONE', #233, 7.500000000000001776 ) ;
#15447 = EDGE_CURVE ( 'NONE', #24401, #18472, #11103, .T. ) ;
#15448 = CARTESIAN_POINT ( 'NONE',  ( -8.118202686958138514, 212.8392687619910930, 71.79886208192142760 ) ) ;
#15449 = AXIS2_PLACEMENT_3D ( 'NONE', #5635, #26742, #16348 ) ;
#15450 = EDGE_LOOP ( 'NONE', ( #16684, #30451, #30377, #1455 ) ) ;
#15451 = CARTESIAN_POINT ( 'NONE',  ( -12.01549611932659722, 210.8513442034533227, 80.64886208192145034 ) ) ;
#15452 = CARTESIAN_POINT ( 'NONE',  ( 10.01549611932653860, 210.2015048109876716, 88.85113791807857808 ) ) ;
#15453 = ORIENTED_EDGE ( 'NONE', *, *, #19475, .T. ) ;
#15454 = CARTESIAN_POINT ( 'NONE',  ( 78.47499999726881015, 149.9369285172503510, 15.58253174999999580 ) ) ;
#15455 = CARTESIAN_POINT ( 'NONE',  ( -8.000000000000008882, 206.9523078486584780, 47.49886208192144466 ) ) ;
#15456 = ORIENTED_EDGE ( 'NONE', *, *, #29333, .F. ) ;
#15457 = CARTESIAN_POINT ( 'NONE',  ( 74.32499999726881867, 145.8408176439707802, 12.60653300113718345 ) ) ;
#15458 = CARTESIAN_POINT ( 'NONE',  ( 6.500000000000000888, -2.759515168581564204, -5.880113447610522570 ) ) ;
#15459 = PRESENTATION_LAYER_ASSIGNMENT (  '', '', ( #13819 ) ) ;
#15460 = LINE ( 'NONE', #15114, #19207 ) ;
#15461 = CARTESIAN_POINT ( 'NONE',  ( 63.12499999726880873, 155.0000000000000000, -15.58253175000000823 ) ) ;
#15462 = CARTESIAN_POINT ( 'NONE',  ( -54.75000000000000711, -7.347880794884118356E-15, -20.00000000000000355 ) ) ;
#15463 = CARTESIAN_POINT ( 'NONE',  ( -10.01549611932659722, 210.2015048109875011, 53.64886208192141481 ) ) ;
#15464 = EDGE_LOOP ( 'NONE', ( #9618, #924 ) ) ;
#15465 = DIRECTION ( 'NONE',  ( 1.000000000000000000, 0.000000000000000000, 0.000000000000000000 ) ) ;
#15466 = CIRCLE ( 'NONE', #26883, 27.99999999999999645 ) ;
#15467 = SURFACE_SIDE_STYLE ('',( #17681 ) ) ;
#15468 = DIRECTION ( 'NONE',  ( 1.000000000000000000, -0.000000000000000000, -0.000000000000000000 ) ) ;
#15469 = CARTESIAN_POINT ( 'NONE',  ( 2.426778023690075337, 214.6231898156240447, 30.39886208192143613 ) ) ;
#15470 = CIRCLE ( 'NONE', #16551, 2.500000000000000000 ) ;
#15471 = CARTESIAN_POINT ( 'NONE',  ( 10.01549611932653860, 210.2015048109876716, 73.85113791807857808 ) ) ;
#15472 = FACE_OUTER_BOUND ( 'NONE', #28776, .T. ) ;
#15473 = CARTESIAN_POINT ( 'NONE',  ( -8.062137200540920645, 212.9164362838581894, 60.80113791807857382 ) ) ;
#15474 = CARTESIAN_POINT ( 'NONE',  ( -6.220909254589537696, 198.5229672870051161, 24.05113791807855961 ) ) ;
#15475 = CARTESIAN_POINT ( 'NONE',  ( 0.05014649552807626948, 215.4116977939061144, 16.25113791807856600 ) ) ;
#15476 = CARTESIAN_POINT ( 'NONE',  ( 86.67499999726879878, 141.7447067706911810, 9.630534252274376428 ) ) ;
#15477 = CYLINDRICAL_SURFACE ( 'NONE', #5682, 5.250000000000004441 ) ;
#15478 = CARTESIAN_POINT ( 'NONE',  ( 37.72499999726881015, 169.8198683612136222, 4.815267126137181997 ) ) ;
#15479 = CARTESIAN_POINT ( 'NONE',  ( 0.05014649552807549926, 219.6175466908591716, 37.25113791807857666 ) ) ;
#15480 = CARTESIAN_POINT ( 'NONE',  ( 3.983107665916332252, -5.570601890521292177, -6.171481112545254000 ) ) ;
#15481 = CARTESIAN_POINT ( 'NONE',  ( 3.135527875058820690, 216.4958274776887492, 85.40113791807857524 ) ) ;
#15482 = CARTESIAN_POINT ( 'NONE',  ( -9.984503880673475606, 210.2968891136704315, 63.65113791807856813 ) ) ;
#15483 = FACE_OUTER_BOUND ( 'NONE', #11992, .T. ) ;
#15484 = STYLED_ITEM ( 'NONE', ( #1666 ), #21009 ) ;
#15485 = CARTESIAN_POINT ( 'NONE',  ( -11.98450388067341876, 203.0532714938636047, 20.34886208192143542 ) ) ;
#15486 = CARTESIAN_POINT ( 'NONE',  ( -10.01549611932659545, 210.2015048109875011, 29.64886208192143968 ) ) ;
#15487 = CARTESIAN_POINT ( 'NONE',  ( 75.99999999453763166, 155.0000000000000000, -14.50000000000000711 ) ) ;
#15488 = CARTESIAN_POINT ( 'NONE',  ( 7.456977232089302632, 217.1783343296989131, 64.55113791807856671 ) ) ;
#15489 = CARTESIAN_POINT ( 'NONE',  ( 7.984503880673485376, 204.3529502787953902, 77.15113791807857524 ) ) ;
#15490 = CARTESIAN_POINT ( 'NONE',  ( 10.00000000000000711, 207.0476921513415220, 39.99886208192143755 ) ) ;
#15491 = LINE ( 'NONE', #25882, #8019 ) ;
#15492 = ORIENTED_EDGE ( 'NONE', *, *, #13098, .T. ) ;
#15493 = CARTESIAN_POINT ( 'NONE',  ( -0.05014649552828442242, 219.6175466908591716, 54.24886208192143755 ) ) ;
#15494 = ORIENTED_EDGE ( 'NONE', *, *, #20197, .F. ) ;
#15495 = VERTEX_POINT ( 'NONE', #17445 ) ;
#15496 = CARTESIAN_POINT ( 'NONE',  ( 10.00000000000000178, 6.613092715395708453E-16, 5.400000000000002132 ) ) ;
#15497 = CARTESIAN_POINT ( 'NONE',  ( -64.50000000000000000, 155.0000000000000000, -40.00000000000000000 ) ) ;
#15498 = EDGE_LOOP ( 'NONE', ( #19419, #21337, #12486, #26624 ) ) ;
#15499 = CARTESIAN_POINT ( 'NONE',  ( 6.444103211791042618, 202.2591342207267644, 41.30113791807857382 ) ) ;
#15500 = FILL_AREA_STYLE_COLOUR ( '', #8001 ) ;
#15501 = APPLICATION_CONTEXT ( 'automotive_design' ) ;
#15502 = CARTESIAN_POINT ( 'NONE',  ( 10.01549611932659545, 203.7984951890123853, 22.14886208192143613 ) ) ;
#15503 = CARTESIAN_POINT ( 'NONE',  ( 62.27499999726880020, 160.0630714827496206, 15.58253174999999224 ) ) ;
#15504 = ORIENTED_EDGE ( 'NONE', *, *, #24130, .T. ) ;
#15505 = CARTESIAN_POINT ( 'NONE',  ( -6.938893903907228378E-15, 31.75426480542944319, -18.00000000000000000 ) ) ;
#15506 = CARTESIAN_POINT ( 'NONE',  ( 0.000000000000000000, 0.000000000000000000, -0.5776712190230133270 ) ) ;
#15507 = CARTESIAN_POINT ( 'NONE',  ( -0.05014649552828365914, 215.4116977939061144, 6.248862081921434886 ) ) ;
#15508 = CARTESIAN_POINT ( 'NONE',  ( 9.984503880673470277, 203.7031108863295401, 44.15113791807856813 ) ) ;
#15509 = CARTESIAN_POINT ( 'NONE',  ( 0.05014649552810505201, 217.5146222423826714, 25.25113791807856245 ) ) ;
#15510 = FACE_OUTER_BOUND ( 'NONE', #5974, .T. ) ;
#15511 = CARTESIAN_POINT ( 'NONE',  ( -0.05014649552828365914, 215.4116977939061144, 96.24886208192144466 ) ) ;
#15512 = CARTESIAN_POINT ( 'NONE',  ( 85.29999999999999716, 163.5228861582408797, 11.73074641843673049 ) ) ;
#15513 =( NAMED_UNIT ( * ) PLANE_ANGLE_UNIT ( ) SI_UNIT ( $, .RADIAN. ) );
#15514 = DIRECTION ( 'NONE',  ( -1.000000000000000000, -0.000000000000000000, -0.000000000000000000 ) ) ;
#15515 = CARTESIAN_POINT ( 'NONE',  ( -7.456977232089304408, 196.8216656703010301, 9.051137918078564937 ) ) ;
#15516 = CYLINDRICAL_SURFACE ( 'NONE', #21098, 40.00000000000000711 ) ;
#15517 = CARTESIAN_POINT ( 'NONE',  ( 53.47499999726881015, 160.0630714827496206, -15.58253175000000823 ) ) ;
#15518 = CARTESIAN_POINT ( 'NONE',  ( 8.062137200540920645, 201.0835637161417822, 53.30113791807857382 ) ) ;
#15519 = CARTESIAN_POINT ( 'NONE',  ( 35.51132485994281041, 146.1832212156128890, -12.13525491562423042 ) ) ;
#15520 = CARTESIAN_POINT ( 'NONE',  ( 97.20416941062678973, 155.0000000000000000, 0.000000000000000000 ) ) ;
#15521 = CARTESIAN_POINT ( 'NONE',  ( -67.50000599999999906, 155.0000000000000000, 17.00000000000001421 ) ) ;
#15522 = CARTESIAN_POINT ( 'NONE',  ( 54.59999999453762598, 168.7903194862797420, 4.480746418436729606 ) ) ;
#15523 = ORIENTED_EDGE ( 'NONE', *, *, #24130, .F. ) ;
#15524 = CARTESIAN_POINT ( 'NONE',  ( 12.00000000000000711, 206.9523078486586485, 41.00113791807856245 ) ) ;
#15525 = CARTESIAN_POINT ( 'NONE',  ( 47.61132485994280472, 150.1262045565063659, -14.99999999999998046 ) ) ;
#15526 = CARTESIAN_POINT ( 'NONE',  ( 0.05014649552828275708, 196.4853777576173002, 16.74886208192143755 ) ) ;
#15527 = DIRECTION ( 'NONE',  ( 0.000000000000000000, -1.000000000000000000, 1.290957005378097920E-14 ) ) ;
#15528 = VERTEX_POINT ( 'NONE', #4154 ) ;
#15529 =( BOUNDED_CURVE ( )  B_SPLINE_CURVE ( 2, ( #27901, #2527, #12911, #20745, #31141, #25347, #30640, #9856, #7807, #18199, #137 ),
 .UNSPECIFIED., .F., .F. ) 
 B_SPLINE_CURVE_WITH_KNOTS ( ( 3, 2, 2, 2, 2, 3 ),
 ( 0.7499999999999997780, 0.7535714285714283367, 0.7571428571428568954, 0.7607142857142855652, 0.7642857142857141239, 0.7678571428571426827 ),
 .UNSPECIFIED. ) 
 CURVE ( )  GEOMETRIC_REPRESENTATION_ITEM ( )  RATIONAL_B_SPLINE_CURVE ( ( 1.000000000000003109, 0.9510565162951504226, 1.000000000000000000, 0.9510565162951534202, 1.000000000000000000, 0.9510565162951534202, 1.000000000000000000, 0.9510565162951534202, 1.000000000000000000, 0.9510565162951549745, 0.9999999999999984457 ) ) 
 REPRESENTATION_ITEM ( '' )  );
#15530 = CARTESIAN_POINT ( 'NONE',  ( 8.118202686958039038, 212.8392687619912635, 7.701137918078566180 ) ) ;
#15531 = CARTESIAN_POINT ( 'NONE',  ( -3.044812012440131443, 216.5253028482142952, 67.10113791807857808 ) ) ;
#15532 = ORIENTED_EDGE ( 'NONE', *, *, #29970, .F. ) ;
#15533 = CARTESIAN_POINT ( 'NONE',  ( -4.984841277089891776, 213.7757310962905990, 29.94886208192143684 ) ) ;
#15534 = B_SPLINE_CURVE_WITH_KNOTS ( 'NONE', 3,
 ( #1401, #3792, #11631, #14352 ),
 .UNSPECIFIED., .F., .F.,
 ( 4, 4 ),
 ( 0.000000000000000000, 0.004600009204204579850 ),
 .UNSPECIFIED. ) ;
#15535 = EDGE_CURVE ( 'NONE', #8952, #8613, #698, .T. ) ;
#15536 = VERTEX_POINT ( 'NONE', #1272 ) ;
#15537 = CARTESIAN_POINT ( 'NONE',  ( -6.500168698208129925, 202.3363017425936050, 9.201137918078563516 ) ) ;
#15538 = CARTESIAN_POINT ( 'NONE',  ( 9.680171189290716072, 214.0920067884432854, 102.6988620819214475 ) ) ;
#15539 = CARTESIAN_POINT ( 'NONE',  ( 43.87499999726880873, 171.3844434931184253, -7.942151717890134290E-15 ) ) ;
#15540 = ORIENTED_EDGE ( 'NONE', *, *, #11204, .T. ) ;
#15541 = CARTESIAN_POINT ( 'NONE',  ( 51.82499999726881157, 168.2552932293087906, 9.630534252274372875 ) ) ;
#15542 = CARTESIAN_POINT ( 'NONE',  ( 130.2500000000000284, 0.6872233929727983304, 35.00001200000000523 ) ) ;
#15543 = CARTESIAN_POINT ( 'NONE',  ( 3.044812012440130555, 197.4746971517856764, 11.60113791807856742 ) ) ;
#15544 = CARTESIAN_POINT ( 'NONE',  ( -3.044812012439970683, 197.4746971517856196, 82.89886208192145034 ) ) ;
#15545 = CARTESIAN_POINT ( 'NONE',  ( 45.77499999726881441, 169.8198683612136222, -4.815267126137197984 ) ) ;
#15546 = CARTESIAN_POINT ( 'NONE',  ( 79.21132485994282035, 139.2280666364260071, -4.041636747397287284E-15 ) ) ;
#15547 = CARTESIAN_POINT ( 'NONE',  ( -6.139770520408369237, 215.5359834540460042, 12.95113791807856352 ) ) ;
#15548 = DIRECTION ( 'NONE',  ( 1.000000000000000000, 0.000000000000000000, 0.000000000000000000 ) ) ;
#15549 = CARTESIAN_POINT ( 'NONE',  ( 70.20000000000001705, 142.6655632788954620, -8.961492836873480528 ) ) ;
#15550 = CARTESIAN_POINT ( 'NONE',  ( 6.220909254589536808, 215.4770327129947702, 97.55113791807855250 ) ) ;
#15551 = CARTESIAN_POINT ( 'NONE',  ( 19.55945325266599966, 20.46160920480079781, -0.4491195576436673997 ) ) ;
#15552 = CARTESIAN_POINT ( 'NONE',  ( -3.135527875058821579, 197.5041725223112223, 80.90113791807858945 ) ) ;
#15553 = LINE ( 'NONE', #64, #6379 ) ;
#15554 = CARTESIAN_POINT ( 'NONE',  ( 3.662846001189864698, 218.4274158808046593, 96.39886208192146455 ) ) ;
#15555 = CARTESIAN_POINT ( 'NONE',  ( 73.12499999726881583, 155.0000000000000000, -15.58253175000000823 ) ) ;
#15556 = ORIENTED_EDGE ( 'NONE', *, *, #18522, .T. ) ;
#15557 = CARTESIAN_POINT ( 'NONE',  ( -60.66914996032592455, 194.9805833264304908, -1.253524243223063994 ) ) ;
#15558 = CARTESIAN_POINT ( 'NONE',  ( 37.49999999453762456, 139.7537977485451393, -4.138211985947621020E-15 ) ) ;
#15559 = CARTESIAN_POINT ( 'NONE',  ( -7.456977232089304408, 196.8216656703010301, 93.05113791807858092 ) ) ;
#15560 = EDGE_CURVE ( 'NONE', #25621, #1492, #27828, .T. ) ;
#15561 = CARTESIAN_POINT ( 'NONE',  ( -64.50000000000000000, 155.0000000000000000, 6.938893903907228378E-15 ) ) ;
#15562 = VERTEX_POINT ( 'NONE', #22383 ) ;
#15563 = CARTESIAN_POINT ( 'NONE',  ( 8.062137200540822946, 212.9164362838583315, 90.69886208192143329 ) ) ;
#15564 = CARTESIAN_POINT ( 'NONE',  ( -7.456977232089471386, 217.1783343296987709, 20.94886208192143684 ) ) ;
#15565 = CARTESIAN_POINT ( 'NONE',  ( -64.96121601855533356, -1.809269760319447418, 19.53878398144468775 ) ) ;
#15566 = CARTESIAN_POINT ( 'NONE',  ( -10.00000000000000711, 207.0476921513413515, 39.50113791807856956 ) ) ;
#15567 = EDGE_LOOP ( 'NONE', ( #30562, #10849, #28280, #22698 ) ) ;
#15568 = CARTESIAN_POINT ( 'NONE',  ( 2.517493886309087436, 199.4062855549015865, 1.598862081921434974 ) ) ;
#15569 = EDGE_CURVE ( 'NONE', #21649, #16763, #2340, .T. ) ;
#15570 = CARTESIAN_POINT ( 'NONE',  ( -6.500000000000000000, -3.752776749732572803, -8.000000000000000000 ) ) ;
#15571 = ORIENTED_EDGE ( 'NONE', *, *, #17705, .F. ) ;
#15572 = CARTESIAN_POINT ( 'NONE',  ( -8.000000000000008882, 206.9523078486584780, 89.49886208192144466 ) ) ;
#15573 = ORIENTED_EDGE ( 'NONE', *, *, #6230, .F. ) ;
#15574 = CARTESIAN_POINT ( 'NONE',  ( -4.903702542908602524, 213.8346818373418898, 30.95113791807857595 ) ) ;
#15575 = EDGE_LOOP ( 'NONE', ( #7551, #27971, #7078, #27178, #32119 ) ) ;
#15576 = DIRECTION ( 'NONE',  ( 1.000000000000000000, 0.000000000000000000, 0.000000000000000000 ) ) ;
#15577 = EDGE_CURVE ( 'NONE', #31166, #27139, #33343, .T. ) ;
#15578 = CARTESIAN_POINT ( 'NONE',  ( 83.02499999726879309, 149.9369285172503510, -15.58253175000000823 ) ) ;
#15579 = DIRECTION ( 'NONE',  ( 0.000000000000000000, 0.000000000000000000, -1.000000000000000000 ) ) ;
#15580 = CARTESIAN_POINT ( 'NONE',  ( -6.444103211791042618, 211.7408657792732356, 90.80113791807858092 ) ) ;
#15581 = CARTESIAN_POINT ( 'NONE',  ( 89.50000000000001421, 155.0000000000000000, -6.938893903907228378E-15 ) ) ;
#15582 = DIRECTION ( 'NONE',  ( 0.000000000000000000, 0.000000000000000000, -1.000000000000000000 ) ) ;
#15583 = CARTESIAN_POINT ( 'NONE',  ( 51.29999999999999716, 163.5228861582408797, 11.73074641843673049 ) ) ;
#15584 = CARTESIAN_POINT ( 'NONE',  ( 6.500168698208244500, 202.3363017425938324, 64.29886208192144181 ) ) ;
#15585 = CARTESIAN_POINT ( 'NONE',  ( 27.49999999999999645, -10.64700562007353923, -1.134120025693882594 ) ) ;
#15586 = EDGE_CURVE ( 'NONE', #28270, #16107, #4254, .T. ) ;
#15587 = VECTOR ( 'NONE', #5303, 1000.000000000000114 ) ;
#15588 = CARTESIAN_POINT ( 'NONE',  ( 50.52499999726880731, 140.1801316387863778, 4.815267126137185549 ) ) ;
#15589 = CLOSED_SHELL ( 'NONE', ( #6204, #7808, #14109, #19890, #3933, #12092, #15815, #16207, #8045, #13762, #6229, #28944, #5756, #2842, #9998, #20566, #14099, #3098, #4931, #24596, #16976, #31395, #30929, #6197, #10390, #6482, #22700 ) ) ;
#15590 = CARTESIAN_POINT ( 'NONE',  ( -6.220909254589537696, 198.5229672870051445, 0.05113791807856578331 ) ) ;
#15591 = DIRECTION ( 'NONE',  ( -0.3500148194780949296, -0.04467534437043436946, 0.9356782244720136532 ) ) ;
#15592 = CARTESIAN_POINT ( 'NONE',  ( 58.42499999726880588, 141.7447067706911810, 9.630534252274376428 ) ) ;
#15593 = CARTESIAN_POINT ( 'NONE',  ( 70.57499999726881867, 145.8408176439707802, 12.60653300113718345 ) ) ;
#15594 = CARTESIAN_POINT ( 'NONE',  ( 7.375838497908181246, 196.7627149292499666, 68.45113791807857240 ) ) ;
#15595 = CARTESIAN_POINT ( 'NONE',  ( 41.61132485994280472, 150.1262045565064227, -15.00000000000002665 ) ) ;
#15596 = CARTESIAN_POINT ( 'NONE',  ( 0.05014649552807549926, 219.6175466908591716, 10.25113791807856600 ) ) ;
#15597 = CARTESIAN_POINT ( 'NONE',  ( -6.220909254589537696, 198.5229672870051445, 84.05113791807856671 ) ) ;
#15598 = AXIS2_PLACEMENT_3D ( 'NONE', #2446, #15213, #9940 ) ;
#15599 = CARTESIAN_POINT ( 'NONE',  ( 7.375838497908012492, 217.2372850707501186, 54.54886208192142760 ) ) ;
#15600 = CARTESIAN_POINT ( 'NONE',  ( -6.220909254589682469, 215.4770327129947134, 59.94886208192142618 ) ) ;
#15601 = CARTESIAN_POINT ( 'NONE',  ( -7.456977232089304408, 196.8216656703010301, 93.05113791807858092 ) ) ;
#15602 = CARTESIAN_POINT ( 'NONE',  ( 34.58867513459482268, 146.1832212156128890, -12.13525491562423042 ) ) ;
#15603 = CARTESIAN_POINT ( 'NONE',  ( 8.062137200540920645, 201.0835637161417822, 11.30113791807856671 ) ) ;
#15604 = CARTESIAN_POINT ( 'NONE',  ( -10.01549611932659722, 210.2015048109875011, 74.64886208192142192 ) ) ;
#15605 = ORIENTED_EDGE ( 'NONE', *, *, #21659, .T. ) ;
#15606 = CARTESIAN_POINT ( 'NONE',  ( -7.456977232089471386, 217.1783343296987709, 77.94886208192143329 ) ) ;
#15607 = CARTESIAN_POINT ( 'NONE',  ( 3.044812012440130555, 197.4746971517856764, 98.60113791807857808 ) ) ;
#15608 = ORIENTED_EDGE ( 'NONE', *, *, #2109, .F. ) ;
#15609 = FACE_OUTER_BOUND ( 'NONE', #31384, .T. ) ;
#15610 = CARTESIAN_POINT ( 'NONE',  ( 2.517493886309087436, 199.4062855549015865, 55.59886208192143897 ) ) ;
#15611 = CIRCLE ( 'NONE', #32478, 18.00000000000000711 ) ;
#15612 = ORIENTED_EDGE ( 'NONE', *, *, #31990, .F. ) ;
#15613 = PRESENTATION_LAYER_ASSIGNMENT (  '', '', ( #11264 ) ) ;
#15614 = CARTESIAN_POINT ( 'NONE',  ( 72.32499999726880446, 145.8408176439707802, 12.60653300113718345 ) ) ;
#15615 = CARTESIAN_POINT ( 'NONE',  ( 6.500000000000000888, -4.076778466486154606, -6.121917890101376436 ) ) ;
#15616 = AXIS2_PLACEMENT_3D ( 'NONE', #9371, #14816, #14991 ) ;
#15617 = FACE_OUTER_BOUND ( 'NONE', #12423, .T. ) ;
#15618 = CARTESIAN_POINT ( 'NONE',  ( 60.82499999726881867, 141.7447067706911810, -9.630534252274385310 ) ) ;
#15619 = EDGE_CURVE ( 'NONE', #10922, #13276, #13178, .T. ) ;
#15620 = CARTESIAN_POINT ( 'NONE',  ( -7.908219015560238319, -3.084967917785936820, -7.795665562178438535 ) ) ;
#15621 = EDGE_CURVE ( 'NONE', #4805, #23382, #2288, .T. ) ;
#15622 = CARTESIAN_POINT ( 'NONE',  ( 3.044812012439969795, 216.5253028482143520, 48.39886208192143613 ) ) ;
#15623 = EDGE_LOOP ( 'NONE', ( #371, #17779, #9282, #11340, #11395, #33214 ) ) ;
#15624 = CIRCLE ( 'NONE', #31930, 15.50000000000001066 ) ;
#15625 = CARTESIAN_POINT ( 'NONE',  ( 4.000000000000000000, 1.759474945355380404, -3.047500000000001652 ) ) ;
#15626 = CARTESIAN_POINT ( 'NONE',  ( 4.000000000000000000, 0.000000000000000000, 3.047499999999999876 ) ) ;
#15627 = CARTESIAN_POINT ( 'NONE',  ( -8.000000000000008882, 206.9523078486584780, 35.49886208192143044 ) ) ;
#15628 = CARTESIAN_POINT ( 'NONE',  ( -3.135527875058821579, 197.5041725223112223, 74.90113791807857524 ) ) ;
#15629 = CARTESIAN_POINT ( 'NONE',  ( -3.376928366568182163E-14, -72.99999999999997158, 30.00000000000000000 ) ) ;
#15630 = ADVANCED_FACE ( 'NONE', ( #31248 ), #4517, .T. ) ;
#15631 = CARTESIAN_POINT ( 'NONE',  ( 3.044812012440130555, 197.4746971517856764, 59.60113791807857808 ) ) ;
#15632 = CARTESIAN_POINT ( 'NONE',  ( 3.044812012440130555, 197.4746971517856764, 26.60113791807856742 ) ) ;
#15633 = CARTESIAN_POINT ( 'NONE',  ( -4.903702542908602524, 213.8346818373418898, 12.95113791807856707 ) ) ;
#15634 = DIRECTION ( 'NONE',  ( 0.000000000000000000, 0.000000000000000000, -1.000000000000000000 ) ) ;
#15635 = CARTESIAN_POINT ( 'NONE',  ( -64.50000000000000000, 155.0000000000000000, 6.938893903907228378E-15 ) ) ;
#15636 = CARTESIAN_POINT ( 'NONE',  ( 36.12499999726881583, 155.0000000000000000, 15.58253174999999402 ) ) ;
#15637 = CARTESIAN_POINT ( 'NONE',  ( -0.05014649552807705357, 194.3824533091408000, 38.75113791807856245 ) ) ;
#15638 = FACE_OUTER_BOUND ( 'NONE', #10802, .T. ) ;
#15639 = AXIS2_PLACEMENT_3D ( 'NONE', #15505, #26071, #10406 ) ;
#15640 = EDGE_CURVE ( 'NONE', #2728, #5762, #18292, .T. ) ;
#15641 = CARTESIAN_POINT ( 'NONE',  ( -0.05014649552810635652, 196.4853777576173002, 89.75113791807854113 ) ) ;
#15642 = CARTESIAN_POINT ( 'NONE',  ( 3.135527875058820690, 216.4958274776887492, 58.40113791807857524 ) ) ;
#15643 = PRESENTATION_LAYER_ASSIGNMENT (  '', '', ( #9655 ) ) ;
#15644 = FACE_OUTER_BOUND ( 'NONE', #20476, .T. ) ;
#15645 = VECTOR ( 'NONE', #1662, 1000.000000000000000 ) ;
#15646 = CARTESIAN_POINT ( 'NONE',  ( 9.680171189290716072, 214.0920067884432854, 27.69886208192143684 ) ) ;
#15647 = CIRCLE ( 'NONE', #6939, 8.331345277524542681 ) ;
#15648 = CARTESIAN_POINT ( 'NONE',  ( -0.05014649552828402690, 217.5146222423826714, 27.24886208192143400 ) ) ;
#15649 = CARTESIAN_POINT ( 'NONE',  ( 79.39999999453763735, 141.2096805137202580, 4.480746418436733158 ) ) ;
#15650 = CARTESIAN_POINT ( 'NONE',  ( -0.05014649552807705357, 194.3824533091408000, 68.75113791807856956 ) ) ;
#15651 = CARTESIAN_POINT ( 'NONE',  ( -2.517493886308901807, 199.4062855549015012, 89.90113791807857524 ) ) ;
#15652 = CARTESIAN_POINT ( 'NONE',  ( -3.044812012439970683, 197.4746971517856196, 46.89886208192143613 ) ) ;
#15653 = DIRECTION ( 'NONE',  ( 1.000000000000000000, 0.000000000000000000, 0.000000000000000000 ) ) ;
#15654 = VECTOR ( 'NONE', #5665, 1000.000000000000000 ) ;
#15655 = ORIENTED_EDGE ( 'NONE', *, *, #33042, .F. ) ;
#15656 = CARTESIAN_POINT ( 'NONE',  ( 7.375838497908012492, 217.2372850707501186, 54.54886208192142760 ) ) ;
#15657 = VERTEX_POINT ( 'NONE', #26130 ) ;
#15658 = VERTEX_POINT ( 'NONE', #30915 ) ;
#15659 = DIRECTION ( 'NONE',  ( -0.000000000000000000, -0.000000000000000000, -1.000000000000000000 ) ) ;
#15660 = LINE ( 'NONE', #31015, #14904 ) ;
#15661 = EDGE_LOOP ( 'NONE', ( #24116, #1242 ) ) ;
#15662 = CARTESIAN_POINT ( 'NONE',  ( -4.903702542908602524, 213.8346818373418898, 45.95113791807857950 ) ) ;
#15663 = CIRCLE ( 'NONE', #8068, 5.250000000000004441 ) ;
#15664 = CIRCLE ( 'NONE', #30908, 3.999999999999999112 ) ;
#15665 = CARTESIAN_POINT ( 'NONE',  ( 0.05014649552828275708, 196.4853777576173002, 22.74886208192142689 ) ) ;
#15666 = CARTESIAN_POINT ( 'NONE',  ( 63.07499999726881867, 141.7447067706911810, -9.630534252274387086 ) ) ;
#15667 = ORIENTED_EDGE ( 'NONE', *, *, #17414, .F. ) ;
#15668 = PLANE ( 'NONE',  #15639 ) ;
#15669 = VECTOR ( 'NONE', #32631, 1000.000000000000000 ) ;
#15670 = DIRECTION ( 'NONE',  ( 1.000000000000000000, 0.000000000000000000, 0.000000000000000000 ) ) ;
#15671 = CARTESIAN_POINT ( 'NONE',  ( -8.015496119326597224, 209.5516654185217362, 2.648862081921435241 ) ) ;
#15672 = CARTESIAN_POINT ( 'NONE',  ( -3.044812012440131443, 216.5253028482142952, 40.10113791807857098 ) ) ;
#15673 =( BOUNDED_CURVE ( )  B_SPLINE_CURVE ( 2, ( #8851, #27871, #4546, #12378, #33168, #25840, #7620, #31613, #31454, #26165, #18004 ),
 .UNSPECIFIED., .F., .T. ) 
 B_SPLINE_CURVE_WITH_KNOTS ( ( 3, 2, 2, 2, 2, 3 ),
 ( 0.6071428571428569843, 0.6107142857142856540, 0.6142857142857142128, 0.6178571428571427715, 0.6214285714285713302, 0.6249999999999998890 ),
 .UNSPECIFIED. ) 
 CURVE ( )  GEOMETRIC_REPRESENTATION_ITEM ( )  RATIONAL_B_SPLINE_CURVE ( ( 1.000000000000001554, 0.9510565162951518658, 1.000000000000000000, 0.9510565162951534202, 1.000000000000000000, 0.9510565162951534202, 1.000000000000000000, 0.9510565162951534202, 1.000000000000000000, 0.9510565162951549745, 0.9999999999999984457 ) ) 
 REPRESENTATION_ITEM ( '' )  );
#15674 = CARTESIAN_POINT ( 'NONE',  ( -8.062137200540920645, 212.9164362838581894, 30.80113791807856671 ) ) ;
#15675 = CARTESIAN_POINT ( 'NONE',  ( 10.00000000000000178, 0.000000000000000000, 0.000000000000000000 ) ) ;
#15676 = AXIS2_PLACEMENT_3D ( 'NONE', #14497, #22849, #1897 ) ;
#15677 = PRODUCT_CONTEXT ( 'NONE', #20073, 'mechanical' ) ;
#15678 = CARTESIAN_POINT ( 'NONE',  ( 0.05014649552828262524, 198.5883022060938572, 91.74886208192144466 ) ) ;
#15679 = CARTESIAN_POINT ( 'NONE',  ( 86.60000000000000853, 159.7113355953771077, -14.50000000000000888 ) ) ;
#15680 = CYLINDRICAL_SURFACE ( 'NONE', #29056, 18.00000000000000355 ) ;
#15681 = DIRECTION ( 'NONE',  ( -1.000000000000000000, 0.000000000000000000, 0.000000000000000000 ) ) ;
#15682 = CARTESIAN_POINT ( 'NONE',  ( 3.662846001190051659, 195.5725841191953691, 14.60113791807856742 ) ) ;
#15683 = DIRECTION ( 'NONE',  ( 0.000000000000000000, 0.000000000000000000, 1.000000000000000000 ) ) ;
#15684 = CARTESIAN_POINT ( 'NONE',  ( 57.17499999726881299, 145.8408176439707802, -12.60653300113719588 ) ) ;
#15685 = CARTESIAN_POINT ( 'NONE',  ( 0.05014649552810505201, 217.5146222423826714, 55.25113791807858377 ) ) ;
#15686 = DIRECTION ( 'NONE',  ( -1.000000000000000000, 0.000000000000000000, 0.000000000000000000 ) ) ;
#15687 = CARTESIAN_POINT ( 'NONE',  ( 65.01132485994280330, 142.2402378747194405, 9.270509831248432420 ) ) ;
#15688 = CARTESIAN_POINT ( 'NONE',  ( 59.29999999453762882, 142.6655632788954620, 8.961492836873471646 ) ) ;
#15689 = ORIENTED_EDGE ( 'NONE', *, *, #27696, .T. ) ;
#15690 = CARTESIAN_POINT ( 'NONE',  ( 12.00000000000000711, 206.9523078486586485, 35.00113791807857666 ) ) ;
#15691 = CARTESIAN_POINT ( 'NONE',  ( 47.21132485994281325, 139.2280666364260071, -4.041636747397287284E-15 ) ) ;
#15692 = CARTESIAN_POINT ( 'NONE',  ( -10.01549611932659722, 210.2015048109875011, 11.64886208192143258 ) ) ;
#15693 = VECTOR ( 'NONE', #6442, 1000.000000000000000 ) ;
#15694 = CARTESIAN_POINT ( 'NONE',  ( -125.0000000000000000, 0.000000000000000000, -20.00000000000000000 ) ) ;
#15695 = ORIENTED_EDGE ( 'NONE', *, *, #12672, .T. ) ;
#15696 = ADVANCED_BREP_SHAPE_REPRESENTATION ( '', ( #951, #2404 ), #27385 ) ;
#15697 = CARTESIAN_POINT ( 'NONE',  ( 8.062137200540920645, 201.0835637161417822, 74.30113791807858092 ) ) ;
#15698 = VERTEX_POINT ( 'NONE', #7742 ) ;
#15699 = CARTESIAN_POINT ( 'NONE',  ( 8.000000000000008882, 207.0476921513415220, 36.99886208192143044 ) ) ;
#15700 = TOROIDAL_SURFACE ( 'NONE', #1541, 70.00000000000001421, 27.99999999999999645 ) ;
#15701 = CARTESIAN_POINT ( 'NONE',  ( 44.41132485994282320, 167.7597621252805880, 9.270509831248428867 ) ) ;
#15702 = VERTEX_POINT ( 'NONE', #12673 ) ;
#15703 = CARTESIAN_POINT ( 'NONE',  ( 6.444103211791042618, 202.2591342207267644, 14.30113791807856849 ) ) ;
#15704 = CARTESIAN_POINT ( 'NONE',  ( -7.456977232089471386, 217.1783343296987709, 101.9488620819214475 ) ) ;
#15705 = CARTESIAN_POINT ( 'NONE',  ( 43.37499999726881583, 155.0000000000000000, -15.58253175000000823 ) ) ;
#15706 = ORIENTED_EDGE ( 'NONE', *, *, #20345, .F. ) ;
#15707 = CARTESIAN_POINT ( 'NONE',  ( 52.52499999726881441, 140.1801316387863778, 4.815267126137185549 ) ) ;
#15708 = DIRECTION ( 'NONE',  ( 1.000000000000000000, 0.000000000000000000, 0.000000000000000000 ) ) ;
#15709 = CARTESIAN_POINT ( 'NONE',  ( -6.220909254589537696, 198.5229672870051161, 12.05113791807856671 ) ) ;
#15710 = CIRCLE ( 'NONE', #13022, 30.00000000000000000 ) ;
#15711 = CARTESIAN_POINT ( 'NONE',  ( -3.135527875058982783, 216.4958274776886924, 81.09886208192143897 ) ) ;
#15712 = CARTESIAN_POINT ( 'NONE',  ( 51.07499999726879736, 141.7447067706911810, -9.630534252274385310 ) ) ;
#15713 = CARTESIAN_POINT ( 'NONE',  ( 78.91132485994282320, 146.1832212156128890, 12.13525491562421976 ) ) ;
#15714 = CARTESIAN_POINT ( 'NONE',  ( 6.139770520408368348, 198.4640165459539674, 14.45113791807856352 ) ) ;
#15715 = DIRECTION ( 'NONE',  ( 0.000000000000000000, -1.000000000000000000, 0.000000000000000000 ) ) ;
#15716 = CIRCLE ( 'NONE', #8119, 8.000000000000000000 ) ;
#15717 = CARTESIAN_POINT ( 'NONE',  ( 9.680171189290831535, 199.9079932115568852, 38.30113791807856671 ) ) ;
#15718 = CARTESIAN_POINT ( 'NONE',  ( 64.29999999999999716, 146.4771138417591203, -11.73074641843674470 ) ) ;
#15719 = CARTESIAN_POINT ( 'NONE',  ( -6.139770520408369237, 215.5359834540460042, 99.95113791807855819 ) ) ;
#15720 = FACE_BOUND ( 'NONE', #17974, .T. ) ;
#15721 = CARTESIAN_POINT ( 'NONE',  ( 0.05014649552810505201, 217.5146222423826714, 88.25113791807858377 ) ) ;
#15722 = CARTESIAN_POINT ( 'NONE',  ( 32.50000000000000000, 155.0000000000000000, 15.00000000000001243 ) ) ;
#15723 = CARTESIAN_POINT ( 'NONE',  ( 38.47499999726881015, 149.9369285172503510, 15.58253174999999580 ) ) ;
#15724 = CARTESIAN_POINT ( 'NONE',  ( -11.98450388067341876, 203.0532714938636047, 101.3488620819214390 ) ) ;
#15725 = EDGE_CURVE ( 'NONE', #16822, #6483, #6686, .T. ) ;
#15726 = VECTOR ( 'NONE', #18068, 1000.000000000000227 ) ;
#15727 = CARTESIAN_POINT ( 'NONE',  ( 69.22499999726881015, 160.0630714827496206, -15.58253175000000823 ) ) ;
#15728 = ORIENTED_EDGE ( 'NONE', *, *, #23368, .F. ) ;
#15729 = FACE_OUTER_BOUND ( 'NONE', #28895, .T. ) ;
#15730 = CARTESIAN_POINT ( 'NONE',  ( 33.99999999453763166, 155.0000000000000000, -14.50000000000000711 ) ) ;
#15731 = CARTESIAN_POINT ( 'NONE',  ( -9.736236675707914401, 199.9851607334237542, 96.20113791807858661 ) ) ;
#15732 = DIRECTION ( 'NONE',  ( -1.000000000000000000, -4.625929269271485914E-16, 0.000000000000000000 ) ) ;
#15733 = EDGE_LOOP ( 'NONE', ( #15227, #22706, #572 ) ) ;
#15734 = CARTESIAN_POINT ( 'NONE',  ( -9.984503880673420539, 203.7031108863293980, 89.34886208192143897 ) ) ;
#15735 = CARTESIAN_POINT ( 'NONE',  ( 3.662846001189864698, 218.4274158808046593, 21.39886208192143613 ) ) ;
#15736 = DIRECTION ( 'NONE',  ( 0.000000000000000000, 0.000000000000000000, -1.000000000000000000 ) ) ;
#15737 = AXIS2_PLACEMENT_3D ( 'NONE', #1432, #11662, #19492 ) ;
#15738 = CARTESIAN_POINT ( 'NONE',  ( -3.135527875058821579, 197.5041725223112223, 38.90113791807857524 ) ) ;
#15739 = AXIS2_PLACEMENT_3D ( 'NONE', #24181, #8836, #21618 ) ;
#15740 = ORIENTED_EDGE ( 'NONE', *, *, #29322, .F. ) ;
#15741 = CARTESIAN_POINT ( 'NONE',  ( 8.000000000000008882, 207.0476921513415220, 6.998862081921435774 ) ) ;
#15742 = CARTESIAN_POINT ( 'NONE',  ( 74.21132485994283456, 170.7719333635740497, -7.904646289410545231E-15 ) ) ;
#15743 = ORIENTED_EDGE ( 'NONE', *, *, #13073, .T. ) ;
#15744 = CARTESIAN_POINT ( 'NONE',  ( -8.015496119326597224, 209.5516654185217362, 92.64886208192143613 ) ) ;
#15745 =( REPRESENTATION_RELATIONSHIP ('NONE','NONE', #25663, #22175 ) REPRESENTATION_RELATIONSHIP_WITH_TRANSFORMATION ( #1509 )SHAPE_REPRESENTATION_RELATIONSHIP( ) );
#15746 = CARTESIAN_POINT ( 'NONE',  ( 8.000000000000008882, 206.9523078486586485, 26.00113791807856600 ) ) ;
#15747 = CARTESIAN_POINT ( 'NONE',  ( 80.78867513459482552, 155.0000000000000000, -15.00000000000002487 ) ) ;
#15748 = ORIENTED_EDGE ( 'NONE', *, *, #3082, .T. ) ;
#15749 = CARTESIAN_POINT ( 'NONE',  ( 2.387978478801324300, 7.281554020289410012, -7.069802615102035226 ) ) ;
#15750 = CARTESIAN_POINT ( 'NONE',  ( 37.37499999726881583, 155.0000000000000000, -15.58253175000000823 ) ) ;
#15751 = DIRECTION ( 'NONE',  ( 0.000000000000000000, 0.000000000000000000, -1.000000000000000000 ) ) ;
#15752 = CARTESIAN_POINT ( 'NONE',  ( 0.05014649552807626948, 215.4116977939061144, 91.25113791807856956 ) ) ;
#15753 = DIRECTION ( 'NONE',  ( 1.000000000000000000, 0.000000000000000000, 0.000000000000000000 ) ) ;
#15754 = CARTESIAN_POINT ( 'NONE',  ( 47.10000000000000142, 168.7903194862797420, 4.480746418436729606 ) ) ;
#15755 = CARTESIAN_POINT ( 'NONE',  ( -4.903702542908436435, 200.1653181626580249, 65.04886208192144181 ) ) ;
#15756 = AXIS2_PLACEMENT_3D ( 'NONE', #5629, #3236, #18908 ) ;
#15757 = DIRECTION ( 'NONE',  ( 1.000000000000000000, 0.000000000000000000, 0.000000000000000000 ) ) ;
#15758 = EDGE_CURVE ( 'NONE', #16822, #11640, #4495, .T. ) ;
#15759 = CARTESIAN_POINT ( 'NONE',  ( 49.32499999726881157, 164.1591823560292198, -12.60653300113719766 ) ) ;
#15760 = CARTESIAN_POINT ( 'NONE',  ( 9.984503880673473830, 203.7031108863295401, -0.8488620819214343083 ) ) ;
#15761 = FACE_OUTER_BOUND ( 'NONE', #21844, .T. ) ;
#15762 = CARTESIAN_POINT ( 'NONE',  ( 61.22499999726880304, 160.0630714827496206, -15.58253175000000823 ) ) ;
#15763 = CARTESIAN_POINT ( 'NONE',  ( 69.27499999726880731, 149.9369285172503510, -15.58253175000000823 ) ) ;
#15764 = CARTESIAN_POINT ( 'NONE',  ( 12.01549611932652972, 210.8513442034534933, 64.85113791807857808 ) ) ;
#15765 = DIRECTION ( 'NONE',  ( 0.7071067811865454633, -0.000000000000000000, 0.7071067811865495711 ) ) ;
#15766 = CARTESIAN_POINT ( 'NONE',  ( 3.135527875058820690, 216.4958274776887492, 91.40113791807857524 ) ) ;
#15767 = CARTESIAN_POINT ( 'NONE',  ( 62.70000000000001705, -88.00000000000000000, -20.00000000000000000 ) ) ;
#15768 = EDGE_CURVE ( 'NONE', #26664, #28067, #3952, .T. ) ;
#15769 = CARTESIAN_POINT ( 'NONE',  ( 9.680171189290716072, 214.0920067884432854, 54.69886208192144039 ) ) ;
#15770 = CARTESIAN_POINT ( 'NONE',  ( 10.00000000000000711, 207.0476921513415220, 54.99886208192143755 ) ) ;
#15771 = CARTESIAN_POINT ( 'NONE',  ( 0.05014649552807549926, 219.6175466908591716, 97.25113791807856956 ) ) ;
#15772 = CARTESIAN_POINT ( 'NONE',  ( -67.50001199999999812, 171.8904165060497178, 2.225267283893263226 ) ) ;
#15773 = CARTESIAN_POINT ( 'NONE',  ( 3.135527875058820690, 216.4958274776887492, 13.40113791807856636 ) ) ;
#15774 = CARTESIAN_POINT ( 'NONE',  ( 8.062137200540822946, 212.9164362838583315, 75.69886208192143329 ) ) ;
#15775 = ORIENTED_EDGE ( 'NONE', *, *, #13967, .T. ) ;
#15776 = CARTESIAN_POINT ( 'NONE',  ( -12.01549611932659722, 210.8513442034533227, 77.64886208192143613 ) ) ;
#15777 = CARTESIAN_POINT ( 'NONE',  ( -8.118202686958039038, 201.1607312380087080, 99.20113791807858661 ) ) ;
#15778 = EDGE_LOOP ( 'NONE', ( #5886, #15329, #8081 ) ) ;
#15779 = CARTESIAN_POINT ( 'NONE',  ( -4.984841277089891776, 213.7757310962905990, 65.94886208192144750 ) ) ;
#15780 = ORIENTED_EDGE ( 'NONE', *, *, #2735, .F. ) ;
#15781 = ADVANCED_FACE ( 'NONE', ( #10131 ), #5009, .T. ) ;
#15782 = CARTESIAN_POINT ( 'NONE',  ( 75.52499999726880731, 169.8198683612136222, -4.815267126137197984 ) ) ;
#15783 = CARTESIAN_POINT ( 'NONE',  ( 0.3999999999999975797, 0.000000000000000000, 0.000000000000000000 ) ) ;
#15784 = CARTESIAN_POINT ( 'NONE',  ( -56.33087447058203168, 194.9805812333615620, -1.253637678855320958 ) ) ;
#15785 = B_SPLINE_CURVE_WITH_KNOTS ( 'NONE', 3,
 ( #19949, #28126, #30348, #4787, #24735, #11777 ),
 .UNSPECIFIED., .F., .F.,
 ( 4, 2, 4 ),
 ( 2.380727408751203747E-07, 0.008032766472079738360, 0.01606529487141860127 ),
 .UNSPECIFIED. ) ;
#15786 = UNCERTAINTY_MEASURE_WITH_UNIT (LENGTH_MEASURE( 1.000000000000000082E-05 ), #15345, 'distance_accuracy_value', 'NONE');
#15787 = ADVANCED_FACE ( 'NONE', ( #20511, #28355 ), #18463, .F. ) ;
#15788 = CARTESIAN_POINT ( 'NONE',  ( 61.22499999726880304, 160.0630714827496206, -15.58253175000000823 ) ) ;
#15789 = CARTESIAN_POINT ( 'NONE',  ( -7.915341292092594294, -3.857523022641989652, -7.913710289178173873 ) ) ;
#15790 = CARTESIAN_POINT ( 'NONE',  ( 8.118202686958138514, 201.1607312380088501, 52.29886208192143471 ) ) ;
#15791 = ORIENTED_EDGE ( 'NONE', *, *, #17878, .T. ) ;
#15792 = CARTESIAN_POINT ( 'NONE',  ( 115.4999999999999858, 183.9550983604194698, 103.9084171661920095 ) ) ;
#15793 =( NAMED_UNIT ( * ) PLANE_ANGLE_UNIT ( ) SI_UNIT ( $, .RADIAN. ) );
#15794 = CARTESIAN_POINT ( 'NONE',  ( -125.0000000000000000, -25.00000000000000000, -35.00000000000000000 ) ) ;
#15795 = CARTESIAN_POINT ( 'NONE',  ( 0.05014649552828262524, 198.5883022060938572, 37.74886208192143755 ) ) ;
#15796 = CARTESIAN_POINT ( 'NONE',  ( -3.135527875058821579, 197.5041725223112223, 77.90113791807857524 ) ) ;
#15797 = DIRECTION ( 'NONE',  ( 0.000000000000000000, 0.000000000000000000, -1.000000000000000000 ) ) ;
#15798 = CARTESIAN_POINT ( 'NONE',  ( -3.135527875058821579, 197.5041725223112223, 53.90113791807857524 ) ) ;
#15799 = CARTESIAN_POINT ( 'NONE',  ( 10.00000000000000711, 206.9523078486586201, 23.00113791807856600 ) ) ;
#15800 = CARTESIAN_POINT ( 'NONE',  ( 2.426778023690261410, 199.3768101843759837, 14.60113791807856742 ) ) ;
#15801 = CARTESIAN_POINT ( 'NONE',  ( 119.7500000000000000, 3.125910954823619074E-14, 35.00000599999999906 ) ) ;
#15802 = DIRECTION ( 'NONE',  ( 0.000000000000000000, 0.000000000000000000, -1.000000000000000000 ) ) ;
#15803 = CARTESIAN_POINT ( 'NONE',  ( 37.32499999726881157, 164.1591823560292198, -12.60653300113719766 ) ) ;
#15804 = CARTESIAN_POINT ( 'NONE',  ( 9.736236675707914401, 214.0148392665762458, 40.70113791807857240 ) ) ;
#15805 = FACE_BOUND ( 'NONE', #1450, .T. ) ;
#15806 = CARTESIAN_POINT ( 'NONE',  ( -0.05014649552810635652, 196.4853777576173002, 86.75113791807858377 ) ) ;
#15807 = CARTESIAN_POINT ( 'NONE',  ( -9.984503880673475606, 210.2968891136704315, 57.65113791807857524 ) ) ;
#15808 = CARTESIAN_POINT ( 'NONE',  ( -3.662846001189865142, 195.5725841191952838, 22.89886208192143613 ) ) ;
#15809 = CARTESIAN_POINT ( 'NONE',  ( -3.135527875058982783, 216.4958274776886924, 27.09886208192143542 ) ) ;
#15810 = CARTESIAN_POINT ( 'NONE',  ( 80.09999999453761177, 159.7113355953771077, -14.50000000000000888 ) ) ;
#15811 = CARTESIAN_POINT ( 'NONE',  ( -9.680171189290831535, 214.0920067884431148, 66.80113791807858092 ) ) ;
#15812 = CARTESIAN_POINT ( 'NONE',  ( 8.015496119326531499, 209.5516654185219636, 88.85113791807857808 ) ) ;
#15813 = ADVANCED_FACE ( 'NONE', ( #25451 ), #1787, .T. ) ;
#15814 = CARTESIAN_POINT ( 'NONE',  ( 10.01549611932659545, 203.7984951890123853, 46.14886208192143613 ) ) ;
#15815 = ADVANCED_FACE ( 'NONE', ( #12510, #20344 ), #30743, .T. ) ;
#15816 = PLANE ( 'NONE',  #2572 ) ;
#15817 = AXIS2_PLACEMENT_3D ( 'NONE', #21124, #23014, #15681 ) ;
#15818 = ORIENTED_EDGE ( 'NONE', *, *, #10995, .F. ) ;
#15819 = CARTESIAN_POINT ( 'NONE',  ( -12.01549611932659722, 210.8513442034533227, 56.64886208192142902 ) ) ;
#15820 = AXIS2_PLACEMENT_3D ( 'NONE', #32001, #26893, #8826 ) ;
#15821 = ORIENTED_EDGE ( 'NONE', *, *, #8901, .T. ) ;
#15822 = EDGE_LOOP ( 'NONE', ( #6595, #25072, #24540, #2806, #28876 ) ) ;
#15823 = EDGE_CURVE ( 'NONE', #31739, #16522, #27877, .T. ) ;
#15824 = CARTESIAN_POINT ( 'NONE',  ( 87.50000000000001421, 166.8192717339189812, 9.236060614774261879 ) ) ;
#15825 = CARTESIAN_POINT ( 'NONE',  ( 56.18867513459483121, 140.7341522555726669, 4.635254915624211769 ) ) ;
#15826 = CARTESIAN_POINT ( 'NONE',  ( -6.500168698208129925, 202.3363017425936050, 39.20113791807857240 ) ) ;
#15827 = EDGE_CURVE ( 'NONE', #2182, #6483, #31083, .T. ) ;
#15828 = CARTESIAN_POINT ( 'NONE',  ( 82.21132485994283456, 170.7719333635740497, -7.904646289410545231E-15 ) ) ;
#15829 = CARTESIAN_POINT ( 'NONE',  ( -6.220909254589682469, 215.4770327129946850, 23.94886208192142618 ) ) ;
#15830 = CARTESIAN_POINT ( 'NONE',  ( 64.77499999726882152, 140.1801316387863778, 4.815267126137185549 ) ) ;
#15831 = ORIENTED_EDGE ( 'NONE', *, *, #31256, .F. ) ;
#15832 = DIRECTION ( 'NONE',  ( -0.9998603841633338929, 0.01669062914075312987, 0.0007969188393214247284 ) ) ;
#15833 =( NAMED_UNIT ( * ) SI_UNIT ( $, .STERADIAN. ) SOLID_ANGLE_UNIT ( ) );
#15834 = CARTESIAN_POINT ( 'NONE',  ( 43.78867513459481842, 155.0000000000000000, 15.00000000000001243 ) ) ;
#15835 = CARTESIAN_POINT ( 'NONE',  ( 7.984503880673422316, 209.6470497212048372, 9.848862081921433642 ) ) ;
#15836 = CARTESIAN_POINT ( 'NONE',  ( 8.062137200540920645, 201.0835637161417822, 44.30113791807857382 ) ) ;
#15837 = CARTESIAN_POINT ( 'NONE',  ( 125.5000000000000000, 81.56696077377658582, -76.47359838532473475 ) ) ;
#15838 = CARTESIAN_POINT ( 'NONE',  ( 8.118202686958039038, 212.8392687619912635, 28.70113791807856884 ) ) ;
#15839 = CARTESIAN_POINT ( 'NONE',  ( -0.05014649552828402690, 217.5146222423826714, 102.2488620819214304 ) ) ;
#15840 = APPLICATION_PROTOCOL_DEFINITION ( 'draft international standard', 'automotive_design', 1998, #15940 ) ;
#15841 = AXIS2_PLACEMENT_3D ( 'NONE', #7310, #10539, #26033 ) ;
#15842 = CARTESIAN_POINT ( 'NONE',  ( -4.984841277089891776, 213.7757310962905990, 89.94886208192144750 ) ) ;
#15843 = CARTESIAN_POINT ( 'NONE',  ( 37.22499999726881015, 160.0630714827496206, -15.58253175000000823 ) ) ;
#15844 = CARTESIAN_POINT ( 'NONE',  ( -57.24471460971760450, 194.9412964752286825, 2.168227419017068502 ) ) ;
#15845 = CARTESIAN_POINT ( 'NONE',  ( -22.98492866215537589, 18.48391005502966777, -16.91127448208919759 ) ) ;
#15846 = CARTESIAN_POINT ( 'NONE',  ( -7.456977232089304408, 196.8216656703010301, 6.051137918078566713 ) ) ;
#15847 = FACE_OUTER_BOUND ( 'NONE', #6175, .T. ) ;
#15848 = CARTESIAN_POINT ( 'NONE',  ( 60.47499999726881725, 149.9369285172503510, 15.58253174999999580 ) ) ;
#15849 = CARTESIAN_POINT ( 'NONE',  ( 9.984503880673470277, 203.7031108863295401, 56.15113791807856103 ) ) ;
#15850 = CARTESIAN_POINT ( 'NONE',  ( 8.118202686958039038, 212.8392687619912635, 31.70113791807856884 ) ) ;
#15851 = CARTESIAN_POINT ( 'NONE',  ( 35.11132485994280472, 140.7341522555726669, 4.635254915624211769 ) ) ;
#15852 = LINE ( 'NONE', #196, #26622 ) ;
#15853 = CARTESIAN_POINT ( 'NONE',  ( 50.78867513459482552, 155.0000000000000000, -15.00000000000002487 ) ) ;
#15854 = CARTESIAN_POINT ( 'NONE',  ( 61.99999999453763166, 155.0000000000000000, -14.50000000000000711 ) ) ;
#15855 = ORIENTED_EDGE ( 'NONE', *, *, #7429, .T. ) ;
#15856 = CARTESIAN_POINT ( 'NONE',  ( -9.736236675707914401, 199.9851607334237542, 36.20113791807856529 ) ) ;
#15857 = CARTESIAN_POINT ( 'NONE',  ( 77.11132485994281183, 140.7341522555726669, 4.635254915624211769 ) ) ;
#15858 = UNCERTAINTY_MEASURE_WITH_UNIT (LENGTH_MEASURE( 1.000000000000000082E-05 ), #32334, 'distance_accuracy_value', 'NONE');
#15859 = CARTESIAN_POINT ( 'NONE',  ( -3.044812012439970683, 197.4746971517856196, 16.89886208192143613 ) ) ;
#15860 = ADVANCED_FACE ( 'NONE', ( #20848 ), #18957, .T. ) ;
#15861 = CARTESIAN_POINT ( 'NONE',  ( 71.08867513459483689, 167.7597621252805880, -9.270509831248443078 ) ) ;
#15862 = EDGE_LOOP ( 'NONE', ( #25499, #30679, #5056, #27093 ) ) ;
#15863 = CARTESIAN_POINT ( 'NONE',  ( -10.01549611932653860, 203.7984951890123284, 66.35113791807853545 ) ) ;
#15864 = EDGE_LOOP ( 'NONE', ( #26960, #18465, #24924 ) ) ;
#15865 = DIRECTION ( 'NONE',  ( -0.1461455375466716444, 0.9854922318508084755, -0.08629335326029916042 ) ) ;
#15866 = PLANE ( 'NONE',  #731 ) ;
#15867 = ORIENTED_EDGE ( 'NONE', *, *, #26819, .F. ) ;
#15868 = CARTESIAN_POINT ( 'NONE',  ( -4.903702542908602524, 213.8346818373418898, 9.951137918078567068 ) ) ;
#15869 =( BOUNDED_CURVE ( )  B_SPLINE_CURVE ( 2, ( #29142, #3079, #26576, #859, #3406, #13467, #5961, #26744, #23860, #18427, #28977 ),
 .UNSPECIFIED., .F., .T. ) 
 B_SPLINE_CURVE_WITH_KNOTS ( ( 3, 2, 2, 2, 2, 3 ),
 ( 0.6785714285714284921, 0.6821428571428570509, 0.6857142857142856096, 0.6892857142857142794, 0.6928571428571428381, 0.6964285714285713969 ),
 .UNSPECIFIED. ) 
 CURVE ( )  GEOMETRIC_REPRESENTATION_ITEM ( )  RATIONAL_B_SPLINE_CURVE ( ( 1.000000000000001554, 0.9510565162951518658, 1.000000000000000000, 0.9510565162951534202, 1.000000000000000000, 0.9510565162951534202, 1.000000000000000000, 0.9510565162951534202, 1.000000000000000000, 0.9510565162951534202, 1.000000000000000000 ) ) 
 REPRESENTATION_ITEM ( '' )  );
#15870 = CARTESIAN_POINT ( 'NONE',  ( -11.98450388067341876, 203.0532714938636047, 98.34886208192145318 ) ) ;
#15871 = CARTESIAN_POINT ( 'NONE',  ( 41.27499999726880731, 149.9369285172503510, -15.58253175000000823 ) ) ;
#15872 = ORIENTED_EDGE ( 'NONE', *, *, #11608, .F. ) ;
#15873 = CARTESIAN_POINT ( 'NONE',  ( 53.82499999726881157, 168.2552932293087906, 9.630534252274372875 ) ) ;
#15874 = FACE_OUTER_BOUND ( 'NONE', #11887, .T. ) ;
#15875 = CARTESIAN_POINT ( 'NONE',  ( 3.135527875058820690, 216.4958274776887492, 4.401137918078565470 ) ) ;
#15876 = AXIS2_PLACEMENT_3D ( 'NONE', #22414, #27196, #1309 ) ;
#15877 = CARTESIAN_POINT ( 'NONE',  ( -8.118202686958138514, 212.8392687619910930, 80.79886208192144181 ) ) ;
#15878 = CARTESIAN_POINT ( 'NONE',  ( 53.27499999726880731, 149.9369285172503510, -15.58253175000000823 ) ) ;
#15879 = CARTESIAN_POINT ( 'NONE',  ( 32.50000000000000000, 155.0000000000000000, 15.00000000000001243 ) ) ;
#15880 = CARTESIAN_POINT ( 'NONE',  ( -6.139770520408369237, 215.5359834540460042, 15.95113791807856884 ) ) ;
#15881 = DIRECTION ( 'NONE',  ( 1.000000000000000000, 0.000000000000000000, 0.000000000000000000 ) ) ;
#15882 = CARTESIAN_POINT ( 'NONE',  ( 64.70000000000000284, 163.5228861582408797, -11.73074641843674470 ) ) ;
#15883 = CARTESIAN_POINT ( 'NONE',  ( 2.000000000000000000, 1.773042676681340968, -2.276824562219559311E-15 ) ) ;
#15884 = CARTESIAN_POINT ( 'NONE',  ( 0.000000000000000000, -0.8865213383406685965, 1.535500000000000531 ) ) ;
#15885 = CARTESIAN_POINT ( 'NONE',  ( -6.220909254589537696, 198.5229672870051161, 81.05113791807856671 ) ) ;
#15886 = DIRECTION ( 'NONE',  ( 0.000000000000000000, 0.7071067811865330288, -0.7071067811865621167 ) ) ;
#15887 = CARTESIAN_POINT ( 'NONE',  ( 39.87499999726880162, 171.3844434931184253, -7.942151717890132712E-15 ) ) ;
#15888 = CARTESIAN_POINT ( 'NONE',  ( -12.00000000000000711, 206.9523078486584780, 98.49886208192143044 ) ) ;
#15889 = CARTESIAN_POINT ( 'NONE',  ( 68.12499999726881583, 155.0000000000000000, 15.58253174999999402 ) ) ;
#15890 = ORIENTED_EDGE ( 'NONE', *, *, #23927, .F. ) ;
#15891 = DIRECTION ( 'NONE',  ( 0.000000000000000000, 0.000000000000000000, -1.000000000000000000 ) ) ;
#15892 = CARTESIAN_POINT ( 'NONE',  ( 39.79999999453762882, 146.4771138417591203, -11.73074641843674470 ) ) ;
#15893 = CARTESIAN_POINT ( 'NONE',  ( -9.680171189290716072, 199.9079932115567146, 5.198862081921434175 ) ) ;
#15894 = CARTESIAN_POINT ( 'NONE',  ( 3.214438021527930012, 2.185595227304852450, -2.682579934988243764 ) ) ;
#15895 = VERTEX_POINT ( 'NONE', #10959 ) ;
#15896 = CARTESIAN_POINT ( 'NONE',  ( 10.00000000000000711, 207.0476921513415220, 96.99886208192143044 ) ) ;
#15897 = AXIS2_PLACEMENT_3D ( 'NONE', #8632, #13577, #800 ) ;
#15898 = CARTESIAN_POINT ( 'NONE',  ( -12.01549611932659722, 210.8513442034533227, 35.64886208192142902 ) ) ;
#15899 = CARTESIAN_POINT ( 'NONE',  ( 2.000000000000000000, 0.000000000000000000, 0.000000000000000000 ) ) ;
#15900 = CARTESIAN_POINT ( 'NONE',  ( -3.044812012440131443, 216.5253028482142952, 43.10113791807857808 ) ) ;
#15901 = ORIENTED_EDGE ( 'NONE', *, *, #12679, .T. ) ;
#15902 = CARTESIAN_POINT ( 'NONE',  ( -6.444103211790928043, 202.2591342207265939, 2.198862081921435063 ) ) ;
#15903 = DIRECTION ( 'NONE',  ( -0.5000000000000006661, -0.8660254037844382635, 0.000000000000000000 ) ) ;
#15904 = ORIENTED_EDGE ( 'NONE', *, *, #17705, .T. ) ;
#15905 = CARTESIAN_POINT ( 'NONE',  ( -4.984841277089891776, 213.7757310962905990, 86.94886208192144750 ) ) ;
#15906 = EDGE_CURVE ( 'NONE', #16399, #536, #16226, .T. ) ;
#15907 = CARTESIAN_POINT ( 'NONE',  ( 4.903702542908601636, 200.1653181626581102, 29.45113791807856529 ) ) ;
#15908 = CARTESIAN_POINT ( 'NONE',  ( 56.31132485994280756, 169.2658477444273331, 4.635254915624208216 ) ) ;
#15909 = ORIENTED_EDGE ( 'NONE', *, *, #3133, .T. ) ;
#15910 = CARTESIAN_POINT ( 'NONE',  ( 33.22499999726881725, 160.0630714827496206, -15.58253175000000823 ) ) ;
#15911 = AXIS2_PLACEMENT_3D ( 'NONE', #28868, #13198, #23756 ) ;
#15912 = CARTESIAN_POINT ( 'NONE',  ( 35.37499999726881583, 155.0000000000000000, -15.58253175000000823 ) ) ;
#15913 = DIRECTION ( 'NONE',  ( 1.000000000000000000, 0.000000000000000000, 0.000000000000000000 ) ) ;
#15914 = CARTESIAN_POINT ( 'NONE',  ( 2.426778023690261410, 199.3768101843759837, 83.60113791807857808 ) ) ;
#15916 = VECTOR ( 'NONE', #3280, 1000.000000000000000 ) ;
#15915 = DIRECTION ( 'NONE',  ( 0.000000000000000000, 0.000000000000000000, 1.000000000000000000 ) ) ;
#15917 = CARTESIAN_POINT ( 'NONE',  ( 45.60000000000000142, 150.2886644046228639, 14.49999999999999645 ) ) ;
#15918 = CARTESIAN_POINT ( 'NONE',  ( -0.05014649552828365914, 215.4116977939061144, 66.24886208192143044 ) ) ;
#15919 = DIRECTION ( 'NONE',  ( -1.000000000000000000, 0.000000000000000000, -0.000000000000000000 ) ) ;
#15920 = VECTOR ( 'NONE', #18174, 1000.000000000000000 ) ;
#15921 = CARTESIAN_POINT ( 'NONE',  ( 48.92499999726881299, 145.8408176439707802, -12.60653300113719588 ) ) ;
#15923 = ORIENTED_EDGE ( 'NONE', *, *, #18090, .F. ) ;
#15922 = CARTESIAN_POINT ( 'NONE',  ( -0.05014649552810635652, 196.4853777576173002, 14.75113791807856423 ) ) ;
#15924 = CARTESIAN_POINT ( 'NONE',  ( -6.500000000000000888, -2.727365451017189635, -5.874157743775032969 ) ) ;
#15925 = CARTESIAN_POINT ( 'NONE',  ( 61.62499999726880162, 171.3844434931184253, -7.942151717890134290E-15 ) ) ;
#15926 = CARTESIAN_POINT ( 'NONE',  ( 76.67499999726881299, 141.7447067706911810, 9.630534252274376428 ) ) ;
#15927 = CARTESIAN_POINT ( 'NONE',  ( -12.01549611932652972, 203.1486557965464499, 72.35113791807857808 ) ) ;
#15928 = CARTESIAN_POINT ( 'NONE',  ( 49.01132485994281041, 142.2402378747194405, 9.270509831248432420 ) ) ;
#15929 = CARTESIAN_POINT ( 'NONE',  ( 6.220909254589536808, 215.4770327129947987, 91.55113791807858092 ) ) ;
#15930 = FACE_OUTER_BOUND ( 'NONE', #32324, .T. ) ;
#15931 = EDGE_LOOP ( 'NONE', ( #27512, #438, #30716, #20660 ) ) ;
#15932 = CARTESIAN_POINT ( 'NONE',  ( -7.456977232089471386, 217.1783343296987709, 53.94886208192144039 ) ) ;
#15933 = CIRCLE ( 'NONE', #27894, 13.00000000000003908 ) ;
#15934 = CARTESIAN_POINT ( 'NONE',  ( 8.062137200540822946, 212.9164362838583315, 66.69886208192143329 ) ) ;
#15935 = CARTESIAN_POINT ( 'NONE',  ( 3.753561863808689836, 218.3979405102790565, 97.40113791807858945 ) ) ;
#15936 = ADVANCED_FACE ( 'NONE', ( #29512 ), #9406, .T. ) ;
#15937 = CARTESIAN_POINT ( 'NONE',  ( 4.000000000000000000, 3.732111120401558708E-16, -3.047499999999999876 ) ) ;
#15938 = CARTESIAN_POINT ( 'NONE',  ( 9.984503880673470277, 203.7031108863295401, 17.15113791807856103 ) ) ;
#15939 = CARTESIAN_POINT ( 'NONE',  ( -6.220909254589682469, 215.4770327129946850, 80.94886208192143329 ) ) ;
#15940 = APPLICATION_CONTEXT ( 'automotive_design' ) ;
#15941 = ORIENTED_EDGE ( 'NONE', *, *, #25545, .F. ) ;
#15942 = CARTESIAN_POINT ( 'NONE',  ( 10.01549611932653860, 210.2015048109876716, 100.8511379180785497 ) ) ;
#15943 = CIRCLE ( 'NONE', #29565, 32.10452846326766974 ) ;
#15944 = ORIENTED_EDGE ( 'NONE', *, *, #12863, .F. ) ;
#15945 = CARTESIAN_POINT ( 'NONE',  ( 117.5000000000000000, 155.0000000000000000, -6.938893903907228378E-15 ) ) ;
#15946 = CARTESIAN_POINT ( 'NONE',  ( -6.500168698208244500, 211.6636982574061676, 62.79886208192144892 ) ) ;
#15947 = ORIENTED_EDGE ( 'NONE', *, *, #32267, .T. ) ;
#15948 = EDGE_CURVE ( 'NONE', #4045, #13342, #10552, .T. ) ;
#15949 = CIRCLE ( 'NONE', #6139, 2.149999999999985256 ) ;
#15950 = CARTESIAN_POINT ( 'NONE',  ( 74.62499999726881583, 138.6155565068815747, -3.929120461958505118E-15 ) ) ;
#15951 = CARTESIAN_POINT ( 'NONE',  ( 125.0000000000000000, 4.592425496802574367E-14, 20.00000000000000000 ) ) ;
#15952 = CARTESIAN_POINT ( 'NONE',  ( 32.50000000000000000, 155.0000000000000000, -6.938893903907228378E-15 ) ) ;
#15953 = CARTESIAN_POINT ( 'NONE',  ( 73.02499999726882152, 149.9369285172503510, -15.58253175000000823 ) ) ;
#15954 = CARTESIAN_POINT ( 'NONE',  ( 2.517493886308900919, 214.5937144450984420, 58.40113791807858235 ) ) ;
#15955 = DIRECTION ( 'NONE',  ( 0.000000000000000000, 0.000000000000000000, 1.000000000000000000 ) ) ;
#15956 = FACE_OUTER_BOUND ( 'NONE', #13680, .T. ) ;
#15957 = ADVANCED_FACE ( 'NONE', ( #13505 ), #16062, .F. ) ;
#15958 = VECTOR ( 'NONE', #23596, 1000.000000000000114 ) ;
#15959 =( NAMED_UNIT ( * ) SI_UNIT ( $, .STERADIAN. ) SOLID_ANGLE_UNIT ( ) );
#15960 = DIRECTION ( 'NONE',  ( 0.000000000000000000, 0.000000000000000000, 1.000000000000000000 ) ) ;
#15961 = PRESENTATION_LAYER_ASSIGNMENT (  '', '', ( #663 ) ) ;
#15962 = CARTESIAN_POINT ( 'NONE',  ( 2.517493886309087436, 199.4062855549015865, 37.59886208192143187 ) ) ;
#15963 = CARTESIAN_POINT ( 'NONE',  ( 10.00000000000000711, 206.9523078486586201, 83.00113791807856956 ) ) ;
#15964 = CARTESIAN_POINT ( 'NONE',  ( -145.0000000000000000, 0.000000000000000000, 20.00000000000000000 ) ) ;
#15965 = CARTESIAN_POINT ( 'NONE',  ( -6.220909254589537696, 198.5229672870051161, 66.05113791807858092 ) ) ;
#15966 = CARTESIAN_POINT ( 'NONE',  ( -3.135527875058821579, 197.5041725223112223, 26.90113791807856813 ) ) ;
#15967 = CARTESIAN_POINT ( 'NONE',  ( -0.05014649552807731031, 198.5883022060938572, 17.75113791807856956 ) ) ;
#15968 = DIRECTION ( 'NONE',  ( -0.000000000000000000, -0.000000000000000000, -1.000000000000000000 ) ) ;
#15969 = MECHANICAL_DESIGN_GEOMETRIC_PRESENTATION_REPRESENTATION (  '', ( #30672 ), #1285 ) ;
#15970 = CARTESIAN_POINT ( 'NONE',  ( 0.000000000000000000, 3.518949890710768802, -4.770489558936219510E-15 ) ) ;
#15971 = CARTESIAN_POINT ( 'NONE',  ( 43.02499999726880020, 149.9369285172503510, -15.58253175000000823 ) ) ;
#15972 = CARTESIAN_POINT ( 'NONE',  ( 12.00000000000000711, 206.9523078486586485, 38.00113791807857666 ) ) ;
#15973 = CARTESIAN_POINT ( 'NONE',  ( -0.3755270751584372513, 206.7692714347155629, 108.3323677711371573 ) ) ;
#15974 = AXIS2_PLACEMENT_3D ( 'NONE', #26102, #18096, #28821 ) ;
#15975 = CARTESIAN_POINT ( 'NONE',  ( -8.062137200540920645, 212.9164362838581894, 84.80113791807856671 ) ) ;
#15976 = CARTESIAN_POINT ( 'NONE',  ( -3.044812012440131443, 216.5253028482142952, 58.10113791807857808 ) ) ;
#15977 = AXIS2_PLACEMENT_3D ( 'NONE', #201, #4799, #7541 ) ;
#15978 = CARTESIAN_POINT ( 'NONE',  ( -12.01549611932659722, 210.8513442034533227, 20.64886208192143613 ) ) ;
#15979 = CARTESIAN_POINT ( 'NONE',  ( -9.984503880673420539, 203.7031108863293980, 29.34886208192143542 ) ) ;
#15980 = CARTESIAN_POINT ( 'NONE',  ( 82.69999999453762030, 167.3344367211045096, 8.961492836873468093 ) ) ;
#15981 = CARTESIAN_POINT ( 'NONE',  ( 0.05014649552807549926, 219.6175466908591716, 67.25113791807856956 ) ) ;
#15982 = CARTESIAN_POINT ( 'NONE',  ( -0.05014649552807731031, 198.5883022060938572, 86.75113791807856956 ) ) ;
#15983 = EDGE_CURVE ( 'NONE', #14298, #14095, #23926, .T. ) ;
#15984 = CARTESIAN_POINT ( 'NONE',  ( 8.062137200540822946, 212.9164362838583315, 54.69886208192143329 ) ) ;
#15985 = DIRECTION ( 'NONE',  ( 0.000000000000000000, -1.000000000000000000, 0.000000000000000000 ) ) ;
#15986 = ORIENTED_EDGE ( 'NONE', *, *, #4938, .T. ) ;
#15987 = CARTESIAN_POINT ( 'NONE',  ( -0.05014649552828442242, 219.6175466908591716, 51.24886208192143755 ) ) ;
#15988 = ORIENTED_EDGE ( 'NONE', *, *, #28019, .T. ) ;
#15989 = EDGE_LOOP ( 'NONE', ( #32565, #19881, #14615, #22944 ) ) ;
#15990 = EDGE_CURVE ( 'NONE', #10897, #13631, #25813, .T. ) ;
#15991 = CARTESIAN_POINT ( 'NONE',  ( 79.97499999726881015, 169.8198683612136222, 4.815267126137181997 ) ) ;
#15992 = DIRECTION ( 'NONE',  ( 0.9396926207859072067, 0.000000000000000000, -0.3420201433256717105 ) ) ;
#15993 = CARTESIAN_POINT ( 'NONE',  ( 59.38867513459481984, 169.2658477444273331, 4.635254915624208216 ) ) ;
#15994 = CARTESIAN_POINT ( 'NONE',  ( 8.015496119326531499, 209.5516654185219636, 43.85113791807856387 ) ) ;
#15995 = AXIS2_PLACEMENT_3D ( 'NONE', #5757, #26882, #6263 ) ;
#15996 = CARTESIAN_POINT ( 'NONE',  ( 6.139770520408223575, 215.5359834540460611, 21.54886208192143826 ) ) ;
#15997 = CARTESIAN_POINT ( 'NONE',  ( 65.57499999726881867, 164.1591823560292198, -12.60653300113719766 ) ) ;
#15998 = ORIENTED_EDGE ( 'NONE', *, *, #13922, .F. ) ;
#15999 = CARTESIAN_POINT ( 'NONE',  ( 41.58867513459482979, 163.8167787843871110, 12.13525491562421621 ) ) ;
#16000 = SURFACE_STYLE_USAGE ( .BOTH. , #5608 ) ;
#16001 = DIRECTION ( 'NONE',  ( -0.000000000000000000, -0.000000000000000000, -1.000000000000000000 ) ) ;
#16002 = CARTESIAN_POINT ( 'NONE',  ( 6.500168698208244500, 202.3363017425938324, 4.298862081921435596 ) ) ;
#16003 = CARTESIAN_POINT ( 'NONE',  ( -3.135527875058821579, 197.5041725223112223, 50.90113791807856813 ) ) ;
#16004 = FILL_AREA_STYLE_COLOUR ( '', #18699 ) ;
#16005 = EDGE_CURVE ( 'NONE', #2085, #4510, #3444, .T. ) ;
#16006 = CARTESIAN_POINT ( 'NONE',  ( -0.05014649552810635652, 196.4853777576173002, 23.75113791807855890 ) ) ;
#16007 = CARTESIAN_POINT ( 'NONE',  ( 82.67499999726879878, 141.7447067706911810, 9.630534252274376428 ) ) ;
#16008 = CARTESIAN_POINT ( 'NONE',  ( 2.426778023690075337, 214.6231898156240447, 93.39886208192143613 ) ) ;
#16009 = CARTESIAN_POINT ( 'NONE',  ( 41.02499999726880731, 149.9369285172503510, -15.58253175000000823 ) ) ;
#16010 = LINE ( 'NONE', #3227, #8390 ) ;
#16011 = CARTESIAN_POINT ( 'NONE',  ( 0.000000000000000000, -2.342598717236903383, 4.057500000000001883 ) ) ;
#16012 = CARTESIAN_POINT ( 'NONE',  ( -3.662846001190052991, 218.4274158808045740, 10.10113791807856742 ) ) ;
#16013 = DIRECTION ( 'NONE',  ( 0.000000000000000000, 0.000000000000000000, -1.000000000000000000 ) ) ;
#16014 = CARTESIAN_POINT ( 'NONE',  ( 55.27499999726881441, 149.9369285172503510, -15.58253175000000823 ) ) ;
#16015 = ADVANCED_FACE ( 'NONE', ( #29179 ), #20874, .T. ) ;
#16016 = CARTESIAN_POINT ( 'NONE',  ( -6.139770520408369237, 215.5359834540460042, 57.95113791807856529 ) ) ;
#16017 = CARTESIAN_POINT ( 'NONE',  ( -6.139770520408368348, 215.5359834540460042, 30.95113791807857240 ) ) ;
#16018 = CARTESIAN_POINT ( 'NONE',  ( -7.500000000000000000, -4.330127018922199866, -1.000000000000000888 ) ) ;
#16019 = CARTESIAN_POINT ( 'NONE',  ( 7.499999999999999112, -4.330127018922205195, -1.000000000000000888 ) ) ;
#16020 = CARTESIAN_POINT ( 'NONE',  ( 3.135527875058981895, 197.5041725223112792, 1.598862081921434530 ) ) ;
#16021 = VECTOR ( 'NONE', #5903, 1000.000000000000000 ) ;
#16022 = CARTESIAN_POINT ( 'NONE',  ( 60.69999999453763451, 167.3344367211045096, 8.961492836873468093 ) ) ;
#16023 = ORIENTED_EDGE ( 'NONE', *, *, #29115, .F. ) ;
#16024 = CARTESIAN_POINT ( 'NONE',  ( -12.01549611932652972, 203.1486557965464499, 39.35113791807856387 ) ) ;
#16025 = EDGE_CURVE ( 'NONE', #25247, #26926, #18624, .T. ) ;
#16026 = CARTESIAN_POINT ( 'NONE',  ( 125.5000000000000000, 229.9533188057739039, -74.95331880577418815 ) ) ;
#16027 = CARTESIAN_POINT ( 'NONE',  ( 8.062137200540822946, 212.9164362838583315, 21.69886208192143684 ) ) ;
#16028 = CARTESIAN_POINT ( 'NONE',  ( 92.60208470531341618, 155.0000000000000000, -13.00000000000002487 ) ) ;
#16029 = EDGE_LOOP ( 'NONE', ( #5706, #13151, #22359, #30246, #17795 ) ) ;
#16030 = CARTESIAN_POINT ( 'NONE',  ( -9.984503880673473830, 210.2968891136704315, 81.65113791807857524 ) ) ;
#16031 = ORIENTED_EDGE ( 'NONE', *, *, #6663, .F. ) ;
#16032 = CARTESIAN_POINT ( 'NONE',  ( 87.50000000000002842, 169.3860439379083402, -5.988074444788474615 ) ) ;
#16033 = CARTESIAN_POINT ( 'NONE',  ( 13.75000000000000888, -23.81569860407206463, -18.00000000000000000 ) ) ;
#16034 = VERTEX_POINT ( 'NONE', #19290 ) ;
#16035 = CARTESIAN_POINT ( 'NONE',  ( -0.05014649552807731031, 198.5883022060938572, 8.751137918078567779 ) ) ;
#16036 = CARTESIAN_POINT ( 'NONE',  ( 12.00000000000000711, 207.0476921513415220, 93.99886208192144466 ) ) ;
#16037 = CARTESIAN_POINT ( 'NONE',  ( 46.37499999726880873, 155.0000000000000000, 15.58253174999999402 ) ) ;
#16038 = ORIENTED_EDGE ( 'NONE', *, *, #14985, .T. ) ;
#16039 = CARTESIAN_POINT ( 'NONE',  ( 49.12499999726880873, 155.0000000000000000, -15.58253175000000823 ) ) ;
#16040 = CARTESIAN_POINT ( 'NONE',  ( 115.4999999999999858, 155.0000000000000000, -6.938893903907228378E-15 ) ) ;
#16041 = DIRECTION ( 'NONE',  ( 1.000000000000000000, 0.000000000000000000, 0.000000000000000000 ) ) ;
#16042 = CARTESIAN_POINT ( 'NONE',  ( 10.01549611932659545, 203.7984951890123853, 79.14886208192142192 ) ) ;
#16043 = CARTESIAN_POINT ( 'NONE',  ( 53.47499999726881015, 160.0630714827496206, -15.58253175000000823 ) ) ;
#16044 = CARTESIAN_POINT ( 'NONE',  ( -6.139770520408369237, 215.5359834540460042, 21.95113791807856884 ) ) ;
#16045 = CARTESIAN_POINT ( 'NONE',  ( -58.50000000000001421, -88.00000000000000000, -20.00000000000000000 ) ) ;
#16046 = EDGE_CURVE ( 'NONE', #4173, #26705, #30707, .T. ) ;
#16047 = EDGE_CURVE ( 'NONE', #14989, #25544, #26290, .T. ) ;
#16048 = CARTESIAN_POINT ( 'NONE',  ( 76.70000000000000284, 163.5228861582408797, -11.73074641843674470 ) ) ;
#16049 = CARTESIAN_POINT ( 'NONE',  ( 10.00000000000000711, 206.9523078486586201, 98.00113791807856956 ) ) ;
#16050 = PLANE ( 'NONE',  #4434 ) ;
#16051 = CARTESIAN_POINT ( 'NONE',  ( -10.01549611932653860, 203.7984951890123284, 87.35113791807854966 ) ) ;
#16052 = CARTESIAN_POINT ( 'NONE',  ( -27.50000000000000355, 0.000000000000000000, 0.000000000000000000 ) ) ;
#16053 = ADVANCED_FACE ( 'NONE', ( #18790 ), #33398, .F. ) ;
#16054 = CARTESIAN_POINT ( 'NONE',  ( 36.57499999726881157, 145.8408176439707802, 12.60653300113718345 ) ) ;
#16055 = EDGE_CURVE ( 'NONE', #5750, #5337, #29571, .T. ) ;
#16056 = CARTESIAN_POINT ( 'NONE',  ( 7.456977232089471386, 196.8216656703012006, 97.44886208192143329 ) ) ;
#16057 = CARTESIAN_POINT ( 'NONE',  ( 79.62499999726881583, 171.3844434931184253, -7.942151717890132712E-15 ) ) ;
#16058 = ORIENTED_EDGE ( 'NONE', *, *, #21057, .T. ) ;
#16059 = DIRECTION ( 'NONE',  ( -0.000000000000000000, -0.000000000000000000, 1.000000000000000000 ) ) ;
#16060 = CARTESIAN_POINT ( 'NONE',  ( 41.79999999453762882, 146.4771138417591203, -11.73074641843674470 ) ) ;
#16061 = PRODUCT_DEFINITION_SHAPE ( 'NONE', 'NONE',  #33718 ) ;
#16062 = CYLINDRICAL_SURFACE ( 'NONE', #30677, 5.200000000000009948 ) ;
#16063 = DIRECTION ( 'NONE',  ( -1.000000000000000000, 0.000000000000000000, 0.000000000000000000 ) ) ;
#16064 = ORIENTED_EDGE ( 'NONE', *, *, #23687, .T. ) ;
#16065 = CARTESIAN_POINT ( 'NONE',  ( -8.118202686958138514, 212.8392687619910930, 92.79886208192144181 ) ) ;
#16066 = CARTESIAN_POINT ( 'NONE',  ( -11.98450388067341876, 203.0532714938636047, 35.34886208192142476 ) ) ;
#16067 = CARTESIAN_POINT ( 'NONE',  ( 6.499999999999999112, -1.280811194704859490, -0.07768058122908397256 ) ) ;
#16068 = CARTESIAN_POINT ( 'NONE',  ( 10.01549611932653860, 210.2015048109876716, 43.85113791807854966 ) ) ;
#16069 = ORIENTED_EDGE ( 'NONE', *, *, #17512, .F. ) ;
#16070 = CARTESIAN_POINT ( 'NONE',  ( 8.015496119326595448, 204.4483345814782638, 1.148862081921434797 ) ) ;
#16071 = LINE ( 'NONE', #20693, #22490 ) ;
#16072 = ORIENTED_EDGE ( 'NONE', *, *, #9737, .F. ) ;
#16073 = CARTESIAN_POINT ( 'NONE',  ( 0.05014649552828262524, 198.5883022060938572, 88.74886208192143044 ) ) ;
#16074 = CARTESIAN_POINT ( 'NONE',  ( -4.903702542908602524, 213.8346818373418898, 33.95113791807857240 ) ) ;
#16075 = CARTESIAN_POINT ( 'NONE',  ( 56.41132485994282320, 167.7597621252805880, 9.270509831248428867 ) ) ;
#16076 = VERTEX_POINT ( 'NONE', #12295 ) ;
#16077 = DIRECTION ( 'NONE',  ( 0.000000000000000000, 0.4999999999999995004, -0.8660254037844389297 ) ) ;
#16078 = CARTESIAN_POINT ( 'NONE',  ( 34.17499999726881299, 164.1591823560292198, 12.60653300113718167 ) ) ;
#16079 = FACE_OUTER_BOUND ( 'NONE', #14544, .T. ) ;
#16080 = CARTESIAN_POINT ( 'NONE',  ( 8.015496119326531499, 209.5516654185219636, 94.85113791807856387 ) ) ;
#16081 = DIRECTION ( 'NONE',  ( -1.000000000000000000, 0.000000000000000000, 0.000000000000000000 ) ) ;
#16082 = CARTESIAN_POINT ( 'NONE',  ( 57.50000000000000000, 155.0000000000000000, 14.49999999999999467 ) ) ;
#16083 = CARTESIAN_POINT ( 'NONE',  ( -4.984841277089891776, 213.7757310962905990, 68.94886208192144750 ) ) ;
#16084 = CARTESIAN_POINT ( 'NONE',  ( 32.50000000000000000, 155.0000000000000000, -15.00000000000002487 ) ) ;
#16085 = CARTESIAN_POINT ( 'NONE',  ( 51.52499999726881441, 169.8198683612136222, -4.815267126137197984 ) ) ;
#16086 = CARTESIAN_POINT ( 'NONE',  ( 8.118202686958039038, 212.8392687619912635, 7.701137918078566180 ) ) ;
#16087 = CARTESIAN_POINT ( 'NONE',  ( 89.50000000000001421, 155.0000000000000000, 70.00000000000000000 ) ) ;
#16088 = CARTESIAN_POINT ( 'NONE',  ( 63.82499999726881867, 168.2552932293087906, 9.630534252274372875 ) ) ;
#16089 = CARTESIAN_POINT ( 'NONE',  ( 77.77499999726880731, 169.8198683612136222, -4.815267126137197984 ) ) ;
#16090 = CARTESIAN_POINT ( 'NONE',  ( 0.05014649552807549926, 219.6175466908591716, 76.25113791807856956 ) ) ;
#16091 = CARTESIAN_POINT ( 'NONE',  ( -65.20000000000000284, -7.347880794884118356E-15, 270.4495957273638282 ) ) ;
#16092 = CARTESIAN_POINT ( 'NONE',  ( 8.062137200540920645, 201.0835637161417822, 98.30113791807858092 ) ) ;
#16093 = CARTESIAN_POINT ( 'NONE',  ( 84.38867513459483405, 140.7341522555726669, -4.635254915624220651 ) ) ;
#16094 = ORIENTED_EDGE ( 'NONE', *, *, #3345, .F. ) ;
#16095 = CARTESIAN_POINT ( 'NONE',  ( 9.736236675708031640, 199.9851607334238963, 61.29886208192144892 ) ) ;
#16096 = CARTESIAN_POINT ( 'NONE',  ( -8.118202686958138514, 212.8392687619910930, 65.79886208192144181 ) ) ;
#16097 = CARTESIAN_POINT ( 'NONE',  ( -7.375838497908014268, 196.7627149292498530, 8.048862081921434708 ) ) ;
#16098 = SHAPE_REPRESENTATION ( 'hex flange nut gradea_iso_ISO - 4161 - M10 - N', ( #2404 ), #11614 ) ;
#16099 = CARTESIAN_POINT ( 'NONE',  ( -67.50001199999999812, 165.3698264620994678, -13.51682963488642919 ) ) ;
#16100 = CARTESIAN_POINT ( 'NONE',  ( -9.984503880673473830, 210.2968891136704315, 12.65113791807856281 ) ) ;
#16101 = CARTESIAN_POINT ( 'NONE',  ( -6.139770520408224463, 198.4640165459539389, 77.04886208192144181 ) ) ;
#16102 = ORIENTED_EDGE ( 'NONE', *, *, #32091, .F. ) ;
#16103 = CARTESIAN_POINT ( 'NONE',  ( -0.05014649552810635652, 196.4853777576173002, 98.75113791807854113 ) ) ;
#16104 = VERTEX_POINT ( 'NONE', #30191 ) ;
#16105 = CARTESIAN_POINT ( 'NONE',  ( 1.525316667890869448E-15, 4.041451884327390331, -2.899999999999999911 ) ) ;
#16106 = CARTESIAN_POINT ( 'NONE',  ( 0.05014649552828262524, 198.5883022060938572, 61.74886208192144466 ) ) ;
#16107 = VERTEX_POINT ( 'NONE', #3791 ) ;
#16108 = CARTESIAN_POINT ( 'NONE',  ( 80.72499999726881015, 140.1801316387863778, -4.815267126137194431 ) ) ;
#16109 = CARTESIAN_POINT ( 'NONE',  ( 5.000000000000000000, 5.258101095580055525E-15, 4.057499999999999218 ) ) ;
#16110 = DIRECTION ( 'NONE',  ( 0.000000000000000000, 0.000000000000000000, 1.000000000000000000 ) ) ;
#16111 = UNCERTAINTY_MEASURE_WITH_UNIT (LENGTH_MEASURE( 1.000000000000000082E-05 ), #32711, 'distance_accuracy_value', 'NONE');
#16112 = CARTESIAN_POINT ( 'NONE',  ( 66.82499999726881867, 141.7447067706911810, -9.630534252274385310 ) ) ;
#16113 = CARTESIAN_POINT ( 'NONE',  ( -6.500168698208129925, 202.3363017425936050, 60.20113791807857240 ) ) ;
#16114 =( LENGTH_UNIT ( ) NAMED_UNIT ( * ) SI_UNIT ( .MILLI., .METRE. ) );
#16115 = AXIS2_PLACEMENT_3D ( 'NONE', #10759, #13630, #10927 ) ;
#16116 = CARTESIAN_POINT ( 'NONE',  ( -9.087479338623817071, 206.5556122393838336, 103.9243378854531130 ) ) ;
#16117 = SURFACE_STYLE_FILL_AREA ( #21563 ) ;
#16118 = DIRECTION ( 'NONE',  ( 1.000000000000000000, -0.000000000000000000, -0.000000000000000000 ) ) ;
#16119 = CARTESIAN_POINT ( 'NONE',  ( 0.05014649552828262524, 198.5883022060938572, 40.74886208192143755 ) ) ;
#16120 = CARTESIAN_POINT ( 'NONE',  ( -3.044812012440131443, 216.5253028482142952, 79.10113791807857808 ) ) ;
#16121 = CARTESIAN_POINT ( 'NONE',  ( 77.50000000000000000, 155.0000000000000000, -6.938893903907228378E-15 ) ) ;
#16122 = CARTESIAN_POINT ( 'NONE',  ( 10.00000000000000711, 206.9523078486586201, 68.00113791807856956 ) ) ;
#16123 = CIRCLE ( 'NONE', #5790, 2.149999999999984812 ) ;
#16124 = CARTESIAN_POINT ( 'NONE',  ( 7.808623696107882317, -4.508310992946666040, -7.999704684617485739 ) ) ;
#16125 = CARTESIAN_POINT ( 'NONE',  ( 0.05014649552807626948, 215.4116977939061144, 19.25113791807856245 ) ) ;
#16126 = CARTESIAN_POINT ( 'NONE',  ( -27.50000000000000711, 6.731471899275991433, -17.54777384619328373 ) ) ;
#16127 = CARTESIAN_POINT ( 'NONE',  ( -3.499999999999997780, -2.020725942163714262, -0.3126073911696551910 ) ) ;
#16128 = CARTESIAN_POINT ( 'NONE',  ( 44.12499999726881583, 155.0000000000000000, 15.58253174999999402 ) ) ;
#16129 = CARTESIAN_POINT ( 'NONE',  ( -9.736236675707914401, 199.9851607334237542, 48.20113791807858661 ) ) ;
#16130 = CARTESIAN_POINT ( 'NONE',  ( 7.894958282449824338, -1.603399432398892266, -7.593838100136980351 ) ) ;
#16131 = CARTESIAN_POINT ( 'NONE',  ( 8.118202686958039038, 212.8392687619912635, 97.70113791807857240 ) ) ;
#16132 = EDGE_CURVE ( 'NONE', #28748, #13563, #27398, .T. ) ;
#16133 = CARTESIAN_POINT ( 'NONE',  ( 8.118202686958039038, 212.8392687619912635, 70.70113791807857240 ) ) ;
#16134 = CARTESIAN_POINT ( 'NONE',  ( 3.662846001189864698, 218.4274158808046593, 27.39886208192143613 ) ) ;
#16135 = CARTESIAN_POINT ( 'NONE',  ( 8.062137200540822946, 212.9164362838583315, 42.69886208192143329 ) ) ;
#16136 = CARTESIAN_POINT ( 'NONE',  ( 79.59999999453762598, 141.2096805137202580, -4.480746418436742040 ) ) ;
#16137 = CARTESIAN_POINT ( 'NONE',  ( 11.98450388067348271, 203.0532714938637753, 74.15113791807857524 ) ) ;
#16138 = CARTESIAN_POINT ( 'NONE',  ( 8.000000000000008882, 206.9523078486586485, 92.00113791807858377 ) ) ;
#16139 = CARTESIAN_POINT ( 'NONE',  ( 8.118202686958138514, 201.1607312380088501, 46.29886208192143471 ) ) ;
#16140 = AXIS2_PLACEMENT_3D ( 'NONE', #29605, #14092, #11710 ) ;
#16141 = LINE ( 'NONE', #13592, #12897 ) ;
#16142 = ORIENTED_EDGE ( 'NONE', *, *, #4170, .F. ) ;
#16143 = CARTESIAN_POINT ( 'NONE',  ( -12.00000000000000711, 206.9523078486584780, 53.49886208192144466 ) ) ;
#16144 = VECTOR ( 'NONE', #14147, 1000.000000000000000 ) ;
#16145 = EDGE_LOOP ( 'NONE', ( #15504, #19296, #25808, #13536, #5, #25844 ) ) ;
#16146 = ORIENTED_EDGE ( 'NONE', *, *, #13907, .T. ) ;
#16147 = AXIS2_PLACEMENT_3D ( 'NONE', #28864, #5520, #11148 ) ;
#16148 = CARTESIAN_POINT ( 'NONE',  ( 75.87499999726881583, 171.3844434931184253, -7.942151717890134290E-15 ) ) ;
#16149 = CARTESIAN_POINT ( 'NONE',  ( 2.000000000000000000, 0.000000000000000000, 0.000000000000000000 ) ) ;
#16150 = DIRECTION ( 'NONE',  ( 1.000000000000000000, 0.000000000000000000, 0.000000000000000000 ) ) ;
#16151 = CARTESIAN_POINT ( 'NONE',  ( 8.015496119326531499, 209.5516654185219636, 55.85113791807856387 ) ) ;
#16152 = DIRECTION ( 'NONE',  ( -0.000000000000000000, -0.000000000000000000, -1.000000000000000000 ) ) ;
#16153 = CARTESIAN_POINT ( 'NONE',  ( 3.135527875058981895, 197.5041725223112792, 34.59886208192143897 ) ) ;
#16154 = CARTESIAN_POINT ( 'NONE',  ( 62.57499999726881867, 145.8408176439707802, 12.60653300113718345 ) ) ;
#16155 = VERTEX_POINT ( 'NONE', #24745 ) ;
#16156 = DIRECTION ( 'NONE',  ( 0.000000000000000000, 0.000000000000000000, 1.000000000000000000 ) ) ;
#16157 = CARTESIAN_POINT ( 'NONE',  ( 0.000000000000000000, 0.000000000000000000, -0.5776712190230133270 ) ) ;
#16158 = CARTESIAN_POINT ( 'NONE',  ( -0.05014649552828365914, 215.4116977939061144, 9.248862081921435774 ) ) ;
#16159 = VECTOR ( 'NONE', #2223, 1000.000000000000000 ) ;
#16160 = CARTESIAN_POINT ( 'NONE',  ( -6.220909254589537696, 198.5229672870051161, 54.05113791807856671 ) ) ;
#16161 = CARTESIAN_POINT ( 'NONE',  ( 82.88867513459484826, 159.8737954434937194, -14.99999999999995559 ) ) ;
#16162 = CARTESIAN_POINT ( 'NONE',  ( 3.044812012440130555, 197.4746971517856764, 35.60113791807857098 ) ) ;
#16163 = CARTESIAN_POINT ( 'NONE',  ( 85.37499999726881583, 155.0000000000000000, -15.58253175000000823 ) ) ;
#16164 = VECTOR ( 'NONE', #1147, 999.9999999999998863 ) ;
#16165 = PRODUCT_CONTEXT ( 'NONE', #2018, 'mechanical' ) ;
#16166 = MECHANICAL_DESIGN_GEOMETRIC_PRESENTATION_REPRESENTATION (  '', ( #5310 ), #6370 ) ;
#16167 = CARTESIAN_POINT ( 'NONE',  ( 4.903702542908435547, 213.8346818373419751, 90.54886208192144181 ) ) ;
#16168 = CARTESIAN_POINT ( 'NONE',  ( 37.82499999726881157, 168.2552932293087906, 9.630534252274372875 ) ) ;
#16169 = DIRECTION ( 'NONE',  ( 1.000000000000000000, -0.000000000000000000, -0.000000000000000000 ) ) ;
#16170 = CARTESIAN_POINT ( 'NONE',  ( 9.736236675707914401, 214.0148392665762458, 19.70113791807856884 ) ) ;
#16171 = LINE ( 'NONE', #21787, #13481 ) ;
#16172 = CARTESIAN_POINT ( 'NONE',  ( 54.87499999726880162, 138.6155565068815463, -3.929120461958505118E-15 ) ) ;
#16173 = CARTESIAN_POINT ( 'NONE',  ( -3.135527875058821579, 197.5041725223112223, 62.90113791807858235 ) ) ;
#16174 = EDGE_CURVE ( 'NONE', #16107, #11012, #6299, .T. ) ;
#16175 = CARTESIAN_POINT ( 'NONE',  ( 9.984503880673473830, 203.7031108863295401, 26.15113791807856813 ) ) ;
#16176 = VECTOR ( 'NONE', #4321, 1000.000000000000000 ) ;
#16177 = CARTESIAN_POINT ( 'NONE',  ( 3.750000000000005329, 6.495190528383288253, 0.000000000000000000 ) ) ;
#16178 = CARTESIAN_POINT ( 'NONE',  ( 54.88867513459484115, 159.8737954434938615, -14.99999999999984190 ) ) ;
#16179 = CARTESIAN_POINT ( 'NONE',  ( 3.135527875058981895, 197.5041725223112792, 13.59886208192143719 ) ) ;
#16180 = CARTESIAN_POINT ( 'NONE',  ( 58.99999999453763166, 155.0000000000000000, 14.49999999999999467 ) ) ;
#16181 = ORIENTED_EDGE ( 'NONE', *, *, #4058, .F. ) ;
#16182 = CARTESIAN_POINT ( 'NONE',  ( 0.05014649552807549926, 219.6175466908591716, 37.25113791807857666 ) ) ;
#16183 = CARTESIAN_POINT ( 'NONE',  ( 77.51132485994280330, 146.1832212156128890, -12.13525491562423042 ) ) ;
#16184 = CARTESIAN_POINT ( 'NONE',  ( 0.05014649552828275708, 196.4853777576173002, 19.74886208192143044 ) ) ;
#16185 = CARTESIAN_POINT ( 'NONE',  ( 59.71132485994280614, 155.0000000000000000, -15.00000000000002487 ) ) ;
#16186 = EDGE_LOOP ( 'NONE', ( #7205, #29985, #25374, #32024, #31692 ) ) ;
#16187 = EDGE_CURVE ( 'NONE', #20653, #28109, #8895, .T. ) ;
#16188 = CARTESIAN_POINT ( 'NONE',  ( 8.062137200540920645, 201.0835637161417822, 83.30113791807858092 ) ) ;
#16189 = AXIS2_PLACEMENT_3D ( 'NONE', #7802, #28585, #5237 ) ;
#16190 = VERTEX_POINT ( 'NONE', #1728 ) ;
#16191 = CIRCLE ( 'NONE', #21641, 3.309499999999999886 ) ;
#16192 = DIRECTION ( 'NONE',  ( 0.000000000000000000, 0.7071067811865475727, 0.7071067811865475727 ) ) ;
#16193 = CARTESIAN_POINT ( 'NONE',  ( 87.50000000000002842, 169.3860439379083402, -5.988074444788474615 ) ) ;
#16194 = ORIENTED_EDGE ( 'NONE', *, *, #12946, .T. ) ;
#16195 = CARTESIAN_POINT ( 'NONE',  ( 6.444103211791042618, 202.2591342207267644, 11.30113791807856671 ) ) ;
#16196 = EDGE_CURVE ( 'NONE', #24528, #30536, #18633, .T. ) ;
#16197 = CARTESIAN_POINT ( 'NONE',  ( -18.00000000000000711, 0.000000000000000000, -17.97459999999999525 ) ) ;
#16198 = CARTESIAN_POINT ( 'NONE',  ( 7.375838497908012492, 217.2372850707501186, 102.5488620819214560 ) ) ;
#16199 = CARTESIAN_POINT ( 'NONE',  ( 46.97499999726881015, 140.1801316387863778, -4.815267126137194431 ) ) ;
#16201 = ORIENTED_EDGE ( 'NONE', *, *, #1028, .F. ) ;
#16200 = AXIS2_PLACEMENT_3D ( 'NONE', #27451, #17737, #9557 ) ;
#16202 = CARTESIAN_POINT ( 'NONE',  ( 50.82499999726880446, 141.7447067706911810, -9.630534252274385310 ) ) ;
#16203 = LINE ( 'NONE', #31712, #6105 ) ;
#16204 = FACE_OUTER_BOUND ( 'NONE', #17679, .T. ) ;
#16205 = FACE_OUTER_BOUND ( 'NONE', #32956, .T. ) ;
#16206 = CARTESIAN_POINT ( 'NONE',  ( 0.05014649552828275708, 196.4853777576173002, 76.74886208192140202 ) ) ;
#16207 = ADVANCED_FACE ( 'NONE', ( #1568 ), #11629, .T. ) ;
#16208 = CARTESIAN_POINT ( 'NONE',  ( 52.97499999726881015, 140.1801316387863778, -4.815267126137194431 ) ) ;
#16209 = CARTESIAN_POINT ( 'NONE',  ( -10.01549611932653860, 203.7984951890123284, 18.35113791807856742 ) ) ;
#16210 = CARTESIAN_POINT ( 'NONE',  ( 73.08867513459483689, 167.7597621252805880, -9.270509831248443078 ) ) ;
#16211 = CARTESIAN_POINT ( 'NONE',  ( -7.456977232089471386, 217.1783343296987709, 74.94886208192143329 ) ) ;
#16212 = CARTESIAN_POINT ( 'NONE',  ( 70.70000000000001705, 163.5228861582408797, -11.73074641843674470 ) ) ;
#16213 = CARTESIAN_POINT ( 'NONE',  ( 127.5000000000000000, 228.4330392262228600, -76.47359838532526055 ) ) ;
#16214 = DIRECTION ( 'NONE',  ( -0.000000000000000000, -0.000000000000000000, 1.000000000000000000 ) ) ;
#16215 = CARTESIAN_POINT ( 'NONE',  ( -3.044812012440131443, 216.5253028482142952, 82.10113791807857808 ) ) ;
#16216 = CARTESIAN_POINT ( 'NONE',  ( 27.50000000000000711, -5.348566131067995499, -17.76938258631346912 ) ) ;
#16217 = CARTESIAN_POINT ( 'NONE',  ( 37.47499999726880304, 160.0630714827496206, -15.58253175000000823 ) ) ;
#16218 = CARTESIAN_POINT ( 'NONE',  ( 7.375838497908012492, 217.2372850707501186, 99.54886208192144181 ) ) ;
#16219 = VECTOR ( 'NONE', #6946, 1000.000000000000000 ) ;
#16220 = CARTESIAN_POINT ( 'NONE',  ( 79.42499999726881299, 168.2552932293087906, -9.630534252274385310 ) ) ;
#16221 = VECTOR ( 'NONE', #10151, 1000.000000000000227 ) ;
#16222 = EDGE_LOOP ( 'NONE', ( #11220, #18050, #28827, #14646, #10967 ) ) ;
#16223 = CARTESIAN_POINT ( 'NONE',  ( 48.51132485994280330, 163.8167787843871110, 12.13525491562421621 ) ) ;
#16224 = CARTESIAN_POINT ( 'NONE',  ( 38.59999999453762598, 168.7903194862797420, 4.480746418436729606 ) ) ;
#16225 = CARTESIAN_POINT ( 'NONE',  ( 3.662846001190051659, 195.5725841191953691, 8.601137918078565647 ) ) ;
#16226 = LINE ( 'NONE', #32070, #15916 ) ;
#16227 = VECTOR ( 'NONE', #26367, 1000.000000000000000 ) ;
#16228 = CARTESIAN_POINT ( 'NONE',  ( 0.6249999999999994449, -8.299410119600885594, -7.298562697733110838 ) ) ;
#16229 = ORIENTED_EDGE ( 'NONE', *, *, #19116, .T. ) ;
#16230 = CARTESIAN_POINT ( 'NONE',  ( -10.01549611932659545, 210.2015048109875011, 95.64886208192143613 ) ) ;
#16231 = CARTESIAN_POINT ( 'NONE',  ( 7.375838497908012492, 217.2372850707501186, 36.54886208192144181 ) ) ;
#16232 = CARTESIAN_POINT ( 'NONE',  ( 0.000000000000000000, 2.428571428571428381, 3.099999999999999645 ) ) ;
#16233 = CARTESIAN_POINT ( 'NONE',  ( -6.139770520408369237, 215.5359834540460042, 51.95113791807857950 ) ) ;
#16234 = ORIENTED_EDGE ( 'NONE', *, *, #23067, .T. ) ;
#16235 = CARTESIAN_POINT ( 'NONE',  ( 0.05014649552828262524, 198.5883022060938572, 16.74886208192143755 ) ) ;
#16236 = EDGE_CURVE ( 'NONE', #17237, #7737, #14351, .T. ) ;
#16237 = EDGE_CURVE ( 'NONE', #13849, #27639, #9061, .T. ) ;
#16238 = DIRECTION ( 'NONE',  ( 0.000000000000000000, 0.000000000000000000, 1.000000000000000000 ) ) ;
#16239 = ORIENTED_EDGE ( 'NONE', *, *, #5564, .F. ) ;
#16240 = CARTESIAN_POINT ( 'NONE',  ( -7.984503880673422316, 204.3529502787951628, 86.34886208192143897 ) ) ;
#16241 = CIRCLE ( 'NONE', #7559, 2.500000000000000000 ) ;
#16242 = ADVANCED_FACE ( 'NONE', ( #14350 ), #16896, .T. ) ;
#16243 = B_SPLINE_CURVE_WITH_KNOTS ( 'NONE', 3,
 ( #5837, #21513, #8573, #3617, #16564, #18963 ),
 .UNSPECIFIED., .F., .F.,
 ( 4, 2, 4 ),
 ( -0.0003963451516553064642, -0.0001381393104116650271, 0.0001200665308319764099 ),
 .UNSPECIFIED. ) ;
#16244 = AXIS2_PLACEMENT_3D ( 'NONE', #10856, #23626, #13565 ) ;
#16245 = CARTESIAN_POINT ( 'NONE',  ( -8.015496119326531499, 204.4483345814780364, 33.35113791807857098 ) ) ;
#16246 = CARTESIAN_POINT ( 'NONE',  ( 55.71132485994280614, 155.0000000000000000, -15.00000000000002487 ) ) ;
#16247 = ORIENTED_EDGE ( 'NONE', *, *, #14920, .T. ) ;
#16248 = CARTESIAN_POINT ( 'NONE',  ( 0.3306966981845720355, 8.469326210127405830, -7.349897473153450989 ) ) ;
#16249 = EDGE_CURVE ( 'NONE', #23405, #20526, #27621, .T. ) ;
#16250 = CARTESIAN_POINT ( 'NONE',  ( 35.47499999726880304, 160.0630714827496206, -15.58253175000000823 ) ) ;
#16251 = DIRECTION ( 'NONE',  ( -0.8660254037844362651, -0.5000000000000041078, 0.000000000000000000 ) ) ;
#16252 = CARTESIAN_POINT ( 'NONE',  ( 8.000000000000008882, 206.9523078486586485, 98.00113791807856956 ) ) ;
#16253 = CIRCLE ( 'NONE', #8642, 4.057500000000000107 ) ;
#16254 = CARTESIAN_POINT ( 'NONE',  ( 52.70000000000000284, 163.5228861582408797, -11.73074641843674470 ) ) ;
#16255 = CARTESIAN_POINT ( 'NONE',  ( -6.444103211790928043, 202.2591342207265939, 74.19886208192143329 ) ) ;
#16256 = CARTESIAN_POINT ( 'NONE',  ( 0.000000000000000000, 0.000000000000000000, 3.469446951953614189E-15 ) ) ;
#16257 = CARTESIAN_POINT ( 'NONE',  ( 58.12499999726881583, 155.0000000000000000, 15.58253174999999402 ) ) ;
#16258 = CARTESIAN_POINT ( 'NONE',  ( 3.135527875058820690, 216.4958274776887492, 13.40113791807856636 ) ) ;
#16259 = CARTESIAN_POINT ( 'NONE',  ( 4.200000000000001954, 2.694222958124178486E-16, 2.200000000000001066 ) ) ;
#16260 = CARTESIAN_POINT ( 'NONE',  ( 64.12499999726881583, 155.0000000000000000, 15.58253174999999402 ) ) ;
#16261 = CARTESIAN_POINT ( 'NONE',  ( 75.17499999726881299, 145.8408176439707802, -12.60653300113719588 ) ) ;
#16262 = CARTESIAN_POINT ( 'NONE',  ( -11.98450388067348804, 210.9467285061362247, 75.65113791807856103 ) ) ;
#16263 = DIRECTION ( 'NONE',  ( -1.000000000000000000, -0.000000000000000000, -0.000000000000000000 ) ) ;
#16264 = AXIS2_PLACEMENT_3D ( 'NONE', #17441, #11827, #24606 ) ;
#16265 = CARTESIAN_POINT ( 'NONE',  ( -3.044812012440131443, 216.5253028482142952, 100.1011379180785781 ) ) ;
#16266 = CARTESIAN_POINT ( 'NONE',  ( 4.000000000000000000, -1.759474945355381958, 3.047500000000001208 ) ) ;
#16267 = VERTEX_POINT ( 'NONE', #4115 ) ;
#16268 = CARTESIAN_POINT ( 'NONE',  ( 9.736236675708031640, 199.9851607334238963, 103.2988620819214560 ) ) ;
#16269 = CIRCLE ( 'NONE', #10318, 3.499999999999999556 ) ;
#16270 = CARTESIAN_POINT ( 'NONE',  ( 11.98450388067341876, 210.9467285061363953, 57.84886208192143187 ) ) ;
#16271 = CARTESIAN_POINT ( 'NONE',  ( -3.044812012439970683, 197.4746971517856196, 67.89886208192143613 ) ) ;
#16272 = CARTESIAN_POINT ( 'NONE',  ( 3.753561863808876797, 195.6020594897209719, 1.598862081921433864 ) ) ;
#16273 = DIRECTION ( 'NONE',  ( -0.5000000000000005551, 0.8660254037844383745, 0.000000000000000000 ) ) ;
#16274 = CARTESIAN_POINT ( 'NONE',  ( -9.984503880673473830, 210.2968891136704315, 24.65113791807856103 ) ) ;
#16275 = CARTESIAN_POINT ( 'NONE',  ( 6.220909254589681581, 198.5229672870052582, 79.44886208192143329 ) ) ;
#16276 = VERTEX_POINT ( 'NONE', #30359 ) ;
#16277 = FACE_OUTER_BOUND ( 'NONE', #783, .T. ) ;
#16278 = ORIENTED_EDGE ( 'NONE', *, *, #827, .F. ) ;
#16279 = CARTESIAN_POINT ( 'NONE',  ( 1.750000000000012879, 3.031088913245524097, 1.502314598737187430E-15 ) ) ;
#16280 = CARTESIAN_POINT ( 'NONE',  ( -2.426778023690076225, 199.3768101843759553, 58.89886208192144323 ) ) ;
#16281 = ORIENTED_EDGE ( 'NONE', *, *, #29925, .T. ) ;
#16282 = CARTESIAN_POINT ( 'NONE',  ( 76.42499999726879878, 141.7447067706911810, 9.630534252274376428 ) ) ;
#16283 = VERTEX_POINT ( 'NONE', #6336 ) ;
#16284 = DIRECTION ( 'NONE',  ( 1.000000000000000000, 0.000000000000000000, 0.000000000000000000 ) ) ;
#16285 = CIRCLE ( 'NONE', #20662, 31.00000000000000000 ) ;
#16286 = CARTESIAN_POINT ( 'NONE',  ( 69.32499999726881867, 164.1591823560292198, -12.60653300113719766 ) ) ;
#16287 = CARTESIAN_POINT ( 'NONE',  ( 2.517493886308900919, 214.5937144450984420, 73.40113791807856103 ) ) ;
#16288 = PRESENTATION_STYLE_ASSIGNMENT (( #24124 ) ) ;
#16289 = CARTESIAN_POINT ( 'NONE',  ( 6.938893903907228378E-15, 31.75426480542944319, -2.456200930618646971 ) ) ;
#16290 = CARTESIAN_POINT ( 'NONE',  ( 36.70000000000000284, 163.5228861582408797, -11.73074641843674470 ) ) ;
#16291 = CARTESIAN_POINT ( 'NONE',  ( 4.984841277089891776, 200.2242689037093726, 40.44886208192144750 ) ) ;
#16292 = CARTESIAN_POINT ( 'NONE',  ( 10.00000000000000711, 206.9523078486586201, 77.00113791807858377 ) ) ;
#16293 = CARTESIAN_POINT ( 'NONE',  ( 3.135527875058820690, 216.4958274776887492, 61.40113791807857524 ) ) ;
#16294 = FACE_OUTER_BOUND ( 'NONE', #3317, .T. ) ;
#16295 = CARTESIAN_POINT ( 'NONE',  ( -8.000000000000008882, 207.0476921513413515, 21.50113791807856956 ) ) ;
#16296 = CARTESIAN_POINT ( 'NONE',  ( 5.000000000000000000, 4.685197434473814759, -5.637851296924623057E-15 ) ) ;
#16297 = CARTESIAN_POINT ( 'NONE',  ( -62.70000000000000284, -88.00000000000000000, 20.00000000000000000 ) ) ;
#16298 = CARTESIAN_POINT ( 'NONE',  ( 46.92499999726881299, 145.8408176439707802, -12.60653300113719588 ) ) ;
#16299 = SHAPE_REPRESENTATION ( 'hex thin nut chamfered gradeab_iso_ISO - 4035 - M36 - N', ( #2404 ), #29629 ) ;
#16300 = CARTESIAN_POINT ( 'NONE',  ( -12.00000000000000711, 207.0476921513413515, 45.50113791807856956 ) ) ;
#16301 = CARTESIAN_POINT ( 'NONE',  ( 7.908230272950877549, -3.123266379887881250, -7.776722524729575703 ) ) ;
#16302 = CARTESIAN_POINT ( 'NONE',  ( -8.118202686958039038, 201.1607312380087080, 90.20113791807857240 ) ) ;
#16303 = B_SPLINE_CURVE_WITH_KNOTS ( 'NONE', 3,
 ( #20678, #27998, #17957, #10123, #20837, #2454, #17435, #25612 ),
 .UNSPECIFIED., .F., .F.,
 ( 4, 2, 2, 4 ),
 ( 0.04438889715320012974, 0.04840678451617883016, 0.05242467187915753057, 0.06046044660511493835 ),
 .UNSPECIFIED. ) ;
#16304 = CARTESIAN_POINT ( 'NONE',  ( -0.05014649552810635652, 196.4853777576173002, 71.75113791807858377 ) ) ;
#16305 = CARTESIAN_POINT ( 'NONE',  ( 9.736236675708031640, 199.9851607334238963, 28.29886208192143826 ) ) ;
#16306 = CARTESIAN_POINT ( 'NONE',  ( -9.984503880673420539, 203.7031108863293980, 38.34886208192143187 ) ) ;
#16307 = CARTESIAN_POINT ( 'NONE',  ( 79.69999999453764872, 142.6655632788954620, -8.961492836873480528 ) ) ;
#16308 = CARTESIAN_POINT ( 'NONE',  ( 12.00000000000000711, 206.9523078486586485, 77.00113791807858377 ) ) ;
#16309 = CARTESIAN_POINT ( 'NONE',  ( -7.984503880673488041, 209.6470497212046098, 84.65113791807856103 ) ) ;
#16310 = CARTESIAN_POINT ( 'NONE',  ( -10.00000000000000711, 206.9523078486584495, 50.49886208192143044 ) ) ;
#16311 = DIRECTION ( 'NONE',  ( 0.000000000000000000, 0.000000000000000000, 1.000000000000000000 ) ) ;
#16312 = VERTEX_POINT ( 'NONE', #30020 ) ;
#16313 = CARTESIAN_POINT ( 'NONE',  ( -7.456977232089471386, 217.1783343296987709, 62.94886208192144039 ) ) ;
#16314 = ORIENTED_EDGE ( 'NONE', *, *, #30373, .F. ) ;
#16315 = CARTESIAN_POINT ( 'NONE',  ( 0.05014649552828262524, 198.5883022060938572, 34.74886208192143755 ) ) ;
#16316 = ORIENTED_EDGE ( 'NONE', *, *, #2946, .T. ) ;
#16317 = CARTESIAN_POINT ( 'NONE',  ( 75.27499999726880731, 149.9369285172503510, -15.58253175000000823 ) ) ;
#16318 = CARTESIAN_POINT ( 'NONE',  ( 53.71132485994279904, 155.0000000000000000, -15.00000000000002487 ) ) ;
#16319 = CYLINDRICAL_SURFACE ( 'NONE', #6215, 2.150000000000004352 ) ;
#16320 = CARTESIAN_POINT ( 'NONE',  ( -8.015496119326531499, 204.4483345814780364, 48.35113791807857098 ) ) ;
#16321 = EDGE_CURVE ( 'NONE', #12674, #24452, #17071, .T. ) ;
#16322 = CARTESIAN_POINT ( 'NONE',  ( -10.01549611932659722, 210.2015048109875011, 32.64886208192143613 ) ) ;
#16323 = CARTESIAN_POINT ( 'NONE',  ( 70.47499999726881015, 149.9369285172503510, 15.58253174999999580 ) ) ;
#16324 = ORIENTED_EDGE ( 'NONE', *, *, #30352, .F. ) ;
#16325 =( LENGTH_UNIT ( ) NAMED_UNIT ( * ) SI_UNIT ( .MILLI., .METRE. ) );
#16326 = CARTESIAN_POINT ( 'NONE',  ( 111.1125082318798007, 155.0000000000000000, 0.000000000000000000 ) ) ;
#16327 = CARTESIAN_POINT ( 'NONE',  ( -8.000000000000008882, 206.9523078486584780, 11.49886208192143577 ) ) ;
#16328 = CARTESIAN_POINT ( 'NONE',  ( -3.135527875058821579, 197.5041725223112223, 47.90113791807857524 ) ) ;
#16329 = CARTESIAN_POINT ( 'NONE',  ( 80.61132485994284025, 159.8737954434934920, 15.00000000000010836 ) ) ;
#16330 = CARTESIAN_POINT ( 'NONE',  ( -3.044812012440131443, 216.5253028482142952, 40.10113791807857098 ) ) ;
#16331 = CARTESIAN_POINT ( 'NONE',  ( 83.07499999726880446, 141.7447067706911810, -9.630534252274385310 ) ) ;
#16332 = SHAPE_DEFINITION_REPRESENTATION ( #27928, #17605 ) ;
#16333 = CARTESIAN_POINT ( 'NONE',  ( -0.05014649552828365914, 215.4116977939061144, 102.2488620819214447 ) ) ;
#16334 = CARTESIAN_POINT ( 'NONE',  ( 37.42499999726881299, 168.2552932293087906, -9.630534252274385310 ) ) ;
#16335 = CARTESIAN_POINT ( 'NONE',  ( 36.28867513459483263, 139.2280666364260071, -4.041636747397287284E-15 ) ) ;
#16336 = CARTESIAN_POINT ( 'NONE',  ( -1.474514954580286030E-14, 206.9977241638431167, -6.000000000000014211 ) ) ;
#16337 = CARTESIAN_POINT ( 'NONE',  ( -7.375838497908182134, 217.2372850707499765, 18.95113791807856529 ) ) ;
#16338 = CARTESIAN_POINT ( 'NONE',  ( 7.779103221381273414, -4.168986698926031131, -7.929128246061905472 ) ) ;
#16339 = CARTESIAN_POINT ( 'NONE',  ( 59.87499999726882294, 171.3844434931184253, -7.942151717890132712E-15 ) ) ;
#16340 = CARTESIAN_POINT ( 'NONE',  ( -3.044812012440131443, 216.5253028482142952, 70.10113791807857808 ) ) ;
#16341 = CARTESIAN_POINT ( 'NONE',  ( -9.984503880673475606, 210.2968891136704315, 36.65113791807856813 ) ) ;
#16342 = CARTESIAN_POINT ( 'NONE',  ( -7.500000000000000000, -1.486698507076798847, -0.09861472150523968583 ) ) ;
#16343 = CARTESIAN_POINT ( 'NONE',  ( 112.4999999999999858, 155.0000000000000000, -12.00000000000001066 ) ) ;
#16344 = CARTESIAN_POINT ( 'NONE',  ( 6.220909254589680693, 198.5229672870052582, 7.448862081921434175 ) ) ;
#16345 = CARTESIAN_POINT ( 'NONE',  ( 57.69999999453762740, 142.6655632788954620, -8.961492836873480528 ) ) ;
#16346 = ORIENTED_EDGE ( 'NONE', *, *, #23687, .F. ) ;
#16347 = CARTESIAN_POINT ( 'NONE',  ( -9.736236675707914401, 199.9851607334237542, 45.20113791807857240 ) ) ;
#16348 = DIRECTION ( 'NONE',  ( 0.000000000000000000, 0.000000000000000000, -1.000000000000000000 ) ) ;
#16349 = CARTESIAN_POINT ( 'NONE',  ( -8.118202686958138514, 212.8392687619910930, 17.79886208192143826 ) ) ;
#16350 = CARTESIAN_POINT ( 'NONE',  ( 92.59660660068168170, 155.0000000000000000, -12.10452846326765020 ) ) ;
#16351 = EDGE_LOOP ( 'NONE', ( #116, #8707, #1085, #31422 ) ) ;
#16352 = CARTESIAN_POINT ( 'NONE',  ( -6.220909254589537696, 198.5229672870051161, 84.05113791807855250 ) ) ;
#16353 = ORIENTED_EDGE ( 'NONE', *, *, #20444, .T. ) ;
#16354 = CARTESIAN_POINT ( 'NONE',  ( -60.00000000000000000, -7.347880794884118356E-15, 270.4495957273638282 ) ) ;
#16355 = CARTESIAN_POINT ( 'NONE',  ( 0.04050535873993867109, -7.919512791578240396, -6.573129608219095310 ) ) ;
#16356 = EDGE_LOOP ( 'NONE', ( #21931, #4638 ) ) ;
#16357 = CARTESIAN_POINT ( 'NONE',  ( 6.444103211791042618, 202.2591342207267644, 20.30113791807857027 ) ) ;
#16358 = DIRECTION ( 'NONE',  ( 0.000000000000000000, 0.000000000000000000, -1.000000000000000000 ) ) ;
#16359 = ADVANCED_FACE ( 'NONE', ( #14680 ), #24906, .T. ) ;
#16360 = CARTESIAN_POINT ( 'NONE',  ( 7.456977232089471386, 196.8216656703012006, 103.4488620819214475 ) ) ;
#16361 = CARTESIAN_POINT ( 'NONE',  ( 50.57499999726881157, 145.8408176439707802, 12.60653300113718345 ) ) ;
#16362 = VERTEX_POINT ( 'NONE', #17235 ) ;
#16363 = CARTESIAN_POINT ( 'NONE',  ( 57.22499999726879594, 160.0630714827496206, -15.58253175000000823 ) ) ;
#16364 = DIRECTION ( 'NONE',  ( 0.000000000000000000, 0.000000000000000000, -1.000000000000000000 ) ) ;
#16365 = AXIS2_PLACEMENT_3D ( 'NONE', #33528, #22965, #33363 ) ;
#16366 = DIRECTION ( 'NONE',  ( -0.000000000000000000, -0.000000000000000000, 1.000000000000000000 ) ) ;
#16367 = EDGE_CURVE ( 'NONE', #20973, #4513, #5429, .T. ) ;
#16368 = CARTESIAN_POINT ( 'NONE',  ( 8.118202686958138514, 201.1607312380088501, 94.29886208192144181 ) ) ;
#16369 = CARTESIAN_POINT ( 'NONE',  ( 55.77499999726881441, 169.8198683612136222, -4.815267126137197984 ) ) ;
#16370 = CARTESIAN_POINT ( 'NONE',  ( -8.062137200540920645, 212.9164362838581894, 24.80113791807857027 ) ) ;
#16371 = DIRECTION ( 'NONE',  ( -1.000000000000000000, -0.000000000000000000, -0.000000000000000000 ) ) ;
#16372 = CARTESIAN_POINT ( 'NONE',  ( -11.98450388067341876, 203.0532714938636047, 83.34886208192143897 ) ) ;
#16373 = EDGE_CURVE ( 'NONE', #28318, #780, #12978, .T. ) ;
#16374 = CARTESIAN_POINT ( 'NONE',  ( 70.80000000000001137, 167.3344367211045096, -8.961492836873482304 ) ) ;
#16375 = CARTESIAN_POINT ( 'NONE',  ( 40.48867513459481415, 142.2402378747194405, -9.270509831248439525 ) ) ;
#16376 = CARTESIAN_POINT ( 'NONE',  ( 8.551039143100592099, 208.8253170565643302, -0.4549153643320029139 ) ) ;
#16377 = CARTESIAN_POINT ( 'NONE',  ( 6.139770520408368348, 198.4640165459539674, 98.45113791807854398 ) ) ;
#16378 = DIRECTION ( 'NONE',  ( 0.000000000000000000, 0.000000000000000000, -1.000000000000000000 ) ) ;
#16379 = CARTESIAN_POINT ( 'NONE',  ( 39.27499999726880020, 149.9369285172503510, -15.58253175000000823 ) ) ;
#16380 = CARTESIAN_POINT ( 'NONE',  ( 6.220909254589536808, 215.4770327129947702, 40.55113791807855250 ) ) ;
#16381 = CARTESIAN_POINT ( 'NONE',  ( 77.42499999726882720, 168.2552932293087906, -9.630534252274385310 ) ) ;
#16382 = ORIENTED_EDGE ( 'NONE', *, *, #4719, .T. ) ;
#16383 = DIRECTION ( 'NONE',  ( -1.000000000000000000, 1.776356839400250465E-15, 0.000000000000000000 ) ) ;
#16384 = CARTESIAN_POINT ( 'NONE',  ( 43.89999999453761603, 150.2886644046228639, -14.50000000000000888 ) ) ;
#16385 = CARTESIAN_POINT ( 'NONE',  ( -7.456977232089304408, 196.8216656703010301, 24.05113791807857027 ) ) ;
#16386 = EDGE_CURVE ( 'NONE', #7333, #23334, #20650, .T. ) ;
#16387 = CARTESIAN_POINT ( 'NONE',  ( -3.499999999999999556, -0.6807265984995714003, -2.870648692803531077 ) ) ;
#16388 = FACE_OUTER_BOUND ( 'NONE', #3049, .T. ) ;
#16389 = EDGE_LOOP ( 'NONE', ( #31215, #4681 ) ) ;
#16390 = CARTESIAN_POINT ( 'NONE',  ( 10.00000000000000711, 207.0476921513415220, 93.99886208192144466 ) ) ;
#16391 = VECTOR ( 'NONE', #20157, 1000.000000000000000 ) ;
#16392 = CARTESIAN_POINT ( 'NONE',  ( -3.753561863808878130, 218.3979405102790281, 36.09886208192143187 ) ) ;
#16393 = DIRECTION ( 'NONE',  ( -1.000000000000000000, 0.000000000000000000, -0.000000000000000000 ) ) ;
#16394 = CARTESIAN_POINT ( 'NONE',  ( -10.00000000000000711, 207.0476921513413515, 51.50113791807857666 ) ) ;
#16395 = EDGE_CURVE ( 'NONE', #1453, #11260, #25917, .T. ) ;
#16396 = VERTEX_POINT ( 'NONE', #25748 ) ;
#16397 = CARTESIAN_POINT ( 'NONE',  ( -6.444103211790928043, 202.2591342207265939, 11.19886208192143506 ) ) ;
#16398 = CARTESIAN_POINT ( 'NONE',  ( 50.28867513459483263, 139.2280666364260071, -4.041636747397287284E-15 ) ) ;
#16399 = VERTEX_POINT ( 'NONE', #20473 ) ;
#16400 = CARTESIAN_POINT ( 'NONE',  ( 4.984841277089891776, 200.2242689037093726, 97.44886208192143329 ) ) ;
#16401 = EDGE_CURVE ( 'NONE', #31219, #25762, #20299, .T. ) ;
#16402 = CARTESIAN_POINT ( 'NONE',  ( -8.000000000000008882, 207.0476921513413515, 42.50113791807857666 ) ) ;
#16403 = FACE_OUTER_BOUND ( 'NONE', #12433, .T. ) ;
#16404 = ORIENTED_EDGE ( 'NONE', *, *, #11642, .T. ) ;
#16405 = CARTESIAN_POINT ( 'NONE',  ( 39.02499999726880731, 149.9369285172503510, -15.58253175000000823 ) ) ;
#16406 =( BOUNDED_CURVE ( )  B_SPLINE_CURVE ( 2, ( #29083, #14202, #7978, #5731, #1260, #16756, #11485, #18362, #11655, #11817, #13242 ),
 .UNSPECIFIED., .F., .T. ) 
 B_SPLINE_CURVE_WITH_KNOTS ( ( 3, 2, 2, 2, 2, 3 ),
 ( 0.4285714285714284366, 0.4321428571428569954, 0.4357142857142856651, 0.4392857142857141683, 0.4428571428571427271, 0.4464285714285712858 ),
 .UNSPECIFIED. ) 
 CURVE ( )  GEOMETRIC_REPRESENTATION_ITEM ( )  RATIONAL_B_SPLINE_CURVE ( ( 1.000000000000000666, 0.9510565162951526430, 1.000000000000000000, 0.9510565162951534202, 1.000000000000000000, 0.9510565162951534202, 1.000000000000000000, 0.9510565162951534202, 1.000000000000000000, 0.9510565162951549745, 0.9999999999999984457 ) ) 
 REPRESENTATION_ITEM ( '' )  );
#16407 = CARTESIAN_POINT ( 'NONE',  ( 3.044812012439969795, 216.5253028482143520, 54.39886208192143613 ) ) ;
#16408 = CARTESIAN_POINT ( 'NONE',  ( 88.12499999726880162, 155.0000000000000000, 15.58253174999999402 ) ) ;
#16409 = CARTESIAN_POINT ( 'NONE',  ( 2.000000000000000000, 0.000000000000000000, 0.000000000000000000 ) ) ;
#16410 = CARTESIAN_POINT ( 'NONE',  ( -2.517493886308901807, 199.4062855549015012, 95.90113791807857524 ) ) ;
#16411 = CARTESIAN_POINT ( 'NONE',  ( -58.50000000000000000, -88.00000000000000000, 38.00000000000000000 ) ) ;
#16412 = CARTESIAN_POINT ( 'NONE',  ( 54.39999999999999147, 150.2886644046228639, -14.50000000000000888 ) ) ;
#16413 = CARTESIAN_POINT ( 'NONE',  ( 4.984841277089891776, 200.2242689037093726, 76.44886208192143329 ) ) ;
#16414 = DIRECTION ( 'NONE',  ( 0.000000000000000000, 0.000000000000000000, -1.000000000000000000 ) ) ;
#16415 = EDGE_CURVE ( 'NONE', #18184, #18269, #31217, .T. ) ;
#16416 = CARTESIAN_POINT ( 'NONE',  ( 60.92499999726882010, 145.8408176439707802, -12.60653300113719588 ) ) ;
#16417 = CARTESIAN_POINT ( 'NONE',  ( 6.220909254589536808, 215.4770327129947987, 10.55113791807856494 ) ) ;
#16418 = FACE_OUTER_BOUND ( 'NONE', #5532, .T. ) ;
#16419 = AXIS2_PLACEMENT_3D ( 'NONE', #15087, #23102, #33490 ) ;
#16420 = CARTESIAN_POINT ( 'NONE',  ( 60.82499999726881157, 141.7447067706911810, -9.630534252274387086 ) ) ;
#16421 = CARTESIAN_POINT ( 'NONE',  ( 73.87499999726881583, 171.3844434931184253, -7.942151717890132712E-15 ) ) ;
#16422 = CARTESIAN_POINT ( 'NONE',  ( 3.662846001190051659, 195.5725841191953691, 80.60113791807857808 ) ) ;
#16423 = EDGE_CURVE ( 'NONE', #29398, #6338, #32291, .T. ) ;
#16424 = CARTESIAN_POINT ( 'NONE',  ( 3.044812012440130555, 197.4746971517856764, 101.6011379180785781 ) ) ;
#16425 = CARTESIAN_POINT ( 'NONE',  ( 84.58867513459483689, 146.1832212156128890, -12.13525491562423042 ) ) ;
#16426 = ORIENTED_EDGE ( 'NONE', *, *, #17276, .F. ) ;
#16427 = CARTESIAN_POINT ( 'NONE',  ( -12.00000000000000711, 206.9523078486584780, 104.4988620819214304 ) ) ;
#16428 = CARTESIAN_POINT ( 'NONE',  ( 3.662846001189864698, 218.4274158808046593, 63.39886208192144323 ) ) ;
#16429 = CARTESIAN_POINT ( 'NONE',  ( 6.139770520408223575, 215.5359834540460611, 66.54886208192144181 ) ) ;
#16430 = CARTESIAN_POINT ( 'NONE',  ( -12.01549611932659722, 210.8513442034533227, 5.648862081921434353 ) ) ;
#16431 = DIRECTION ( 'NONE',  ( 1.000000000000000000, 0.000000000000000000, 0.000000000000000000 ) ) ;
#16432 = CARTESIAN_POINT ( 'NONE',  ( 3.135527875058820690, 216.4958274776887492, 19.40113791807856813 ) ) ;
#16433 = EDGE_CURVE ( 'NONE', #8233, #5762, #9916, .T. ) ;
#16434 = CARTESIAN_POINT ( 'NONE',  ( 10.01549611932659545, 203.7984951890123853, 91.14886208192140771 ) ) ;
#16435 = ORIENTED_EDGE ( 'NONE', *, *, #25101, .T. ) ;
#16436 = PRODUCT_DEFINITION_FORMATION_WITH_SPECIFIED_SOURCE ( 'ANY', '', #14870, .NOT_KNOWN. ) ;
#16437 = DIRECTION ( 'NONE',  ( -1.000000000000000000, 0.000000000000000000, 0.000000000000000000 ) ) ;
#16438 = ORIENTED_EDGE ( 'NONE', *, *, #7107, .F. ) ;
#16439 = DIRECTION ( 'NONE',  ( 0.000000000000000000, 0.000000000000000000, 1.000000000000000000 ) ) ;
#16440 = CARTESIAN_POINT ( 'NONE',  ( 8.015496119326595448, 204.4483345814782638, 64.14886208192143613 ) ) ;
#16441 = VERTEX_POINT ( 'NONE', #30875 ) ;
#16442 = CARTESIAN_POINT ( 'NONE',  ( 75.62499999726881583, 171.3844434931184253, -7.942151717890134290E-15 ) ) ;
#16443 = ORIENTED_EDGE ( 'NONE', *, *, #6230, .T. ) ;
#16444 = FACE_OUTER_BOUND ( 'NONE', #28412, .T. ) ;
#16445 = VECTOR ( 'NONE', #873, 1000.000000000000000 ) ;
#16446 = AXIS2_PLACEMENT_3D ( 'NONE', #6892, #20350, #9963 ) ;
#16447 = CARTESIAN_POINT ( 'NONE',  ( 69.92499999726881299, 164.1591823560292198, 12.60653300113718167 ) ) ;
#16448 = CARTESIAN_POINT ( 'NONE',  ( 2.517493886308900919, 214.5937144450984420, 67.40113791807856103 ) ) ;
#16449 =( NAMED_UNIT ( * ) PLANE_ANGLE_UNIT ( ) SI_UNIT ( $, .RADIAN. ) );
#16450 = CARTESIAN_POINT ( 'NONE',  ( 2.000000000000000000, -0.8865213383406685965, 1.535500000000000531 ) ) ;
#16451 = CARTESIAN_POINT ( 'NONE',  ( 38.19999999999998153, 142.6655632788954620, -8.961492836873480528 ) ) ;
#16452 = CARTESIAN_POINT ( 'NONE',  ( 6.500168698208244500, 202.3363017425938324, 46.29886208192144892 ) ) ;
#16453 = CARTESIAN_POINT ( 'NONE',  ( 9.984503880673470277, 203.7031108863295401, 80.15113791807858945 ) ) ;
#16454 = CARTESIAN_POINT ( 'NONE',  ( 0.05014649552810505201, 217.5146222423826714, 70.25113791807858377 ) ) ;
#16455 = EDGE_CURVE ( 'NONE', #31129, #17462, #11630, .T. ) ;
#16456 = VECTOR ( 'NONE', #28750, 1000.000000000000000 ) ;
#16457 = CARTESIAN_POINT ( 'NONE',  ( 105.9028607166213192, 155.0000000000000000, 0.000000000000000000 ) ) ;
#16458 = CARTESIAN_POINT ( 'NONE',  ( -6.500168698208129925, 202.3363017425936050, 24.20113791807856529 ) ) ;
#16459 = CARTESIAN_POINT ( 'NONE',  ( 0.6250000000000013323, 8.299410119600871383, -7.298562697733108173 ) ) ;
#16460 = CARTESIAN_POINT ( 'NONE',  ( 6.500000000000001776, -5.204170427930421283E-15, -5.592027715088708995 ) ) ;
#16461 = CARTESIAN_POINT ( 'NONE',  ( 42.92499999726881299, 145.8408176439707802, -12.60653300113719588 ) ) ;
#16462 = CARTESIAN_POINT ( 'NONE',  ( 12.01549611932652972, 210.8513442034534933, 46.85113791807857098 ) ) ;
#16463 = EDGE_CURVE ( 'NONE', #22313, #19626, #31755, .T. ) ;
#16464 = CARTESIAN_POINT ( 'NONE',  ( 6.220909254589536808, 215.4770327129947702, 91.55113791807858092 ) ) ;
#16465 = ADVANCED_FACE ( 'NONE', ( #28315 ), #37, .F. ) ;
#16466 = CARTESIAN_POINT ( 'NONE',  ( 9.984503880673473830, 203.7031108863295401, 71.15113791807857524 ) ) ;
#16467 = CARTESIAN_POINT ( 'NONE',  ( 3.662846001189864698, 218.4274158808046593, 30.39886208192143613 ) ) ;
#16468 = CARTESIAN_POINT ( 'NONE',  ( 8.062137200540822946, 212.9164362838583315, 36.69886208192143329 ) ) ;
#16469 = CARTESIAN_POINT ( 'NONE',  ( 82.89999999453760893, 159.7113355953771077, 14.49999999999999289 ) ) ;
#16470 = AXIS2_PLACEMENT_3D ( 'NONE', #7230, #32772, #11832 ) ;
#16471 = CARTESIAN_POINT ( 'NONE',  ( 3.753561863808689836, 218.3979405102790565, 79.40113791807858945 ) ) ;
#16472 = CARTESIAN_POINT ( 'NONE',  ( 6.500168698208129925, 211.6636982574063381, 97.70113791807858661 ) ) ;
#16473 = AXIS2_PLACEMENT_3D ( 'NONE', #24577, #6173, #31576 ) ;
#16474 = CARTESIAN_POINT ( 'NONE',  ( -3.135527875058982783, 216.4958274776886924, 57.09886208192143187 ) ) ;
#16475 = AXIS2_PLACEMENT_3D ( 'NONE', #15952, #11643, #1580 ) ;
#16476 = CARTESIAN_POINT ( 'NONE',  ( 6.602753909532903087, 5.319290460493537154, -7.792447862505332168 ) ) ;
#16477 = ORIENTED_EDGE ( 'NONE', *, *, #25823, .F. ) ;
#16478 = CARTESIAN_POINT ( 'NONE',  ( 3.753561863808876797, 195.6020594897209719, 58.59886208192143897 ) ) ;
#16479 = ORIENTED_EDGE ( 'NONE', *, *, #31409, .T. ) ;
#16480 = CARTESIAN_POINT ( 'NONE',  ( -6.444103211790928043, 202.2591342207265939, 35.19886208192144039 ) ) ;
#16481 = ORIENTED_EDGE ( 'NONE', *, *, #24941, .F. ) ;
#16482 = CARTESIAN_POINT ( 'NONE',  ( 78.67499999726879878, 141.7447067706911810, 9.630534252274376428 ) ) ;
#16483 = LINE ( 'NONE', #5599, #12434 ) ;
#16484 = AXIS2_PLACEMENT_3D ( 'NONE', #17132, #28203, #15751 ) ;
#16485 = CARTESIAN_POINT ( 'NONE',  ( -6.837824896291514243, 3.947820044545427454, -6.564402953523716278 ) ) ;
#16486 = CARTESIAN_POINT ( 'NONE',  ( -6.500168698208129925, 202.3363017425936050, 48.20113791807858661 ) ) ;
#16487 = FACE_OUTER_BOUND ( 'NONE', #2798, .T. ) ;
#16488 = CARTESIAN_POINT ( 'NONE',  ( 8.062137200540822946, 212.9164362838583315, 36.69886208192143329 ) ) ;
#16489 = CARTESIAN_POINT ( 'NONE',  ( 66.37499999726881583, 155.0000000000000000, 15.58253174999999402 ) ) ;
#16490 = EDGE_LOOP ( 'NONE', ( #25295, #16703 ) ) ;
#16491 = CARTESIAN_POINT ( 'NONE',  ( 61.88867513459483405, 150.1262045565064227, 15.00000000000001599 ) ) ;
#16492 = CIRCLE ( 'NONE', #13773, 2.149999999999996803 ) ;
#16493 = CARTESIAN_POINT ( 'NONE',  ( -67.50000000000000000, 155.0000000000000000, 6.938893903907228378E-15 ) ) ;
#16494 = FACE_OUTER_BOUND ( 'NONE', #33285, .T. ) ;
#16495 = CARTESIAN_POINT ( 'NONE',  ( 6.444103211790928043, 211.7408657792734061, 18.69886208192143684 ) ) ;
#16496 = CARTESIAN_POINT ( 'NONE',  ( 8.118202686958039038, 212.8392687619912635, 52.70113791807857240 ) ) ;
#16497 = CARTESIAN_POINT ( 'NONE',  ( 80.31132485994280046, 169.2658477444273331, 4.635254915624208216 ) ) ;
#16498 = CARTESIAN_POINT ( 'NONE',  ( -9.984503880673473830, 210.2968891136704315, 36.65113791807855392 ) ) ;
#16499 = CARTESIAN_POINT ( 'NONE',  ( 83.77499999726880731, 169.8198683612136222, -4.815267126137197984 ) ) ;
#16500 = AXIS2_PLACEMENT_3D ( 'NONE', #6847, #19800, #11961 ) ;
#16501 = APPLICATION_PROTOCOL_DEFINITION ( 'draft international standard', 'automotive_design', 1998, #22452 ) ;
#16502 = CARTESIAN_POINT ( 'NONE',  ( -7.984503880673422316, 204.3529502787951628, 104.3488620819214532 ) ) ;
#16503 = CARTESIAN_POINT ( 'NONE',  ( 35.42499999726880588, 168.2552932293087906, -9.630534252274385310 ) ) ;
#16504 = LINE ( 'NONE', #3561, #7303 ) ;
#16505 = CARTESIAN_POINT ( 'NONE',  ( 37.78867513459481842, 155.0000000000000000, 15.00000000000001243 ) ) ;
#16506 = CARTESIAN_POINT ( 'NONE',  ( 3.753561863808689836, 218.3979405102790565, 19.40113791807856813 ) ) ;
#16507 = CARTESIAN_POINT ( 'NONE',  ( 4.406466114817131796, -6.116179640279303165, -7.446478553994418270 ) ) ;
#16508 = CARTESIAN_POINT ( 'NONE',  ( 62.47499999726881725, 149.9369285172503510, 15.58253174999999580 ) ) ;
#16509 = CARTESIAN_POINT ( 'NONE',  ( -10.01549611932653860, 203.7984951890123284, 63.35113791807857098 ) ) ;
#16510 = CARTESIAN_POINT ( 'NONE',  ( -3.135527875058821579, 197.5041725223112223, 38.90113791807857524 ) ) ;
#16511 = CARTESIAN_POINT ( 'NONE',  ( -7.500000000000000888, -3.640541674360520119, -0.7158139487964623182 ) ) ;
#16512 = FACE_OUTER_BOUND ( 'NONE', #15575, .T. ) ;
#16513 = CARTESIAN_POINT ( 'NONE',  ( -12.01549611932659722, 210.8513442034533227, 5.648862081921434353 ) ) ;
#16514 = CARTESIAN_POINT ( 'NONE',  ( 0.05014649552828275014, 196.4853777576173002, 7.748862081921435774 ) ) ;
#16515 = CARTESIAN_POINT ( 'NONE',  ( 64.29999999453762882, 167.3344367211045096, -8.961492836873482304 ) ) ;
#16516 = ORIENTED_EDGE ( 'NONE', *, *, #33319, .F. ) ;
#16517 = CARTESIAN_POINT ( 'NONE',  ( -12.00000000000000711, 207.0476921513413515, 48.50113791807856956 ) ) ;
#16518 = CARTESIAN_POINT ( 'NONE',  ( -7.984503880673488041, 209.6470497212046098, 69.65113791807856103 ) ) ;
#16519 = CARTESIAN_POINT ( 'NONE',  ( 0.000000000000000000, 1.649999999999999911, 2.066666666667000385 ) ) ;
#16520 = CARTESIAN_POINT ( 'NONE',  ( 10.00000000000000711, 207.0476921513415220, 21.99886208192143755 ) ) ;
#16521 = LINE ( 'NONE', #3578, #12871 ) ;
#16522 = VERTEX_POINT ( 'NONE', #33590 ) ;
#16523 = CIRCLE ( 'NONE', #4004, 32.10452846326769816 ) ;
#16524 = CARTESIAN_POINT ( 'NONE',  ( -8.062137200540920645, 212.9164362838581894, 84.80113791807856671 ) ) ;
#16525 = EDGE_LOOP ( 'NONE', ( #8575, #9418, #2092, #14977 ) ) ;
#16526 = PLANE ( 'NONE',  #6424 ) ;
#16527 = CARTESIAN_POINT ( 'NONE',  ( 32.50000000000000000, 155.0000000000000000, -15.00000000000002487 ) ) ;
#16528 = ORIENTED_EDGE ( 'NONE', *, *, #28137, .T. ) ;
#16529 = CARTESIAN_POINT ( 'NONE',  ( -8.000000000000008882, 207.0476921513413515, 21.50113791807856956 ) ) ;
#16530 = ADVANCED_BREP_SHAPE_REPRESENTATION ( '', ( #1232, #2404 ), #33431 ) ;
#16531 = CARTESIAN_POINT ( 'NONE',  ( -58.82891977373553516, 194.9228321189716837, -2.483646737656201253 ) ) ;
#16532 = CARTESIAN_POINT ( 'NONE',  ( 3.044812012439969795, 216.5253028482143520, 6.398862081921435241 ) ) ;
#16533 = CARTESIAN_POINT ( 'NONE',  ( 48.07499999726881867, 168.2552932293087906, 9.630534252274372875 ) ) ;
#16534 = EDGE_LOOP ( 'NONE', ( #16831, #216, #3837, #1294 ) ) ;
#16535 = CARTESIAN_POINT ( 'NONE',  ( 57.02499999726882152, 149.9369285172503510, -15.58253175000000823 ) ) ;
#16536 = LINE ( 'NONE', #18933, #32768 ) ;
#16537 = CARTESIAN_POINT ( 'NONE',  ( 7.703928834700305650, 4.447865386531936416, -7.917997657324733929 ) ) ;
#16538 = COLOUR_RGB ( '', 0.09019608, 0.27058824, 0.51372549) ;
#16539 = DIRECTION ( 'NONE',  ( 1.000000000000000000, 0.000000000000000000, 0.000000000000000000 ) ) ;
#16540 = CARTESIAN_POINT ( 'NONE',  ( -6.139770520408224463, 198.4640165459539389, 92.04886208192139918 ) ) ;
#16541 = CARTESIAN_POINT ( 'NONE',  ( 62.87499999726881583, 138.6155565068815463, -3.929120461958505118E-15 ) ) ;
#16542 = CARTESIAN_POINT ( 'NONE',  ( -8.118202686958039038, 201.1607312380087080, 24.20113791807856884 ) ) ;
#16543 = LINE ( 'NONE', #18939, #12153 ) ;
#16544 = CARTESIAN_POINT ( 'NONE',  ( 11.98450388067341876, 210.9467285061363953, 75.84886208192143897 ) ) ;
#16545 = MECHANICAL_DESIGN_GEOMETRIC_PRESENTATION_REPRESENTATION (  '', ( #3463 ), #11118 ) ;
#16546 = CARTESIAN_POINT ( 'NONE',  ( 71.90000000000000568, 141.2096805137202580, 4.480746418436733158 ) ) ;
#16547 = CARTESIAN_POINT ( 'NONE',  ( 61.71132485994280614, 155.0000000000000000, -15.00000000000002487 ) ) ;
#16548 = CARTESIAN_POINT ( 'NONE',  ( -6.500000000000000000, 3.752776749732564809, -6.064240316920399110 ) ) ;
#16549 = CARTESIAN_POINT ( 'NONE',  ( 10.01549611932653860, 210.2015048109876716, 91.85113791807853545 ) ) ;
#16550 = CARTESIAN_POINT ( 'NONE',  ( 32.98867513459481415, 163.8167787843871110, -12.13525491562423397 ) ) ;
#16551 = AXIS2_PLACEMENT_3D ( 'NONE', #12223, #9326, #30115 ) ;
#16552 = CARTESIAN_POINT ( 'NONE',  ( 44.07499999726881157, 168.2552932293087906, 9.630534252274372875 ) ) ;
#16553 = CARTESIAN_POINT ( 'NONE',  ( 0.05014649552810505201, 217.5146222423826714, 37.25113791807855534 ) ) ;
#16554 = CARTESIAN_POINT ( 'NONE',  ( 73.92499999726881299, 164.1591823560292198, 12.60653300113718167 ) ) ;
#16555 = ORIENTED_EDGE ( 'NONE', *, *, #32627, .F. ) ;
#16556 = CARTESIAN_POINT ( 'NONE',  ( 77.50000000000000000, 155.0000000000000000, -7.500000000000022204 ) ) ;
#16557 = CARTESIAN_POINT ( 'NONE',  ( 42.79999999453762882, 163.5228861582408797, 11.73074641843673049 ) ) ;
#16558 = CARTESIAN_POINT ( 'NONE',  ( -3.662846001190052991, 218.4274158808045740, 16.10113791807856742 ) ) ;
#16559 = CARTESIAN_POINT ( 'NONE',  ( 40.21132485994280614, 170.7719333635740497, -7.904646289410545231E-15 ) ) ;
#16560 = ADVANCED_FACE ( 'NONE', ( #15020 ), #31206, .F. ) ;
#16561 = CARTESIAN_POINT ( 'NONE',  ( 0.3483149870578491347, -8.861353789385031376, -7.493854785173814648 ) ) ;
#16562 = ORIENTED_EDGE ( 'NONE', *, *, #15827, .F. ) ;
#16563 = CARTESIAN_POINT ( 'NONE',  ( 7.456977232089471386, 196.8216656703012006, 31.44886208192143684 ) ) ;
#16564 = CARTESIAN_POINT ( 'NONE',  ( -10.08243921202409688, 207.8094824920489714, 102.5360034692371869 ) ) ;
#16565 = EDGE_CURVE ( 'NONE', #8868, #3834, #27407, .T. ) ;
#16566 = CARTESIAN_POINT ( 'NONE',  ( 3.135527875058820690, 216.4958274776887492, 49.40113791807857524 ) ) ;
#16567 = ORIENTED_EDGE ( 'NONE', *, *, #7049, .T. ) ;
#16568 = CARTESIAN_POINT ( 'NONE',  ( 2.517493886309087436, 199.4062855549015865, 13.59886208192143719 ) ) ;
#16569 = B_SPLINE_CURVE_WITH_KNOTS ( 'NONE', 3,
 ( #9421, #19815, #27642, #32586, #30209, #2102 ),
 .UNSPECIFIED., .F., .F.,
 ( 4, 2, 4 ),
 ( 8.673617379884035472E-19, 0.0003352299596252163519, 0.0006704599192504318364 ),
 .UNSPECIFIED. ) ;
#16570 = PRODUCT_DEFINITION_CONTEXT ( 'detailed design', #916, 'design' ) ;
#16571 = CARTESIAN_POINT ( 'NONE',  ( 51.31132485994280046, 140.7341522555726669, -4.635254915624220651 ) ) ;
#16572 = ORIENTED_EDGE ( 'NONE', *, *, #20497, .T. ) ;
#16573 = CARTESIAN_POINT ( 'NONE',  ( -8.000000000000008882, 206.9523078486584780, 98.49886208192143044 ) ) ;
#16574 = CARTESIAN_POINT ( 'NONE',  ( 8.015496119326531499, 209.5516654185219636, 40.85113791807856387 ) ) ;
#16575 = CARTESIAN_POINT ( 'NONE',  ( 33.97499999726881725, 169.8198683612136222, 4.815267126137181997 ) ) ;
#16576 = ORIENTED_EDGE ( 'NONE', *, *, #28419, .F. ) ;
#16577 = CARTESIAN_POINT ( 'NONE',  ( 39.52499999726881441, 169.8198683612136222, -4.815267126137197984 ) ) ;
#16578 = CARTESIAN_POINT ( 'NONE',  ( 10.00000000000000711, 207.0476921513415220, 57.99886208192143044 ) ) ;
#16579 = CARTESIAN_POINT ( 'NONE',  ( 41.37499999726880873, 155.0000000000000000, -15.58253175000000823 ) ) ;
#16580 = DIRECTION ( 'NONE',  ( -0.000000000000000000, -0.000000000000000000, -1.000000000000000000 ) ) ;
#16581 = CARTESIAN_POINT ( 'NONE',  ( 7.984503880673485376, 204.3529502787953902, 98.15113791807856103 ) ) ;
#16582 = APPLICATION_CONTEXT ( 'automotive_design' ) ;
#16583 = CARTESIAN_POINT ( 'NONE',  ( 56.80000000000000426, 167.3344367211045096, -8.961492836873482304 ) ) ;
#16584 = CARTESIAN_POINT ( 'NONE',  ( -7.984503880673422316, 204.3529502787951628, 68.34886208192142476 ) ) ;
#16585 = ADVANCED_FACE ( 'NONE', ( #7367 ), #30130, .T. ) ;
#16586 = CARTESIAN_POINT ( 'NONE',  ( 57.12499999726880873, 155.0000000000000000, -15.58253175000000823 ) ) ;
#16588 = ORIENTED_EDGE ( 'NONE', *, *, #9880, .T. ) ;
#16587 = CARTESIAN_POINT ( 'NONE',  ( -3.135527875058821579, 197.5041725223112223, 14.90113791807856636 ) ) ;
#16589 = CARTESIAN_POINT ( 'NONE',  ( 37.41132485994281609, 142.2402378747194405, -9.270509831248439525 ) ) ;
#16590 = CARTESIAN_POINT ( 'NONE',  ( 67.42499999726879878, 168.2552932293087906, -9.630534252274387086 ) ) ;
#16591 = CARTESIAN_POINT ( 'NONE',  ( 77.47499999726878173, 160.0630714827496206, -15.58253175000000823 ) ) ;
#16592 = CARTESIAN_POINT ( 'NONE',  ( -3.753561863808691168, 195.6020594897209435, 77.90113791807856103 ) ) ;
#16593 = CARTESIAN_POINT ( 'NONE',  ( -8.118202686958039038, 201.1607312380087080, 99.20113791807858661 ) ) ;
#16594 = EDGE_CURVE ( 'NONE', #5188, #22989, #19346, .T. ) ;
#16595 = CARTESIAN_POINT ( 'NONE',  ( -125.0000000000000000, -25.00000000000000000, -35.00000000000000000 ) ) ;
#16596 = ORIENTED_EDGE ( 'NONE', *, *, #7454, .T. ) ;
#16597 = CARTESIAN_POINT ( 'NONE',  ( -0.05014649552828403384, 217.5146222423826714, 6.248862081921433109 ) ) ;
#16598 = CARTESIAN_POINT ( 'NONE',  ( -9.736236675708031640, 214.0148392665760753, 62.79886208192144892 ) ) ;
#16599 = CARTESIAN_POINT ( 'NONE',  ( -10.01549611932659545, 210.2015048109875011, 62.64886208192144323 ) ) ;
#16600 = CARTESIAN_POINT ( 'NONE',  ( 12.01549611932659367, 203.1486557965466773, 4.148862081921434353 ) ) ;
#16601 = CARTESIAN_POINT ( 'NONE',  ( 95.70416941062676131, 155.0000000000000000, 32.00000000000005684 ) ) ;
#16602 = CARTESIAN_POINT ( 'NONE',  ( -3.044812012440131443, 216.5253028482142952, 19.10113791807856742 ) ) ;
#16603 = CARTESIAN_POINT ( 'NONE',  ( -8.062137200540822946, 201.0835637161416400, 92.19886208192143329 ) ) ;
#16604 = ORIENTED_EDGE ( 'NONE', *, *, #12643, .T. ) ;
#16605 = EDGE_CURVE ( 'NONE', #8327, #3502, #24610, .T. ) ;
#16606 = DIRECTION ( 'NONE',  ( -1.000000000000000000, -0.000000000000000000, -0.000000000000000000 ) ) ;
#16607 = EDGE_LOOP ( 'NONE', ( #21877, #1398, #31375, #18430, #21309 ) ) ;
#16608 = CARTESIAN_POINT ( 'NONE',  ( 72.78867513459482552, 155.0000000000000000, -15.00000000000002487 ) ) ;
#16609 =( BOUNDED_CURVE ( )  B_SPLINE_CURVE ( 2, ( #20996, #15383, #5325, #2944, #5658, #23555, #13327, #26116, #23719, #31393, #5160 ),
 .UNSPECIFIED., .F., .T. ) 
 B_SPLINE_CURVE_WITH_KNOTS ( ( 3, 2, 2, 2, 2, 3 ),
 ( 0.7678571428571426827, 0.7714285714285712414, 0.7749999999999998002, 0.7785714285714284699, 0.7821428571428570287, 0.7857142857142856984 ),
 .UNSPECIFIED. ) 
 CURVE ( )  GEOMETRIC_REPRESENTATION_ITEM ( )  RATIONAL_B_SPLINE_CURVE ( ( 1.000000000000001554, 0.9510565162951518658, 1.000000000000000000, 0.9510565162951534202, 1.000000000000000000, 0.9510565162951534202, 1.000000000000000000, 0.9510565162951534202, 1.000000000000000000, 0.9510565162951534202, 1.000000000000000000 ) ) 
 REPRESENTATION_ITEM ( '' )  );
#16610 = CARTESIAN_POINT ( 'NONE',  ( 2.517493886309087436, 199.4062855549015865, 73.59886208192142476 ) ) ;
#16611 = ORIENTED_EDGE ( 'NONE', *, *, #33299, .T. ) ;
#16612 = CARTESIAN_POINT ( 'NONE',  ( 81.62499999726880162, 171.3844434931184253, -7.942151717890134290E-15 ) ) ;
#16613 = ORIENTED_EDGE ( 'NONE', *, *, #30340, .F. ) ;
#16614 = DIRECTION ( 'NONE',  ( -0.5526942671207061286, -0.1536855300543007730, -0.8190908404712107238 ) ) ;
#16615 = CARTESIAN_POINT ( 'NONE',  ( 67.02499999726882152, 149.9369285172503510, -15.58253175000000823 ) ) ;
#16616 = EDGE_CURVE ( 'NONE', #15495, #20097, #24194, .T. ) ;
#16617 = CARTESIAN_POINT ( 'NONE',  ( 4.984841277089725686, 213.7757310962907411, 70.55113791807856671 ) ) ;
#16618 =( NAMED_UNIT ( * ) SI_UNIT ( $, .STERADIAN. ) SOLID_ANGLE_UNIT ( ) );
#16619 = CARTESIAN_POINT ( 'NONE',  ( -64.50000000000000000, 0.000000000000000000, 20.00000000000000000 ) ) ;
#16620 = SHAPE_REPRESENTATION_RELATIONSHIP ( 'NONE' , 'NONE' ,  #32622, #33198 ) ;
#16621 = CARTESIAN_POINT ( 'NONE',  ( 32.89999999999999858, 168.7903194862797420, -4.480746418436745593 ) ) ;
#16622 = CARTESIAN_POINT ( 'NONE',  ( -7.984503880673422316, 204.3529502787951628, 47.34886208192143897 ) ) ;
#16623 = ADVANCED_FACE ( 'NONE', ( #28974 ), #8204, .T. ) ;
#16624 = CARTESIAN_POINT ( 'NONE',  ( -3.135527875058821579, 197.5041725223112223, 86.90113791807857524 ) ) ;
#16625 = CARTESIAN_POINT ( 'NONE',  ( 10.01549611932653860, 210.2015048109876716, 64.85113791807857808 ) ) ;
#16626 = CARTESIAN_POINT ( 'NONE',  ( -60.00000000000000000, -7.347880794884118356E-15, 35.00000000000000000 ) ) ;
#16627 = CARTESIAN_POINT ( 'NONE',  ( -4.984841277089726574, 200.2242689037092305, 21.05113791807857027 ) ) ;
#16628 = CARTESIAN_POINT ( 'NONE',  ( 0.000000000000000000, 0.000000000000000000, -10.00000000000000000 ) ) ;
#16629 = CARTESIAN_POINT ( 'NONE',  ( -4.574783636564603739, 5.228990388888020036, -6.171384342982724647 ) ) ;
#16630 = CARTESIAN_POINT ( 'NONE',  ( 43.92499999726881299, 164.1591823560292198, 12.60653300113718167 ) ) ;
#16631 = CARTESIAN_POINT ( 'NONE',  ( 0.05014649552807549926, 219.6175466908591716, 52.25113791807857666 ) ) ;
#16632 = CARTESIAN_POINT ( 'NONE',  ( 7.499999999999999112, 0.7577384720672989404, -7.446470314338469620 ) ) ;
#16633 = CARTESIAN_POINT ( 'NONE',  ( 6.139770520408368348, 198.4640165459539674, 92.45113791807857240 ) ) ;
#16634 = CARTESIAN_POINT ( 'NONE',  ( -3.044812012440131443, 216.5253028482142952, 73.10113791807857808 ) ) ;
#16635 = CARTESIAN_POINT ( 'NONE',  ( 7.375838497908012492, 217.2372850707501186, 30.54886208192144181 ) ) ;
#16636 = CARTESIAN_POINT ( 'NONE',  ( 6.220909254589680693, 198.5229672870052582, 34.44886208192143329 ) ) ;
#16637 = CARTESIAN_POINT ( 'NONE',  ( 87.09999999453764019, 150.2886644046228639, 14.49999999999999645 ) ) ;
#16638 = CARTESIAN_POINT ( 'NONE',  ( 7.375838497908181246, 196.7627149292499666, 77.45113791807855819 ) ) ;
#16639 = CARTESIAN_POINT ( 'NONE',  ( 10.00000000000000711, 206.9523078486586201, -0.9988620819214343305 ) ) ;
#16640 = CARTESIAN_POINT ( 'NONE',  ( 6.139770520408223575, 215.5359834540460611, 57.54886208192142050 ) ) ;
#16641 = VERTEX_POINT ( 'NONE', #20975 ) ;
#16642 = CARTESIAN_POINT ( 'NONE',  ( -12.01549611932659722, 210.8513442034533227, 65.64886208192142192 ) ) ;
#16643 = ORIENTED_EDGE ( 'NONE', *, *, #19129, .F. ) ;
#16644 = CARTESIAN_POINT ( 'NONE',  ( 73.27499999726882152, 149.9369285172503510, -15.58253175000000823 ) ) ;
#16645 = CARTESIAN_POINT ( 'NONE',  ( -8.000000000000008882, 206.9523078486584780, 44.49886208192143755 ) ) ;
#16646 = VERTEX_POINT ( 'NONE', #13965 ) ;
#16647 = EDGE_CURVE ( 'NONE', #16283, #4641, #5643, .T. ) ;
#16648 = ADVANCED_FACE ( 'NONE', ( #24361, #2919 ), #31694, .F. ) ;
#16649 = AXIS2_PLACEMENT_3D ( 'NONE', #3984, #14205, #11488 ) ;
#16650 = CARTESIAN_POINT ( 'NONE',  ( 81.37499999726881583, 155.0000000000000000, -15.58253175000000823 ) ) ;
#16651 = CARTESIAN_POINT ( 'NONE',  ( 115.4999999999999858, 155.0000000000000000, -6.938893903907228378E-15 ) ) ;
#16652 = CIRCLE ( 'NONE', #14493, 19.99999999999998934 ) ;
#16653 = DIRECTION ( 'NONE',  ( 0.5526942671207055735, 0.1536855300543024383, 0.8190908404712107238 ) ) ;
#16654 = CARTESIAN_POINT ( 'NONE',  ( -6.500168698208129925, 202.3363017425936050, 51.20113791807857240 ) ) ;
#16655 = EDGE_CURVE ( 'NONE', #25537, #2009, #10020, .T. ) ;
#16656 = B_SPLINE_CURVE_WITH_KNOTS ( 'NONE', 3,
 ( #30580, #25633, #7243, #31376 ),
 .UNSPECIFIED., .F., .F.,
 ( 4, 4 ),
 ( 0.001859822337438910272, 0.001914709330258871581 ),
 .UNSPECIFIED. ) ;
#16657 = CARTESIAN_POINT ( 'NONE',  ( -8.062137200540822946, 201.0835637161416400, 32.19886208192143329 ) ) ;
#16658 = CARTESIAN_POINT ( 'NONE',  ( 66.47499999726881015, 149.9369285172503510, 15.58253174999999580 ) ) ;
#16659 = ORIENTED_EDGE ( 'NONE', *, *, #33256, .T. ) ;
#16660 = CIRCLE ( 'NONE', #23749, 2.000000000000000888 ) ;
#16661 = CARTESIAN_POINT ( 'NONE',  ( 99.17200000000002547, 0.000000000000000000, 0.000000000000000000 ) ) ;
#16662 = DIRECTION ( 'NONE',  ( 0.000000000000000000, 0.000000000000000000, -1.000000000000000000 ) ) ;
#16663 = DIRECTION ( 'NONE',  ( 0.000000000000000000, 0.000000000000000000, -1.000000000000000000 ) ) ;
#16664 = CARTESIAN_POINT ( 'NONE',  ( -0.05014649552828365914, 215.4116977939061144, 15.24886208192143577 ) ) ;
#16665 = EDGE_CURVE ( 'NONE', #30462, #6526, #10011, .T. ) ;
#16666 = CARTESIAN_POINT ( 'NONE',  ( 6.220909254589536808, 215.4770327129947702, 61.55113791807858092 ) ) ;
#16667 = CARTESIAN_POINT ( 'NONE',  ( -0.05014649552810635652, 196.4853777576173002, 32.75113791807856956 ) ) ;
#16668 = CARTESIAN_POINT ( 'NONE',  ( 86.07499999726880446, 168.2552932293087906, 9.630534252274372875 ) ) ;
#16669 = ITEM_DEFINED_TRANSFORMATION ( 'NONE', 'NONE', #28979,  #2404 ) ;
#16670 = CARTESIAN_POINT ( 'NONE',  ( 7.984503880673422316, 209.6470497212048372, 102.8488620819214390 ) ) ;
#16671 = CARTESIAN_POINT ( 'NONE',  ( 47.62499999726880162, 171.3844434931184253, -7.942151717890132712E-15 ) ) ;
#16672 = LINE ( 'NONE', #27069, #20914 ) ;
#16673 = LINE ( 'NONE', #3391, #27756 ) ;
#16674 = CARTESIAN_POINT ( 'NONE',  ( 12.00000000000000711, 206.9523078486586485, 23.00113791807856600 ) ) ;
#16675 = CARTESIAN_POINT ( 'NONE',  ( -125.0000000000000000, 25.00000000000000000, 20.00000000000000000 ) ) ;
#16676 = CARTESIAN_POINT ( 'NONE',  ( 6.220909254589536808, 215.4770327129947702, 70.55113791807856671 ) ) ;
#16677 = CARTESIAN_POINT ( 'NONE',  ( 9.984503880673473830, 203.7031108863295401, 41.15113791807856813 ) ) ;
#16678 = AXIS2_PLACEMENT_3D ( 'NONE', #22477, #6809, #32868 ) ;
#16679 = DIRECTION ( 'NONE',  ( 0.9366133782696128840, 0.000000000000000000, 0.3503646381220332229 ) ) ;
#16680 = CARTESIAN_POINT ( 'NONE',  ( 85.68867513459483121, 159.8737954434936341, 14.99999999999997158 ) ) ;
#16681 = CARTESIAN_POINT ( 'NONE',  ( -0.05014649552828442242, 219.6175466908591716, 6.248862081921433997 ) ) ;
#16682 = CARTESIAN_POINT ( 'NONE',  ( -6.139770520408224463, 198.4640165459539105, 5.048862081921435596 ) ) ;
#16683 = CARTESIAN_POINT ( 'NONE',  ( 67.49999999453763166, 139.7537977485451393, -4.138211985947621020E-15 ) ) ;
#16684 = ORIENTED_EDGE ( 'NONE', *, *, #26662, .F. ) ;
#16685 = CARTESIAN_POINT ( 'NONE',  ( 7.375838497908181246, 196.7627149292499666, 50.45113791807855819 ) ) ;
#16686 = CARTESIAN_POINT ( 'NONE',  ( -2.517493886308901807, 199.4062855549015012, 65.90113791807856103 ) ) ;
#16687 = CARTESIAN_POINT ( 'NONE',  ( 32.50000000000000000, 155.0000000000000000, 15.00000000000001243 ) ) ;
#16688 = CARTESIAN_POINT ( 'NONE',  ( 8.118202686958138514, 201.1607312380088501, 34.29886208192143471 ) ) ;
#16689 = CARTESIAN_POINT ( 'NONE',  ( 3.811597179862312057, -5.304926841629219680, -0.01956314070068839589 ) ) ;
#16690 = VECTOR ( 'NONE', #13524, 1000.000000000000000 ) ;
#16691 = ORIENTED_EDGE ( 'NONE', *, *, #5363, .T. ) ;
#16692 = CARTESIAN_POINT ( 'NONE',  ( 9.984503880673470277, 203.7031108863295401, 80.15113791807858945 ) ) ;
#16693 = ORIENTED_EDGE ( 'NONE', *, *, #23945, .T. ) ;
#16694 = CARTESIAN_POINT ( 'NONE',  ( 0.000000000000000000, 1.773042676681340968, -2.276824562219559311E-15 ) ) ;
#16695 = DIRECTION ( 'NONE',  ( -1.000000000000000000, -0.000000000000000000, -0.000000000000000000 ) ) ;
#16696 = ORIENTED_EDGE ( 'NONE', *, *, #25629, .T. ) ;
#16697 = CARTESIAN_POINT ( 'NONE',  ( -7.984503880673488041, 209.6470497212046098, 24.65113791807857169 ) ) ;
#16698 = AXIS2_PLACEMENT_3D ( 'NONE', #18330, #28724, #5381 ) ;
#16699 = CARTESIAN_POINT ( 'NONE',  ( -60.38337337305365793, 194.9660334721754111, 1.652118058477962004 ) ) ;
#16700 = CIRCLE ( 'NONE', #10738, 4.199999999999988631 ) ;
#16701 = CARTESIAN_POINT ( 'NONE',  ( -10.01549611932659722, 210.2015048109875011, 8.648862081921436129 ) ) ;
#16702 = CARTESIAN_POINT ( 'NONE',  ( 51.97499999726881725, 169.8198683612136222, 4.815267126137181997 ) ) ;
#16703 = ORIENTED_EDGE ( 'NONE', *, *, #28307, .F. ) ;
#16704 = CARTESIAN_POINT ( 'NONE',  ( 54.32499999726880446, 145.8408176439707802, 12.60653300113718345 ) ) ;
#16705 = CARTESIAN_POINT ( 'NONE',  ( -8.015496119326531499, 204.4483345814780364, 51.35113791807857098 ) ) ;
#16706 = CARTESIAN_POINT ( 'NONE',  ( 7.500000000000000000, 4.330127018922190096, -7.422398894150032511 ) ) ;
#16707 = DIRECTION ( 'NONE',  ( -1.000000000000000000, -4.625929269271485914E-16, 0.000000000000000000 ) ) ;
#16708 = CARTESIAN_POINT ( 'NONE',  ( 10.01549611932659545, 203.7984951890123853, 88.14886208192143613 ) ) ;
#16709 = CARTESIAN_POINT ( 'NONE',  ( 58.17499999726881299, 164.1591823560292198, 12.60653300113718167 ) ) ;
#16710 = CARTESIAN_POINT ( 'NONE',  ( 8.118202686958039038, 212.8392687619912635, 25.70113791807856529 ) ) ;
#16711 = DIRECTION ( 'NONE',  ( 1.000000000000000000, 0.000000000000000000, 0.000000000000000000 ) ) ;
#16712 = CARTESIAN_POINT ( 'NONE',  ( 9.736236675708031640, 199.9851607334238963, 76.29886208192142760 ) ) ;
#16713 = CIRCLE ( 'NONE', #8031, 5.249999999999991118 ) ;
#16714 = CARTESIAN_POINT ( 'NONE',  ( 72.70000000000000284, 163.5228861582408797, -11.73074641843674470 ) ) ;
#16715 = CARTESIAN_POINT ( 'NONE',  ( 65.68867513459483121, 159.8737954434934920, 15.00000000000010836 ) ) ;
#16716 = DIRECTION ( 'NONE',  ( 0.000000000000000000, 0.000000000000000000, -1.000000000000000000 ) ) ;
#16717 = CARTESIAN_POINT ( 'NONE',  ( 3.135527875058820690, 216.4958274776887492, 97.40113791807858945 ) ) ;
#16718 = CARTESIAN_POINT ( 'NONE',  ( 27.50000000000000355, -14.58598892539968972, -15.91652008647648842 ) ) ;
#16719 = CARTESIAN_POINT ( 'NONE',  ( 44.77499999726881441, 140.1801316387863778, 4.815267126137185549 ) ) ;
#16720 = CARTESIAN_POINT ( 'NONE',  ( 3.044812012440130555, 197.4746971517856764, 41.60113791807857808 ) ) ;
#16721 = CARTESIAN_POINT ( 'NONE',  ( 77.12499999726881583, 155.0000000000000000, -15.58253175000000823 ) ) ;
#16722 = ORIENTED_EDGE ( 'NONE', *, *, #31660, .F. ) ;
#16723 = CARTESIAN_POINT ( 'NONE',  ( -4.613983237546153582, 6.452243898629808960, -7.591546097228401457 ) ) ;
#16724 = CARTESIAN_POINT ( 'NONE',  ( 46.49999999453762456, 170.2462022514548323, -7.872454543227099337E-15 ) ) ;
#16725 = CARTESIAN_POINT ( 'NONE',  ( 3.662846001190051659, 195.5725841191953691, 17.60113791807856742 ) ) ;
#16726 = AXIS2_PLACEMENT_3D ( 'NONE', #4053, #17343, #9170 ) ;
#16727 = CARTESIAN_POINT ( 'NONE',  ( -2.352990130084580066E-16, 8.660254037844390851, -10.00000000000000000 ) ) ;
#16728 = AXIS2_PLACEMENT_3D ( 'NONE', #1486, #17488, #20393 ) ;
#16729 = DIRECTION ( 'NONE',  ( -1.000000000000000000, -0.000000000000000000, -0.000000000000000000 ) ) ;
#16730 = ORIENTED_EDGE ( 'NONE', *, *, #32029, .F. ) ;
#16731 = CARTESIAN_POINT ( 'NONE',  ( 0.05014649552828288198, 194.3824533091408000, 46.74886208192143755 ) ) ;
#16732 = FACE_OUTER_BOUND ( 'NONE', #14604, .T. ) ;
#16733 = CARTESIAN_POINT ( 'NONE',  ( -8.062137200540920645, 212.9164362838581894, 54.80113791807857382 ) ) ;
#16734 = EDGE_LOOP ( 'NONE', ( #5063, #26915, #27584, #3292, #22377, #7956 ) ) ;
#16735 = VECTOR ( 'NONE', #24594, 1000.000000000000114 ) ;
#16736 = CARTESIAN_POINT ( 'NONE',  ( -0.05014649552828365914, 215.4116977939061144, 18.24886208192143755 ) ) ;
#16737 = VECTOR ( 'NONE', #20121, 1000.000000000000000 ) ;
#16738 = DIRECTION ( 'NONE',  ( 1.000000000000000000, 1.804112415015879378E-16, 0.000000000000000000 ) ) ;
#16739 = ORIENTED_EDGE ( 'NONE', *, *, #1292, .F. ) ;
#16740 = CARTESIAN_POINT ( 'NONE',  ( 4.984841277089891776, 200.2242689037093726, 103.4488620819214475 ) ) ;
#16741 = FACE_OUTER_BOUND ( 'NONE', #33681, .T. ) ;
#16742 = CARTESIAN_POINT ( 'NONE',  ( 6.444103211791042618, 202.2591342207267644, 44.30113791807857382 ) ) ;
#16743 = DIRECTION ( 'NONE',  ( 1.000000000000000000, -0.000000000000000000, -0.000000000000000000 ) ) ;
#16744 = ORIENTED_EDGE ( 'NONE', *, *, #30419, .T. ) ;
#16745 = CARTESIAN_POINT ( 'NONE',  ( 37.72499999726881015, 169.8198683612136222, 4.815267126137181997 ) ) ;
#16746 = CIRCLE ( 'NONE', #2079, 1.000000000000000222 ) ;
#16747 = CARTESIAN_POINT ( 'NONE',  ( 8.118202686958138514, 201.1607312380088501, 64.29886208192144181 ) ) ;
#16748 = CARTESIAN_POINT ( 'NONE',  ( 41.57499999726881157, 164.1591823560292198, -12.60653300113719766 ) ) ;
#16749 = CARTESIAN_POINT ( 'NONE',  ( -125.0000000000000000, 0.000000000000000000, -20.00000000000000000 ) ) ;
#16750 = CARTESIAN_POINT ( 'NONE',  ( 4.984841277089725686, 213.7757310962907411, 97.55113791807858092 ) ) ;
#16751 = PRODUCT ( 'pad arm right_right', 'pad arm right_right', '', ( #3058 ) ) ;
#16752 = ADVANCED_FACE ( 'NONE', ( #29308 ), #11250, .T. ) ;
#16753 = AXIS2_PLACEMENT_3D ( 'NONE', #29989, #30157, #14473 ) ;
#16754 = COLOUR_RGB ( '', 0.08235294, 0.09019608, 0.10196078) ;
#16755 = CARTESIAN_POINT ( 'NONE',  ( 55.50000000000000000, 155.0000000000000000, 14.49999999999999467 ) ) ;
#16756 = CARTESIAN_POINT ( 'NONE',  ( 63.28867513459482552, 170.7719333635740497, -7.904646289410545231E-15 ) ) ;
#16757 = CARTESIAN_POINT ( 'NONE',  ( -2.426778023690076225, 199.3768101843759553, 76.89886208192143613 ) ) ;
#16758 = CARTESIAN_POINT ( 'NONE',  ( 77.58867513459483689, 163.8167787843871110, 12.13525491562421621 ) ) ;
#16759 = CARTESIAN_POINT ( 'NONE',  ( 3.500000000000004885, 2.020725942163702715, -2.587392608830344720 ) ) ;
#16760 =( BOUNDED_CURVE ( )  B_SPLINE_CURVE ( 2, ( #20977, #13305, #23697, #1031, #30316, #19755, #8853, #22136, #1362, #4246, #32193 ),
 .UNSPECIFIED., .F., .T. ) 
 B_SPLINE_CURVE_WITH_KNOTS ( ( 3, 2, 2, 2, 2, 3 ),
 ( 0.1964285714285714524, 0.2000000000000000389, 0.2035714285714285976, 0.2071428571428572118, 0.2107142857142857706, 0.2142857142857143293 ),
 .UNSPECIFIED. ) 
 CURVE ( )  GEOMETRIC_REPRESENTATION_ITEM ( )  RATIONAL_B_SPLINE_CURVE ( ( 0.9999999999999996669, 0.9510565162951537532, 1.000000000000000000, 0.9510565162951534202, 1.000000000000000000, 0.9510565162951534202, 1.000000000000000000, 0.9510565162951534202, 1.000000000000000000, 0.9510565162951526430, 1.000000000000000666 ) ) 
 REPRESENTATION_ITEM ( '' )  );
#16761 = CARTESIAN_POINT ( 'NONE',  ( 58.82499999726881867, 141.7447067706911810, -9.630534252274385310 ) ) ;
#16763 = VERTEX_POINT ( 'NONE', #10757 ) ;
#16762 = CARTESIAN_POINT ( 'NONE',  ( 6.220909254589536808, 215.4770327129947987, 19.55113791807856671 ) ) ;
#16764 = DIRECTION ( 'NONE',  ( 0.000000000000000000, 0.9988620819214357738, 0.04769215134144196705 ) ) ;
#16765 = CARTESIAN_POINT ( 'NONE',  ( 82.07499999726880446, 168.2552932293087906, 9.630534252274372875 ) ) ;
#16766 = CARTESIAN_POINT ( 'NONE',  ( 3.753561863808689836, 218.3979405102790565, 91.40113791807857524 ) ) ;
#16767 = CARTESIAN_POINT ( 'NONE',  ( 10.00000000000000711, 206.9523078486586201, 95.00113791807856956 ) ) ;
#16768 = CARTESIAN_POINT ( 'NONE',  ( 54.30000000000001137, -88.00000000000000000, 20.00000000000000000 ) ) ;
#16769 = ORIENTED_EDGE ( 'NONE', *, *, #5363, .F. ) ;
#16770 = CARTESIAN_POINT ( 'NONE',  ( -0.05014649552828403384, 217.5146222423826714, 3.248862081921433997 ) ) ;
#16771 = CARTESIAN_POINT ( 'NONE',  ( -7.456977232089471386, 217.1783343296987709, 56.94886208192144039 ) ) ;
#16772 = CARTESIAN_POINT ( 'NONE',  ( 0.05014649552828275014, 196.4853777576173002, 79.74886208192143044 ) ) ;
#16773 = CARTESIAN_POINT ( 'NONE',  ( -7.456977232089471386, 217.1783343296987709, 2.948862081921434175 ) ) ;
#16774 = DIRECTION ( 'NONE',  ( 0.000000000000000000, 0.000000000000000000, -1.000000000000000000 ) ) ;
#16775 = CIRCLE ( 'NONE', #2103, 13.00000000000003908 ) ;
#16776 = CARTESIAN_POINT ( 'NONE',  ( 6.220909254589536808, 215.4770327129947702, 19.55113791807856671 ) ) ;
#16777 = CARTESIAN_POINT ( 'NONE',  ( -6.220909254589682469, 215.4770327129946850, 92.94886208192143329 ) ) ;
#16778 = ORIENTED_EDGE ( 'NONE', *, *, #6413, .F. ) ;
#16779 = CARTESIAN_POINT ( 'NONE',  ( 0.000000000000000000, 0.000000000000000000, -8.499999999999998224 ) ) ;
#16780 = ORIENTED_EDGE ( 'NONE', *, *, #5234, .F. ) ;
#16781 = CARTESIAN_POINT ( 'NONE',  ( 32.50000000000000000, 155.0000000000000000, -15.00000000000002487 ) ) ;
#16782 = CARTESIAN_POINT ( 'NONE',  ( 4.903702542908435547, 213.8346818373419751, 69.54886208192141339 ) ) ;
#16783 = VERTEX_POINT ( 'NONE', #26416 ) ;
#16784 = CARTESIAN_POINT ( 'NONE',  ( 83.12499999726881583, 155.0000000000000000, -15.58253175000000823 ) ) ;
#16785 = VERTEX_POINT ( 'NONE', #29140 ) ;
#16786 = CARTESIAN_POINT ( 'NONE',  ( 76.42499999726879878, 141.7447067706911810, 9.630534252274376428 ) ) ;
#16787 = CARTESIAN_POINT ( 'NONE',  ( 0.05014649552807626948, 215.4116977939061144, 67.25113791807856956 ) ) ;
#16788 = CARTESIAN_POINT ( 'NONE',  ( 75.78867513459483973, 155.0000000000000000, 15.00000000000001243 ) ) ;
#16789 = EDGE_CURVE ( 'NONE', #22659, #7757, #3077, .T. ) ;
#16790 = CARTESIAN_POINT ( 'NONE',  ( 37.10000000000000142, 168.7903194862797420, 4.480746418436729606 ) ) ;
#16791 = CARTESIAN_POINT ( 'NONE',  ( 0.05014649552828262524, 198.5883022060938572, 46.74886208192144466 ) ) ;
#16792 = AXIS2_PLACEMENT_3D ( 'NONE', #6026, #32264, #5862 ) ;
#16793 = CARTESIAN_POINT ( 'NONE',  ( -10.00000000000000711, 207.0476921513413515, 90.50113791807858377 ) ) ;
#16794 = CARTESIAN_POINT ( 'NONE',  ( 8.062137200540920645, 201.0835637161417822, 74.30113791807858092 ) ) ;
#16795 = EDGE_CURVE ( 'NONE', #8949, #536, #9930, .T. ) ;
#16796 = AXIS2_PLACEMENT_3D ( 'NONE', #9894, #14823, #1886 ) ;
#16797 = CARTESIAN_POINT ( 'NONE',  ( 92.50248874961125978, 155.0000000000000000, -13.00000000000001066 ) ) ;
#16798 = CYLINDRICAL_SURFACE ( 'NONE', #25485, 2.149999999999999023 ) ;
#16799 = DIRECTION ( 'NONE',  ( 0.9945218953682661844, 1.280104479606063378E-17, 0.1045284632677211112 ) ) ;
#16800 = CARTESIAN_POINT ( 'NONE',  ( 51.22499999726881725, 160.0630714827496206, -15.58253175000000823 ) ) ;
#16801 = CARTESIAN_POINT ( 'NONE',  ( -0.05014649552807705357, 194.3824533091408000, 50.75113791807857666 ) ) ;
#16802 = CARTESIAN_POINT ( 'NONE',  ( 1.734723475976807094E-14, 31.75426480542944319, -15.54379906938135214 ) ) ;
#16803 = CARTESIAN_POINT ( 'NONE',  ( 0.05014649552810505201, 217.5146222423826714, 94.25113791807855534 ) ) ;
#16804 = CARTESIAN_POINT ( 'NONE',  ( -9.984503880673475606, 210.2968891136704315, 66.65113791807857524 ) ) ;
#16805 = VECTOR ( 'NONE', #1395, 1000.000000000000000 ) ;
#16806 = CARTESIAN_POINT ( 'NONE',  ( -11.98450388067341876, 203.0532714938636047, 32.34886208192142476 ) ) ;
#16807 = CARTESIAN_POINT ( 'NONE',  ( 9.984503880673420539, 210.2968891136705736, 51.84886208192143897 ) ) ;
#16808 = CARTESIAN_POINT ( 'NONE',  ( 83.49999999453764588, 139.7537977485451393, -4.138211985947621020E-15 ) ) ;
#16809 =( BOUNDED_CURVE ( )  B_SPLINE_CURVE ( 2, ( #1765, #19999, #27824, #14886, #27162, #1269, #7399, #23231, #26126, #15228, #5171 ),
 .UNSPECIFIED., .F., .T. ) 
 B_SPLINE_CURVE_WITH_KNOTS ( ( 3, 2, 2, 2, 2, 3 ),
 ( 0.1607142857142856984, 0.1642857142857142572, 0.1678571428571428437, 0.1714285714285714302, 0.1750000000000000167, 0.1785714285714286031 ),
 .UNSPECIFIED. ) 
 CURVE ( )  GEOMETRIC_REPRESENTATION_ITEM ( )  RATIONAL_B_SPLINE_CURVE ( ( 1.000000000000000444, 0.9510565162951530871, 1.000000000000000000, 0.9510565162951534202, 1.000000000000000000, 0.9510565162951534202, 1.000000000000000000, 0.9510565162951534202, 1.000000000000000000, 0.9510565162951530871, 1.000000000000000444 ) ) 
 REPRESENTATION_ITEM ( '' )  );
#16810 = CARTESIAN_POINT ( 'NONE',  ( 0.05014649552807549926, 219.6175466908591716, 73.25113791807858377 ) ) ;
#16811 = CARTESIAN_POINT ( 'NONE',  ( 7.984503880673485376, 204.3529502787953902, 98.15113791807856103 ) ) ;
#16812 = ADVANCED_FACE ( 'NONE', ( #5959 ), #13800, .T. ) ;
#16813 = CARTESIAN_POINT ( 'NONE',  ( 6.139770520408223575, 215.5359834540460611, 63.54886208192144181 ) ) ;
#16814 = CARTESIAN_POINT ( 'NONE',  ( 5.000000000000000000, 4.685197434473814759, -5.637851296924623057E-15 ) ) ;
#16815 = EDGE_LOOP ( 'NONE', ( #4464, #16229 ) ) ;
#16816 = CARTESIAN_POINT ( 'NONE',  ( 7.375838497908012492, 217.2372850707501186, 63.54886208192144181 ) ) ;
#16817 = ORIENTED_EDGE ( 'NONE', *, *, #30138, .T. ) ;
#16818 = CARTESIAN_POINT ( 'NONE',  ( 72.07499999726880446, 168.2552932293087906, 9.630534252274372875 ) ) ;
#16819 = CARTESIAN_POINT ( 'NONE',  ( -0.05014649552828365914, 215.4116977939061144, 45.24886208192144466 ) ) ;
#16820 = CIRCLE ( 'NONE', #2151, 0.9999999999999941158 ) ;
#16821 = EDGE_CURVE ( 'NONE', #11212, #28445, #6123, .T. ) ;
#16822 = VERTEX_POINT ( 'NONE', #10007 ) ;
#16823 = CARTESIAN_POINT ( 'NONE',  ( 86.57499999726880446, 145.8408176439707802, 12.60653300113718345 ) ) ;
#16824 = FACE_BOUND ( 'NONE', #27168, .T. ) ;
#16825 = CARTESIAN_POINT ( 'NONE',  ( -9.000000000000005329, 207.1715159932409733, 103.3438395974723818 ) ) ;
#16826 = CARTESIAN_POINT ( 'NONE',  ( -0.05014649552807731031, 198.5883022060938572, 53.75113791807857666 ) ) ;
#16827 = CARTESIAN_POINT ( 'NONE',  ( 7.922281120364393914, -4.573931137438282057, -8.047472243342932430 ) ) ;
#16828 =( REPRESENTATION_RELATIONSHIP ('NONE','NONE', #25663, #16098 ) REPRESENTATION_RELATIONSHIP_WITH_TRANSFORMATION ( #28592 )SHAPE_REPRESENTATION_RELATIONSHIP( ) );
#16829 = CARTESIAN_POINT ( 'NONE',  ( 0.05014649552828275708, 196.4853777576173002, 31.74886208192143044 ) ) ;
#16830 = CARTESIAN_POINT ( 'NONE',  ( 69.37499999726881583, 155.0000000000000000, -15.58253175000000823 ) ) ;
#16831 = ORIENTED_EDGE ( 'NONE', *, *, #18646, .T. ) ;
#16832 = CARTESIAN_POINT ( 'NONE',  ( 77.50000000000000000, 155.0000000000000000, 7.500000000000007994 ) ) ;
#16833 = PLANE ( 'NONE',  #13940 ) ;
#16834 = CARTESIAN_POINT ( 'NONE',  ( -5.007715329123872641E-16, -8.660254037844399733, -7.422398894150038728 ) ) ;
#16835 = CARTESIAN_POINT ( 'NONE',  ( -8.015496119326597224, 209.5516654185217362, 14.64886208192143258 ) ) ;
#16836 = CARTESIAN_POINT ( 'NONE',  ( 0.05014649552810505201, 217.5146222423826714, 58.25113791807856245 ) ) ;
#16837 = CARTESIAN_POINT ( 'NONE',  ( -3.044812012440131443, 216.5253028482142952, 34.10113791807857808 ) ) ;
#16838 = DIRECTION ( 'NONE',  ( -1.000000000000000000, -0.000000000000000000, -0.000000000000000000 ) ) ;
#16839 = UNCERTAINTY_MEASURE_WITH_UNIT (LENGTH_MEASURE( 1.000000000000000082E-05 ), #15120, 'distance_accuracy_value', 'NONE');
#16840 = CARTESIAN_POINT ( 'NONE',  ( -8.000000000000008882, 207.0476921513413515, 0.5011379180785658916 ) ) ;
#16841 = CARTESIAN_POINT ( 'NONE',  ( 45.12499999726880873, 155.0000000000000000, -15.58253175000000823 ) ) ;
#16842 = CARTESIAN_POINT ( 'NONE',  ( -4.639619758716985842, 4.826867782832376719, -0.1499059597315285375 ) ) ;
#16843 = DIRECTION ( 'NONE',  ( -0.000000000000000000, -0.000000000000000000, 1.000000000000000000 ) ) ;
#16844 = CARTESIAN_POINT ( 'NONE',  ( 12.00000000000000711, 206.9523078486586485, 20.00113791807856956 ) ) ;
#16845 = VECTOR ( 'NONE', #21213, 1000.000000000000000 ) ;
#16846 = LINE ( 'NONE', #14967, #21120 ) ;
#16847 = EDGE_CURVE ( 'NONE', #12511, #18640, #8320, .T. ) ;
#16848 = CARTESIAN_POINT ( 'NONE',  ( 6.220909254589536808, 215.4770327129947702, 61.55113791807858092 ) ) ;
#16849 = CARTESIAN_POINT ( 'NONE',  ( 6.220909254589536808, 215.4770327129947987, 40.55113791807856671 ) ) ;
#16850 = CARTESIAN_POINT ( 'NONE',  ( 32.50000000000000000, 155.0000000000000000, -15.00000000000002487 ) ) ;
#16851 = FACE_OUTER_BOUND ( 'NONE', #28284, .T. ) ;
#16852 = CARTESIAN_POINT ( 'NONE',  ( 0.05014649552828288198, 194.3824533091408000, 1.748862081921433775 ) ) ;
#16853 = CARTESIAN_POINT ( 'NONE',  ( 9.984503880673420539, 210.2968891136705736, 6.848862081921434530 ) ) ;
#16854 = CARTESIAN_POINT ( 'NONE',  ( 69.79999999453761461, 146.4771138417591203, -11.73074641843674470 ) ) ;
#16855 = EDGE_LOOP ( 'NONE', ( #23199, #21987 ) ) ;
#16856 = CARTESIAN_POINT ( 'NONE',  ( -7.456977232089304408, 196.8216656703010301, 48.05113791807856671 ) ) ;
#16857 = CARTESIAN_POINT ( 'NONE',  ( -8.015496119326531499, 204.4483345814780364, 72.35113791807857808 ) ) ;
#16858 = EDGE_CURVE ( 'NONE', #20297, #6207, #13721, .T. ) ;
#16859 = CARTESIAN_POINT ( 'NONE',  ( -6.139770520408224463, 198.4640165459539389, 29.04886208192143471 ) ) ;
#16860 = DIRECTION ( 'NONE',  ( 1.000000000000000000, -0.000000000000000000, -0.000000000000000000 ) ) ;
#16861 = ORIENTED_EDGE ( 'NONE', *, *, #4127, .F. ) ;
#16862 = CARTESIAN_POINT ( 'NONE',  ( 10.01549611932653860, 210.2015048109876716, 85.85113791807857808 ) ) ;
#16863 = EDGE_CURVE ( 'NONE', #16267, #7668, #15271, .T. ) ;
#16864 = EDGE_LOOP ( 'NONE', ( #28444, #29506, #31890, #9287, #2255, #12684, #33603 ) ) ;
#16865 = CARTESIAN_POINT ( 'NONE',  ( 42.68867513459482410, 150.1262045565064227, -15.00000000000002665 ) ) ;
#16866 = LINE ( 'NONE', #18764, #29060 ) ;
#16867 = EDGE_LOOP ( 'NONE', ( #17031, #33400, #29649, #28398 ) ) ;
#16868 = CARTESIAN_POINT ( 'NONE',  ( 6.500168698208129925, 211.6636982574063381, 22.70113791807856529 ) ) ;
#16869 = CARTESIAN_POINT ( 'NONE',  ( -60.87189664283175006, 194.9921494935721569, 0.8066102793772919055 ) ) ;
#16870 = CARTESIAN_POINT ( 'NONE',  ( 8.118202686958138514, 201.1607312380088501, 1.298862081921434486 ) ) ;
#16871 = CARTESIAN_POINT ( 'NONE',  ( 52.67499999726880588, 141.7447067706911810, 9.630534252274376428 ) ) ;
#16872 = VERTEX_POINT ( 'NONE', #29646 ) ;
#16873 = CARTESIAN_POINT ( 'NONE',  ( 4.903702542908601636, 200.1653181626581102, 50.45113791807857240 ) ) ;
#16874 = FACE_OUTER_BOUND ( 'NONE', #15623, .T. ) ;
#16875 = CARTESIAN_POINT ( 'NONE',  ( -7.500000000000000000, -4.330127018922198090, -7.422398894150034288 ) ) ;
#16876 = CARTESIAN_POINT ( 'NONE',  ( -10.00000000000000711, 206.9523078486584495, 89.49886208192144466 ) ) ;
#16877 = CARTESIAN_POINT ( 'NONE',  ( 60.67499999726881299, 141.7447067706911810, 9.630534252274376428 ) ) ;
#16878 = CARTESIAN_POINT ( 'NONE',  ( -0.05014649552810635652, 196.4853777576173002, 32.75113791807856956 ) ) ;
#16879 = CARTESIAN_POINT ( 'NONE',  ( 7.500000000000000888, -2.886751345948134873, -7.198902722707428481 ) ) ;
#16880 = CARTESIAN_POINT ( 'NONE',  ( -12.01549611932659722, 210.8513442034533227, 83.64886208192143613 ) ) ;
#16881 = CARTESIAN_POINT ( 'NONE',  ( 83.30000000000001137, 163.5228861582408797, 11.73074641843673049 ) ) ;
#16882 = CARTESIAN_POINT ( 'NONE',  ( 62.51132485994280330, 163.8167787843871110, 12.13525491562421621 ) ) ;
#16883 = CARTESIAN_POINT ( 'NONE',  ( 64.50000000000000000, -103.0000000000000000, 20.00000000000000000 ) ) ;
#16884 = CARTESIAN_POINT ( 'NONE',  ( 8.062137200540920645, 201.0835637161417822, 95.30113791807858092 ) ) ;
#16885 = CARTESIAN_POINT ( 'NONE',  ( 27.50000000000000355, -13.28298644054430255, -16.25870334244831383 ) ) ;
#16886 = CARTESIAN_POINT ( 'NONE',  ( 45.57499999726881157, 164.1591823560292198, -12.60653300113719766 ) ) ;
#16887 = CARTESIAN_POINT ( 'NONE',  ( 8.118202686958039038, 212.8392687619912635, 37.70113791807857240 ) ) ;
#16888 = EDGE_CURVE ( 'NONE', #14731, #26926, #6293, .T. ) ;
#16889 = CARTESIAN_POINT ( 'NONE',  ( 85.12499999726881583, 155.0000000000000000, -15.58253175000000823 ) ) ;
#16890 = EDGE_LOOP ( 'NONE', ( #23285, #25109, #27933, #17383 ) ) ;
#16891 = FACE_OUTER_BOUND ( 'NONE', #11304, .T. ) ;
#16892 = CARTESIAN_POINT ( 'NONE',  ( 49.51132485994280330, 146.1832212156128890, -12.13525491562423042 ) ) ;
#16893 = CARTESIAN_POINT ( 'NONE',  ( 50.79999999453762882, 163.5228861582408797, 11.73074641843673049 ) ) ;
#16894 = CARTESIAN_POINT ( 'NONE',  ( -11.98450388067348804, 210.9467285061362247, 21.65113791807856813 ) ) ;
#16895 = EDGE_CURVE ( 'NONE', #28642, #11454, #6930, .T. ) ;
#16896 = CYLINDRICAL_SURFACE ( 'NONE', #16500, 15.00000000000001776 ) ;
#16897 = CARTESIAN_POINT ( 'NONE',  ( 66.41132485994285162, 167.7597621252805880, 9.270509831248428867 ) ) ;
#16898 = ORIENTED_EDGE ( 'NONE', *, *, #19928, .T. ) ;
#16899 = CARTESIAN_POINT ( 'NONE',  ( 3.662846001189864698, 218.4274158808046593, 39.39886208192143613 ) ) ;
#16900 = CARTESIAN_POINT ( 'NONE',  ( -10.01549611932653860, 203.7984951890123284, 3.351137918078566091 ) ) ;
#16901 = CARTESIAN_POINT ( 'NONE',  ( 8.118202686958039038, 212.8392687619912635, 52.70113791807857240 ) ) ;
#16902 = CARTESIAN_POINT ( 'NONE',  ( 4.903702542908435547, 213.8346818373419751, 15.54886208192143826 ) ) ;
#16903 = UNCERTAINTY_MEASURE_WITH_UNIT (LENGTH_MEASURE( 1.000000000000000082E-05 ), #8959, 'distance_accuracy_value', 'NONE');
#16904 = CARTESIAN_POINT ( 'NONE',  ( 78.98867513459482836, 163.8167787843871110, -12.13525491562423397 ) ) ;
#16905 = VECTOR ( 'NONE', #15670, 1000.000000000000000 ) ;
#16906 = ORIENTED_EDGE ( 'NONE', *, *, #9936, .T. ) ;
#16907 = CARTESIAN_POINT ( 'NONE',  ( -2.426778023690076225, 199.3768101843759553, 100.8988620819214361 ) ) ;
#16908 = CYLINDRICAL_SURFACE ( 'NONE', #14319, 5.250000000000004441 ) ;
#16909 = CARTESIAN_POINT ( 'NONE',  ( 4.903702542908601636, 200.1653181626581102, 44.45113791807857240 ) ) ;
#16910 = CARTESIAN_POINT ( 'NONE',  ( 33.57499999726881157, 164.1591823560292198, -12.60653300113719766 ) ) ;
#16911 = ORIENTED_EDGE ( 'NONE', *, *, #5748, .T. ) ;
#16912 = CARTESIAN_POINT ( 'NONE',  ( 36.52499999726881441, 140.1801316387863778, 4.815267126137185549 ) ) ;
#16913 = DIRECTION ( 'NONE',  ( 0.000000000000000000, 0.000000000000000000, -1.000000000000000000 ) ) ;
#16914 = CARTESIAN_POINT ( 'NONE',  ( -10.00000000000000711, 206.9523078486584495, 65.49886208192143044 ) ) ;
#16915 = CARTESIAN_POINT ( 'NONE',  ( 38.77499999726881441, 140.1801316387863778, 4.815267126137185549 ) ) ;
#16916 = FACE_OUTER_BOUND ( 'NONE', #931, .T. ) ;
#16917 = CARTESIAN_POINT ( 'NONE',  ( 6.220909254589536808, 215.4770327129947702, 4.551137918078564937 ) ) ;
#16918 = CARTESIAN_POINT ( 'NONE',  ( 63.90000000000001279, 141.2096805137202580, 4.480746418436733158 ) ) ;
#16919 = DIRECTION ( 'NONE',  ( 1.000000000000000000, 0.000000000000000000, 0.000000000000000000 ) ) ;
#16920 = CARTESIAN_POINT ( 'NONE',  ( 7.984503880673422316, 209.6470497212048372, 84.84886208192142476 ) ) ;
#16921 = CARTESIAN_POINT ( 'NONE',  ( 77.28867513459483973, 170.7719333635740497, -7.904646289410545231E-15 ) ) ;
#16922 = B_SPLINE_CURVE_WITH_KNOTS ( 'NONE', 3,
 ( #26355, #12745, #21073, #2523, #18689, #7640 ),
 .UNSPECIFIED., .F., .F.,
 ( 4, 2, 4 ),
 ( 0.004615310220740742597, 0.006918661718823353700, 0.009222013216905964803 ),
 .UNSPECIFIED. ) ;
#16923 = CARTESIAN_POINT ( 'NONE',  ( 3.500000000000004441, 1.362959798491822250, -2.760265505016209264 ) ) ;
#16924 = B_SPLINE_CURVE_WITH_KNOTS ( 'NONE', 3,
 ( #29800, #22458, #22295, #16842, #19573, #32850, #9513, #14628 ),
 .UNSPECIFIED., .F., .F.,
 ( 4, 2, 2, 4 ),
 ( 2.459764730722484167E-07, 0.001920659145285713056, 0.002880865729692032307, 0.003841072314098351557 ),
 .UNSPECIFIED. ) ;
#16925 = CARTESIAN_POINT ( 'NONE',  ( 59.32499999726881157, 164.1591823560292198, -12.60653300113719766 ) ) ;
#16927 = ORIENTED_EDGE ( 'NONE', *, *, #11754, .T. ) ;
#16926 = CARTESIAN_POINT ( 'NONE',  ( -8.118202686958039038, 201.1607312380087080, 24.20113791807856884 ) ) ;
#16928 = CARTESIAN_POINT ( 'NONE',  ( 125.5000000000000000, 80.04668119422552763, -74.95331880577366235 ) ) ;
#16929 = AXIS2_PLACEMENT_3D ( 'NONE', #23306, #7129, #25688 ) ;
#16930 = CARTESIAN_POINT ( 'NONE',  ( 84.27499999726879309, 160.0630714827496206, 15.58253174999999402 ) ) ;
#16931 = CARTESIAN_POINT ( 'NONE',  ( -7.456977232089304408, 196.8216656703010301, 87.05113791807856671 ) ) ;
#16932 = CARTESIAN_POINT ( 'NONE',  ( 72.78867513459482552, 155.0000000000000000, -15.00000000000002487 ) ) ;
#16933 = CARTESIAN_POINT ( 'NONE',  ( 53.18867513459482410, 169.2658477444273331, -4.635254915624224203 ) ) ;
#16934 = VERTEX_POINT ( 'NONE', #27085 ) ;
#16935 = CARTESIAN_POINT ( 'NONE',  ( -11.98450388067341876, 203.0532714938636047, 68.34886208192142476 ) ) ;
#16936 = CARTESIAN_POINT ( 'NONE',  ( -9.984503880673420539, 203.7031108863293980, 77.34886208192143897 ) ) ;
#16937 = CARTESIAN_POINT ( 'NONE',  ( -0.05014649552828442242, 219.6175466908591716, 15.24886208192143577 ) ) ;
#16938 = DIRECTION ( 'NONE',  ( 0.000000000000000000, 0.000000000000000000, -1.000000000000000000 ) ) ;
#16939 = CARTESIAN_POINT ( 'NONE',  ( 8.062137200540920645, 201.0835637161417822, 20.30113791807856671 ) ) ;
#16940 = CARTESIAN_POINT ( 'NONE',  ( 10.01549611932659545, 203.7984951890123853, 88.14886208192143613 ) ) ;
#16941 = ADVANCED_FACE ( 'NONE', ( #20212 ), #30268, .F. ) ;
#16942 = ORIENTED_EDGE ( 'NONE', *, *, #12294, .F. ) ;
#16943 = CARTESIAN_POINT ( 'NONE',  ( 38.81132485994282177, 150.1262045565064795, 15.00000000000006395 ) ) ;
#16944 = ORIENTED_EDGE ( 'NONE', *, *, #33019, .T. ) ;
#16945 = PLANE ( 'NONE',  #24337 ) ;
#16946 = CARTESIAN_POINT ( 'NONE',  ( 6.444103211790928043, 211.7408657792734061, 75.69886208192143329 ) ) ;
#16947 = VERTEX_POINT ( 'NONE', #21972 ) ;
#16948 = CARTESIAN_POINT ( 'NONE',  ( 84.32499999726880446, 145.8408176439707802, 12.60653300113718345 ) ) ;
#16949 = ORIENTED_EDGE ( 'NONE', *, *, #11483, .F. ) ;
#16950 = CARTESIAN_POINT ( 'NONE',  ( 68.81132485994281467, 150.1262045565065364, 15.00000000000011191 ) ) ;
#16951 = AXIS2_PLACEMENT_3D ( 'NONE', #9050, #21663, #31884 ) ;
#16952 = CARTESIAN_POINT ( 'NONE',  ( 74.12499999726881583, 155.0000000000000000, 15.58253174999999402 ) ) ;
#16953 = CARTESIAN_POINT ( 'NONE',  ( -52.50000000000002132, 155.0000000000000000, 40.00000000000001421 ) ) ;
#16954 =( BOUNDED_CURVE ( )  B_SPLINE_CURVE ( 2, ( #5944, #842, #5618, #24342, #5773, #16335, #3731, #26729, #11568, #14120, #8191 ),
 .UNSPECIFIED., .F., .T. ) 
 B_SPLINE_CURVE_WITH_KNOTS ( ( 3, 2, 2, 2, 2, 3 ),
 ( 0.9107142857142853654, 0.9142857142857139241, 0.9178571428571425939, 0.9214285714285711526, 0.9249999999999998224, 0.9285714285714283811 ),
 .UNSPECIFIED. ) 
 CURVE ( )  GEOMETRIC_REPRESENTATION_ITEM ( )  RATIONAL_B_SPLINE_CURVE ( ( 1.000000000000004663, 0.9510565162951488682, 1.000000000000000000, 0.9510565162951534202, 1.000000000000000000, 0.9510565162951534202, 1.000000000000000000, 0.9510565162951534202, 1.000000000000000000, 0.9510565162951549745, 0.9999999999999984457 ) ) 
 REPRESENTATION_ITEM ( '' )  );
#16955 = CARTESIAN_POINT ( 'NONE',  ( 7.984503880673485376, 204.3529502787953902, 65.15113791807856103 ) ) ;
#16956 = CARTESIAN_POINT ( 'NONE',  ( 87.50000000000001421, 166.8192717339189812, 9.236060614774261879 ) ) ;
#16958 = AXIS2_PLACEMENT_3D ( 'NONE', #14416, #17474, #3852 ) ;
#16957 = SURFACE_STYLE_FILL_AREA ( #12020 ) ;
#16959 = CARTESIAN_POINT ( 'NONE',  ( 43.10000000000000142, 168.7903194862797420, 4.480746418436729606 ) ) ;
#16960 = CARTESIAN_POINT ( 'NONE',  ( 2.517493886309087436, 199.4062855549015865, 49.59886208192143897 ) ) ;
#16961 = CARTESIAN_POINT ( 'NONE',  ( -8.062137200540920645, 212.9164362838581894, 75.80113791807858092 ) ) ;
#16962 = CARTESIAN_POINT ( 'NONE',  ( -6.500000000000000888, 0.000000000000000000, 0.000000000000000000 ) ) ;
#16963 = LINE ( 'NONE', #17138, #4279 ) ;
#16964 = LINE ( 'NONE', #9134, #20789 ) ;
#16965 = CARTESIAN_POINT ( 'NONE',  ( 48.52499999726880731, 140.1801316387863778, 4.815267126137185549 ) ) ;
#16966 = CARTESIAN_POINT ( 'NONE',  ( -12.00000000000000711, 207.0476921513413515, 57.50113791807856956 ) ) ;
#16967 = CARTESIAN_POINT ( 'NONE',  ( 4.174999999999999822, 0.000000000000000000, -0.5776712190230133270 ) ) ;
#16968 = CARTESIAN_POINT ( 'NONE',  ( 12.00000000000000711, 206.9523078486586485, 5.001137918078565114 ) ) ;
#16969 = CARTESIAN_POINT ( 'NONE',  ( -3.044812012440131443, 216.5253028482142952, 76.10113791807856387 ) ) ;
#16970 = CARTESIAN_POINT ( 'NONE',  ( 12.00000000000000711, 207.0476921513415220, 36.99886208192143044 ) ) ;
#16971 = CARTESIAN_POINT ( 'NONE',  ( 10.01549611932659367, 203.7984951890124421, 52.14886208192142902 ) ) ;
#16972 = CARTESIAN_POINT ( 'NONE',  ( 85.49999999453763166, 139.7537977485451393, -4.138211985947621020E-15 ) ) ;
#16973 = CARTESIAN_POINT ( 'NONE',  ( -9.680171189290831535, 214.0920067884431148, 84.80113791807858092 ) ) ;
#16974 = CARTESIAN_POINT ( 'NONE',  ( -2.517493886308901807, 199.4062855549015012, 95.90113791807857524 ) ) ;
#16975 = CARTESIAN_POINT ( 'NONE',  ( -10.01549611932659722, 210.2015048109875011, 59.64886208192143613 ) ) ;
#16976 = ADVANCED_FACE ( 'NONE', ( #30613 ), #17323, .F. ) ;
#16977 = EDGE_LOOP ( 'NONE', ( #5446, #9781, #14107 ) ) ;
#16978 = CARTESIAN_POINT ( 'NONE',  ( 9.736236675708031640, 199.9851607334238963, 58.29886208192143471 ) ) ;
#16979 = CIRCLE ( 'NONE', #25703, 12.10452846326762177 ) ;
#16980 = ORIENTED_EDGE ( 'NONE', *, *, #33450, .F. ) ;
#16981 = CARTESIAN_POINT ( 'NONE',  ( 70.27499999726880731, 160.0630714827496206, 15.58253174999999402 ) ) ;
#16982 = CARTESIAN_POINT ( 'NONE',  ( -0.05014649552828365914, 215.4116977939061144, 42.24886208192143755 ) ) ;
#16983 = EDGE_CURVE ( 'NONE', #15895, #18797, #14572, .T. ) ;
#16984 = VECTOR ( 'NONE', #20689, 1000.000000000000000 ) ;
#16985 = EDGE_LOOP ( 'NONE', ( #7701, #23243, #10933, #3866, #14150, #4167, #12219 ) ) ;
#16986 = CARTESIAN_POINT ( 'NONE',  ( 84.17499999726882720, 164.1591823560292198, 12.60653300113718167 ) ) ;
#16987 = DIRECTION ( 'NONE',  ( -0.2649168722799616349, 0.9642688156137669830, -0.002168413296787739895 ) ) ;
#16988 = EDGE_CURVE ( 'NONE', #21673, #13849, #1029, .T. ) ;
#16989 = CYLINDRICAL_SURFACE ( 'NONE', #28540, 5.250000000000004441 ) ;
#16990 = CARTESIAN_POINT ( 'NONE',  ( 8.000000000000008882, 206.9523078486586485, 59.00113791807857666 ) ) ;
#16991 = PRESENTATION_STYLE_ASSIGNMENT (( #27222 ) ) ;
#16992 = CARTESIAN_POINT ( 'NONE',  ( -6.220909254589682469, 215.4770327129946850, 44.94886208192143329 ) ) ;
#16993 = CARTESIAN_POINT ( 'NONE',  ( 70.17499999726881299, 164.1591823560292198, 12.60653300113718167 ) ) ;
#16994 = ORIENTED_EDGE ( 'NONE', *, *, #13877, .F. ) ;
#16995 = CARTESIAN_POINT ( 'NONE',  ( -52.50000000000002132, 155.0000000000000000, 17.00000000000001066 ) ) ;
#16996 = EDGE_CURVE ( 'NONE', #17245, #28697, #9811, .T. ) ;
#16997 =( LENGTH_UNIT ( ) NAMED_UNIT ( * ) SI_UNIT ( .MILLI., .METRE. ) );
#16998 = CARTESIAN_POINT ( 'NONE',  ( -52.50000000000002132, -95.00000000000000000, 20.00000000000001776 ) ) ;
#16999 = DIRECTION ( 'NONE',  ( 0.000000000000000000, 0.000000000000000000, -1.000000000000000000 ) ) ;
#17000 = CARTESIAN_POINT ( 'NONE',  ( 2.426778023690075337, 214.6231898156240447, 15.39886208192143613 ) ) ;
#17001 = CARTESIAN_POINT ( 'NONE',  ( -9.984503880673473830, 210.2968891136704315, 60.65113791807856103 ) ) ;
#17002 = CARTESIAN_POINT ( 'NONE',  ( -10.01549611932653860, 203.7984951890123284, 42.35113791807855677 ) ) ;
#17003 = CARTESIAN_POINT ( 'NONE',  ( 71.01132485994281751, 142.2402378747194405, 9.270509831248432420 ) ) ;
#17004 = ITEM_DEFINED_TRANSFORMATION ( 'NONE', 'NONE', #22422,  #2404 ) ;
#17005 = CARTESIAN_POINT ( 'NONE',  ( -3.135527875058821579, 197.5041725223112223, 14.90113791807856636 ) ) ;
#17006 = CARTESIAN_POINT ( 'NONE',  ( -8.015496119326531499, 204.4483345814780364, 0.3511379180785659249 ) ) ;
#17007 = AXIS2_PLACEMENT_3D ( 'NONE', #9271, #6549, #14889 ) ;
#17008 = CARTESIAN_POINT ( 'NONE',  ( 46.72499999726881015, 140.1801316387863778, -4.815267126137194431 ) ) ;
#17009 = FILL_AREA_STYLE_COLOUR ( '', #4599 ) ;
#17010 = CARTESIAN_POINT ( 'NONE',  ( 33.72499999726881725, 169.8198683612136222, 4.815267126137181997 ) ) ;
#17011 = CARTESIAN_POINT ( 'NONE',  ( -9.736236675707914401, 199.9851607334237542, 30.20113791807856529 ) ) ;
#17012 = DIRECTION ( 'NONE',  ( 1.000000000000000000, 0.000000000000000000, 0.000000000000000000 ) ) ;
#17013 = EDGE_CURVE ( 'NONE', #1328, #3092, #15673, .T. ) ;
#17014 = AXIS2_PLACEMENT_3D ( 'NONE', #2466, #28188, #12677 ) ;
#17015 = CARTESIAN_POINT ( 'NONE',  ( 6.139770520408368348, 198.4640165459539674, 77.45113791807854398 ) ) ;
#17016 = CARTESIAN_POINT ( 'NONE',  ( -6.139770520408368348, 215.5359834540460042, 36.95113791807857240 ) ) ;
#17017 = DIRECTION ( 'NONE',  ( 0.000000000000000000, -0.5000000000000008882, -0.8660254037844381525 ) ) ;
#17018 = PLANE ( 'NONE',  #8163 ) ;
#17019 = CARTESIAN_POINT ( 'NONE',  ( 9.736236675708031640, 199.9851607334238963, 1.298862081921434264 ) ) ;
#17020 = CARTESIAN_POINT ( 'NONE',  ( -10.00000000000000711, 206.9523078486584495, 14.49886208192143577 ) ) ;
#17021 = CARTESIAN_POINT ( 'NONE',  ( 65.39999999453763735, 141.2096805137202580, 4.480746418436733158 ) ) ;
#17022 = ORIENTED_EDGE ( 'NONE', *, *, #21749, .T. ) ;
#17023 = CARTESIAN_POINT ( 'NONE',  ( 12.01549611932652972, 210.8513442034534933, 49.85113791807857808 ) ) ;
#17024 = CARTESIAN_POINT ( 'NONE',  ( -4.903702542908602524, 213.8346818373418898, 69.95113791807858661 ) ) ;
#17025 = CARTESIAN_POINT ( 'NONE',  ( -8.062137200540822946, 201.0835637161416400, 35.19886208192143329 ) ) ;
#17026 = EDGE_CURVE ( 'NONE', #6222, #27878, #2502, .T. ) ;
#17027 = FILL_AREA_STYLE ('',( #27420 ) ) ;
#17028 = ORIENTED_EDGE ( 'NONE', *, *, #26031, .T. ) ;
#17029 = AXIS2_PLACEMENT_3D ( 'NONE', #25031, #1178, #30479 ) ;
#17030 = CARTESIAN_POINT ( 'NONE',  ( 3.135527875058820690, 216.4958274776887492, 94.40113791807857524 ) ) ;
#17031 = ORIENTED_EDGE ( 'NONE', *, *, #29, .F. ) ;
#17032 = CARTESIAN_POINT ( 'NONE',  ( 42.58867513459482979, 146.1832212156128890, -12.13525491562423042 ) ) ;
#17033 = ADVANCED_FACE ( 'NONE', ( #20721 ), #31120, .T. ) ;
#17034 = FACE_OUTER_BOUND ( 'NONE', #11097, .T. ) ;
#17035 = EDGE_LOOP ( 'NONE', ( #18287, #20316, #28351, #24232 ) ) ;
#17036 = CARTESIAN_POINT ( 'NONE',  ( -4.984841277089726574, 200.2242689037092305, 27.05113791807857027 ) ) ;
#17037 = AXIS2_PLACEMENT_3D ( 'NONE', #19968, #7031, #25080 ) ;
#17038 = LINE ( 'NONE', #7160, #21038 ) ;
#17039 = CARTESIAN_POINT ( 'NONE',  ( 10.01549611932659545, 203.7984951890123853, 10.14886208192143613 ) ) ;
#17040 = CARTESIAN_POINT ( 'NONE',  ( 48.57499999726881157, 145.8408176439707802, 12.60653300113718345 ) ) ;
#17041 = ORIENTED_EDGE ( 'NONE', *, *, #11411, .F. ) ;
#17042 = CARTESIAN_POINT ( 'NONE',  ( -2.426778023690262742, 214.6231898156240163, 46.10113791807857098 ) ) ;
#17043 = CARTESIAN_POINT ( 'NONE',  ( 67.11132485994281183, 140.7341522555726669, 4.635254915624211769 ) ) ;
#17044 = SURFACE_SIDE_STYLE ('',( #32377 ) ) ;
#17045 = DIRECTION ( 'NONE',  ( 1.000000000000000000, 0.000000000000000000, 0.000000000000000000 ) ) ;
#17046 = CARTESIAN_POINT ( 'NONE',  ( -10.00000000000000711, 206.9523078486584495, 92.49886208192144466 ) ) ;
#17047 = CARTESIAN_POINT ( 'NONE',  ( 57.47499999726879594, 160.0630714827496206, -15.58253175000000823 ) ) ;
#17048 = CARTESIAN_POINT ( 'NONE',  ( 6.139770520408368348, 198.4640165459539674, 32.45113791807856529 ) ) ;
#17049 = DIRECTION ( 'NONE',  ( 1.000000000000000000, 0.000000000000000000, 0.000000000000000000 ) ) ;
#17050 = ADVANCED_FACE ( 'NONE', ( #2832 ), #5216, .F. ) ;
#17051 = CARTESIAN_POINT ( 'NONE',  ( -3.135527875058821579, 197.5041725223112223, 17.90113791807856458 ) ) ;
#17052 = DIRECTION ( 'NONE',  ( 0.000000000000000000, -1.000000000000000000, 3.491481338843133355E-15 ) ) ;
#17053 = AXIS2_PLACEMENT_3D ( 'NONE', #2031, #2541, #23151 ) ;
#17054 = CARTESIAN_POINT ( 'NONE',  ( 79.30000000000001137, 163.5228861582408797, 11.73074641843673049 ) ) ;
#17055 = SURFACE_SIDE_STYLE ('',( #32720 ) ) ;
#17056 = DIRECTION ( 'NONE',  ( 0.000000000000000000, 0.000000000000000000, -1.000000000000000000 ) ) ;
#17057 = CARTESIAN_POINT ( 'NONE',  ( -10.01549611932653860, 203.7984951890123284, 90.35113791807857808 ) ) ;
#17058 = LINE ( 'NONE', #1557, #4236 ) ;
#17059 = CARTESIAN_POINT ( 'NONE',  ( 46.17499999726881299, 164.1591823560292198, 12.60653300113718167 ) ) ;
#17060 = EDGE_CURVE ( 'NONE', #31940, #11543, #6523, .T. ) ;
#17061 = CARTESIAN_POINT ( 'NONE',  ( 3.044812012440130555, 197.4746971517856764, 50.60113791807857808 ) ) ;
#17062 = CARTESIAN_POINT ( 'NONE',  ( 85.82499999726879025, 168.2552932293087906, 9.630534252274372875 ) ) ;
#17063 = CARTESIAN_POINT ( 'NONE',  ( -7.264118654998712010, 4.945491722146218905, -7.907633014911216840 ) ) ;
#17064 = CARTESIAN_POINT ( 'NONE',  ( 35.78867513459482552, 155.0000000000000000, 15.00000000000001243 ) ) ;
#17065 = VECTOR ( 'NONE', #7899, 1000.000000000000114 ) ;
#17066 = CARTESIAN_POINT ( 'NONE',  ( 44.59999999453762598, 168.7903194862797420, 4.480746418436729606 ) ) ;
#17067 = ORIENTED_EDGE ( 'NONE', *, *, #28713, .T. ) ;
#17068 = CARTESIAN_POINT ( 'NONE',  ( 11.98450388067348271, 203.0532714938637753, 23.15113791807856458 ) ) ;
#17069 = B_SPLINE_CURVE_WITH_KNOTS ( 'NONE', 3,
 ( #17202, #17714, #20099, #27586, #19598, #4256, #2048, #12436, #30322, #22827 ),
 .UNSPECIFIED., .F., .F.,
 ( 4, 2, 2, 2, 4 ),
 ( 8.662740229329108052E-20, 0.001989602278884365725, 0.003979204557768730582, 0.005968806836653095874, 0.007958409115537461165 ),
 .UNSPECIFIED. ) ;
#17070 = AXIS2_PLACEMENT_3D ( 'NONE', #24754, #26962, #16238 ) ;
#17071 = LINE ( 'NONE', #16727, #6169 ) ;
#17072 = AXIS2_PLACEMENT_3D ( 'NONE', #16519, #31856, #21300 ) ;
#17073 = DIRECTION ( 'NONE',  ( -1.000000000000000000, 0.000000000000000000, 0.000000000000000000 ) ) ;
#17074 = ORIENTED_EDGE ( 'NONE', *, *, #23752, .F. ) ;
#17075 = B_SPLINE_CURVE_WITH_KNOTS ( 'NONE', 3,
 ( #32943, #9096, #6373, #3989, #20166, #6719, #27494, #22558, #4149, #14546 ),
 .UNSPECIFIED., .F., .F.,
 ( 4, 2, 2, 2, 4 ),
 ( 0.01606529487141860474, 0.01806591702017404724, 0.02006653916892948974, 0.02406778346644037475, 0.03207027206146213782 ),
 .UNSPECIFIED. ) ;
#17076 = CARTESIAN_POINT ( 'NONE',  ( 7.375838497908012492, 217.2372850707501186, 39.54886208192143471 ) ) ;
#17077 = CARTESIAN_POINT ( 'NONE',  ( 10.01549611932653860, 210.2015048109876716, 4.851137918078563871 ) ) ;
#17078 = CARTESIAN_POINT ( 'NONE',  ( -6.139770520408369237, 215.5359834540460042, 63.95113791807857950 ) ) ;
#17079 = CARTESIAN_POINT ( 'NONE',  ( -4.903702542908436435, 200.1653181626580249, 26.04886208192144181 ) ) ;
#17080 = CIRCLE ( 'NONE', #11111, 13.00000000000001066 ) ;
#17081 = CARTESIAN_POINT ( 'NONE',  ( 125.5000000000000000, 261.0000000000000000, 0.000000000000000000 ) ) ;
#17082 = EDGE_LOOP ( 'NONE', ( #10013, #21303, #20095, #23909 ) ) ;
#17083 = CARTESIAN_POINT ( 'NONE',  ( -4.903702542908436435, 200.1653181626580249, 101.0488620819214276 ) ) ;
#17084 = EDGE_CURVE ( 'NONE', #854, #14265, #21218, .T. ) ;
#17085 = ADVANCED_FACE ( 'NONE', ( #8280 ), #23113, .T. ) ;
#17086 = CARTESIAN_POINT ( 'NONE',  ( 2.000000000000000000, 1.773042676681340968, -2.276824562219559311E-15 ) ) ;
#17087 = CARTESIAN_POINT ( 'NONE',  ( -7.984503880673488041, 209.6470497212046098, 42.65113791807857524 ) ) ;
#17088 = DIRECTION ( 'NONE',  ( 0.5526942671207023539, 0.1536855300543050473, 0.8190908404712123891 ) ) ;
#17089 = ORIENTED_EDGE ( 'NONE', *, *, #23274, .F. ) ;
#17090 = CARTESIAN_POINT ( 'NONE',  ( 38.72499999726881015, 140.1801316387863778, -4.815267126137194431 ) ) ;
#17091 = DIRECTION ( 'NONE',  ( 1.000000000000000000, 0.000000000000000000, 0.000000000000000000 ) ) ;
#17092 = CARTESIAN_POINT ( 'NONE',  ( 117.5000000000000142, 155.0000000000000000, -70.00000000000002842 ) ) ;
#17093 = AXIS2_PLACEMENT_3D ( 'NONE', #6835, #4275, #30178 ) ;
#17095 = EDGE_CURVE ( 'NONE', #30404, #18396, #24791, .T. ) ;
#17094 = CARTESIAN_POINT ( 'NONE',  ( -3.044812012439970683, 197.4746971517856196, 58.89886208192143613 ) ) ;
#17096 = VECTOR ( 'NONE', #22653, 1000.000000000000000 ) ;
#17097 = CARTESIAN_POINT ( 'NONE',  ( 37.57499999726881157, 164.1591823560292198, -12.60653300113719766 ) ) ;
#17098 = FACE_OUTER_BOUND ( 'NONE', #7147, .T. ) ;
#17099 = CARTESIAN_POINT ( 'NONE',  ( -8.062137200540920645, 212.9164362838581894, 6.801137918078565825 ) ) ;
#17100 = EDGE_CURVE ( 'NONE', #19626, #22313, #24632, .T. ) ;
#17101 = CARTESIAN_POINT ( 'NONE',  ( 60.59999999999999432, 159.7113355953771077, -14.50000000000000888 ) ) ;
#17102 = FACE_OUTER_BOUND ( 'NONE', #14056, .T. ) ;
#17103 = CARTESIAN_POINT ( 'NONE',  ( -4.984841277089891776, 213.7757310962905990, 80.94886208192143329 ) ) ;
#17104 = CARTESIAN_POINT ( 'NONE',  ( 98.19869130599479945, 155.0000000000000000, 0.000000000000000000 ) ) ;
#17105 = CARTESIAN_POINT ( 'NONE',  ( 58.50000000000001421, -88.00000000000000000, 20.00000000000000000 ) ) ;
#17106 = CARTESIAN_POINT ( 'NONE',  ( 66.92499999726881299, 145.8408176439707802, -12.60653300113719588 ) ) ;
#17107 = MECHANICAL_DESIGN_GEOMETRIC_PRESENTATION_REPRESENTATION (  '', ( #32320 ), #7321 ) ;
#17109 = VERTEX_POINT ( 'NONE', #18828 ) ;
#17108 = CARTESIAN_POINT ( 'NONE',  ( -3.135527875058821579, 197.5041725223112223, 17.90113791807856458 ) ) ;
#17110 = CARTESIAN_POINT ( 'NONE',  ( 103.4083388212532810, 155.0000000000000000, -32.00000000000002842 ) ) ;
#17111 = CARTESIAN_POINT ( 'NONE',  ( 80.17499999726881299, 164.1591823560292198, 12.60653300113718167 ) ) ;
#17112 = CARTESIAN_POINT ( 'NONE',  ( -9.736236675707914401, 199.9851607334237542, 90.20113791807857240 ) ) ;
#17113 = LINE ( 'NONE', #27497, #3413 ) ;
#17114 = ORIENTED_EDGE ( 'NONE', *, *, #29470, .T. ) ;
#17115 = CARTESIAN_POINT ( 'NONE',  ( 3.662846001189864698, 218.4274158808046593, 69.39886208192143613 ) ) ;
#17116 = CARTESIAN_POINT ( 'NONE',  ( 8.118202686958138514, 201.1607312380088501, 76.29886208192144181 ) ) ;
#17117 = AXIS2_PLACEMENT_3D ( 'NONE', #26039, #12754, #15802 ) ;
#17118 = CARTESIAN_POINT ( 'NONE',  ( -12.00000000000000711, 206.9523078486584780, 17.49886208192143400 ) ) ;
#17119 = FACE_OUTER_BOUND ( 'NONE', #23530, .T. ) ;
#17120 = CARTESIAN_POINT ( 'NONE',  ( 10.01549611932653860, 210.2015048109876716, 28.85113791807855677 ) ) ;
#17121 = DIRECTION ( 'NONE',  ( -0.2649168722799636333, 0.9642688156137663169, -0.002168413296789690158 ) ) ;
#17122 = CARTESIAN_POINT ( 'NONE',  ( 3.044812012439969795, 216.5253028482143520, 90.39886208192143613 ) ) ;
#17123 = CARTESIAN_POINT ( 'NONE',  ( 0.5219667817988800085, -7.204195837485521281, -0.5602453477493418710 ) ) ;
#17124 = ORIENTED_EDGE ( 'NONE', *, *, #15407, .T. ) ;
#17125 = DIRECTION ( 'NONE',  ( 0.000000000000000000, 0.000000000000000000, -1.000000000000000000 ) ) ;
#17126 = CARTESIAN_POINT ( 'NONE',  ( -8.015496119326597224, 209.5516654185217362, 71.64886208192143613 ) ) ;
#17127 = ORIENTED_EDGE ( 'NONE', *, *, #29739, .F. ) ;
#17128 = CARTESIAN_POINT ( 'NONE',  ( 87.22499999726881015, 160.0630714827496206, -15.58253175000000823 ) ) ;
#17129 = EDGE_LOOP ( 'NONE', ( #22024, #17460, #4760, #10397 ) ) ;
#17130 = CARTESIAN_POINT ( 'NONE',  ( 69.21132485994282035, 139.2280666364260071, -4.041636747397287284E-15 ) ) ;
#17131 = CARTESIAN_POINT ( 'NONE',  ( 77.12499999726881583, 155.0000000000000000, -15.58253175000000823 ) ) ;
#17132 = CARTESIAN_POINT ( 'NONE',  ( 32.50000000000000000, 155.0000000000000000, -6.938893903907228378E-15 ) ) ;
#17133 = CARTESIAN_POINT ( 'NONE',  ( 7.984503880673485376, 204.3529502787953902, 74.15113791807857524 ) ) ;
#17134 = CARTESIAN_POINT ( 'NONE',  ( 87.50000000000002842, 170.3690997408855878, -1.377696575527767697 ) ) ;
#17135 = CARTESIAN_POINT ( 'NONE',  ( 43.00000000000000711, 170.2462022514548323, -7.872454543227099337E-15 ) ) ;
#17136 = CARTESIAN_POINT ( 'NONE',  ( -8.015496119326597224, 209.5516654185217362, 50.64886208192145034 ) ) ;
#17137 = DIRECTION ( 'NONE',  ( -1.000000000000000000, -0.000000000000000000, -0.000000000000000000 ) ) ;
#17138 = CARTESIAN_POINT ( 'NONE',  ( 32.50000000000000000, 155.0000000000000000, 15.00000000000001243 ) ) ;
#17139 = LINE ( 'NONE', #20033, #13693 ) ;
#17140 = CARTESIAN_POINT ( 'NONE',  ( 48.42499999726881299, 141.7447067706911810, 9.630534252274376428 ) ) ;
#17141 = CARTESIAN_POINT ( 'NONE',  ( 66.07499999726881867, 168.2552932293087906, 9.630534252274372875 ) ) ;
#17142 = CARTESIAN_POINT ( 'NONE',  ( -11.98450388067348804, 210.9467285061362247, 60.65113791807856813 ) ) ;
#17143 = DIRECTION ( 'NONE',  ( -0.000000000000000000, -0.000000000000000000, 1.000000000000000000 ) ) ;
#17144 = CARTESIAN_POINT ( 'NONE',  ( -12.00000000000000711, 207.0476921513413515, 0.5011379180785653364 ) ) ;
#17145 = CARTESIAN_POINT ( 'NONE',  ( 9.984503880673473830, 203.7031108863295401, 74.15113791807856103 ) ) ;
#17146 = CARTESIAN_POINT ( 'NONE',  ( -11.98450388067341876, 203.0532714938636047, 38.34886208192142476 ) ) ;
#17147 = CARTESIAN_POINT ( 'NONE',  ( 6.220909254589680693, 198.5229672870052582, 43.44886208192143329 ) ) ;
#17148 = CARTESIAN_POINT ( 'NONE',  ( 84.19999999453763451, 163.5228861582408797, -11.73074641843674470 ) ) ;
#17149 = CARTESIAN_POINT ( 'NONE',  ( 0.05014649552807549926, 219.6175466908591716, 91.25113791807856956 ) ) ;
#17150 = CARTESIAN_POINT ( 'NONE',  ( -2.517493886308901807, 199.4062855549015012, 98.90113791807858945 ) ) ;
#17151 = CARTESIAN_POINT ( 'NONE',  ( -8.062137200540822946, 201.0835637161416400, 59.19886208192144039 ) ) ;
#17152 = SURFACE_SIDE_STYLE ('',( #1322 ) ) ;
#17153 = VERTEX_POINT ( 'NONE', #19503 ) ;
#17154 = CARTESIAN_POINT ( 'NONE',  ( 12.01549611932659367, 203.1486557965466773, 67.14886208192143613 ) ) ;
#17155 = VERTEX_POINT ( 'NONE', #24618 ) ;
#17156 = CARTESIAN_POINT ( 'NONE',  ( 71.37499999726881583, 155.0000000000000000, -15.58253175000000823 ) ) ;
#17157 = CARTESIAN_POINT ( 'NONE',  ( -8.015496119326597224, 209.5516654185217362, 44.64886208192143613 ) ) ;
#17158 = B_SPLINE_CURVE_WITH_KNOTS ( 'NONE', 3,
 ( #30803, #25684, #23466, #12399, #10196, #10533, #23301, #20913, #25514, #28068 ),
 .UNSPECIFIED., .F., .F.,
 ( 4, 2, 2, 2, 4 ),
 ( 0.01606529487141864984, 0.01806591702017408541, 0.02006653916892952097, 0.02406778346644038516, 0.03207027206146210313 ),
 .UNSPECIFIED. ) ;
#17159 = ORIENTED_EDGE ( 'NONE', *, *, #26065, .F. ) ;
#17160 = CARTESIAN_POINT ( 'NONE',  ( 85.57499999726880446, 164.1591823560292198, -12.60653300113719766 ) ) ;
#17161 = CARTESIAN_POINT ( 'NONE',  ( -2.927447417349532177, 2.351289329882143786, -2.778243469714890779 ) ) ;
#17162 = DIRECTION ( 'NONE',  ( 0.000000000000000000, 0.000000000000000000, -1.000000000000000000 ) ) ;
#17163 = CARTESIAN_POINT ( 'NONE',  ( -2.517493886308901807, 199.4062855549015012, 56.90113791807858235 ) ) ;
#17164 = LINE ( 'NONE', #17339, #29236 ) ;
#17165 = CARTESIAN_POINT ( 'NONE',  ( 6.139770520408223575, 215.5359834540460611, 42.54886208192142050 ) ) ;
#17166 = ORIENTED_EDGE ( 'NONE', *, *, #5983, .F. ) ;
#17167 = CYLINDRICAL_SURFACE ( 'NONE', #19990, 31.00000000000000000 ) ;
#17168 = SURFACE_STYLE_FILL_AREA ( #30122 ) ;
#17169 = CARTESIAN_POINT ( 'NONE',  ( 1.098735407079012738, -7.248058225758961193, -6.326622577870306685 ) ) ;
#17170 = CARTESIAN_POINT ( 'NONE',  ( 86.51132485994281751, 163.8167787843871110, 12.13525491562421621 ) ) ;
#17171 = CARTESIAN_POINT ( 'NONE',  ( 8.015496119326595448, 204.4483345814782638, 22.14886208192143613 ) ) ;
#17172 = CARTESIAN_POINT ( 'NONE',  ( 9.984503880673470277, 203.7031108863295401, 65.15113791807856103 ) ) ;
#17173 = ADVANCED_FACE ( 'NONE', ( #11170 ), #21381, .T. ) ;
#17174 = CARTESIAN_POINT ( 'NONE',  ( -3.044812012440131443, 216.5253028482142952, 49.10113791807857808 ) ) ;
#17175 = CARTESIAN_POINT ( 'NONE',  ( 71.11132485994281183, 140.7341522555726669, 4.635254915624211769 ) ) ;
#17176 = CONTEXT_DEPENDENT_SHAPE_REPRESENTATION ( #27930, #24509 ) ;
#17177 = CARTESIAN_POINT ( 'NONE',  ( -6.139770520408369237, 215.5359834540460042, 15.95113791807856884 ) ) ;
#17178 = CARTESIAN_POINT ( 'NONE',  ( -4.903702542908602524, 213.8346818373418898, 3.951137918078566624 ) ) ;
#17179 = CARTESIAN_POINT ( 'NONE',  ( 47.12499999726880873, 155.0000000000000000, -15.58253175000000823 ) ) ;
#17180 = CARTESIAN_POINT ( 'NONE',  ( -58.50000000000002132, 209.9999999999999716, 2.500000000000000000 ) ) ;
#17181 = DIRECTION ( 'NONE',  ( 0.000000000000000000, 0.000000000000000000, -1.000000000000000000 ) ) ;
#17182 = CARTESIAN_POINT ( 'NONE',  ( -12.00000000000000711, 207.0476921513413515, 24.50113791807856600 ) ) ;
#17183 = CARTESIAN_POINT ( 'NONE',  ( 0.000000000000000000, 4.685197434473814759, -5.637851296924623057E-15 ) ) ;
#17184 = CARTESIAN_POINT ( 'NONE',  ( -9.984503880673473830, 210.2968891136704315, 72.65113791807857524 ) ) ;
#17185 = CARTESIAN_POINT ( 'NONE',  ( 3.044812012440130555, 197.4746971517856764, 53.60113791807857098 ) ) ;
#17186 = DIRECTION ( 'NONE',  ( 0.9945218953682661844, 0.000000000000000000, -0.1045284632677211112 ) ) ;
#17187 = DIRECTION ( 'NONE',  ( 0.000000000000000000, 0.000000000000000000, 1.000000000000000000 ) ) ;
#17188 = CARTESIAN_POINT ( 'NONE',  ( 7.375838497908012492, 217.2372850707501186, 15.54886208192143826 ) ) ;
#17189 = CARTESIAN_POINT ( 'NONE',  ( 0.05014649552828275014, 196.4853777576173002, 16.74886208192143400 ) ) ;
#17190 = CARTESIAN_POINT ( 'NONE',  ( 66.79999999453762882, 163.5228861582408797, 11.73074641843673049 ) ) ;
#17191 = ORIENTED_EDGE ( 'NONE', *, *, #11801, .F. ) ;
#17192 = CARTESIAN_POINT ( 'NONE',  ( 0.05014649552807549926, 219.6175466908591716, 61.25113791807856245 ) ) ;
#17193 = CARTESIAN_POINT ( 'NONE',  ( -4.903702542908602524, 213.8346818373418898, 66.95113791807857240 ) ) ;
#17194 = CARTESIAN_POINT ( 'NONE',  ( -6.220909254589682469, 215.4770327129946850, 35.94886208192141908 ) ) ;
#17195 = VECTOR ( 'NONE', #1987, 1000.000000000000114 ) ;
#17196 = CARTESIAN_POINT ( 'NONE',  ( 3.250000000000003109, -5.629165124598849879, 0.000000000000000000 ) ) ;
#17197 = ORIENTED_EDGE ( 'NONE', *, *, #4602, .T. ) ;
#17198 = SHAPE_REPRESENTATION ( 'hex flange nut gradea_iso_ISO - 4161 - M8 - N', ( #2404 ), #27385 ) ;
#17199 = CARTESIAN_POINT ( 'NONE',  ( 10.00000000000000711, 206.9523078486586201, 89.00113791807858377 ) ) ;
#17200 = VERTEX_POINT ( 'NONE', #21882 ) ;
#17201 = CARTESIAN_POINT ( 'NONE',  ( 87.49999999999998579, 165.2808968839347301, -11.75397288630872694 ) ) ;
#17202 = CARTESIAN_POINT ( 'NONE',  ( -1.269541193505925744E-15, 7.895640089090863789, -6.564402953523717166 ) ) ;
#17203 = ORIENTED_EDGE ( 'NONE', *, *, #28137, .F. ) ;
#17204 = CARTESIAN_POINT ( 'NONE',  ( 4.903702542908601636, 200.1653181626581102, 35.45113791807857240 ) ) ;
#17205 = DIRECTION ( 'NONE',  ( -0.000000000000000000, -0.000000000000000000, 1.000000000000000000 ) ) ;
#17206 = CARTESIAN_POINT ( 'NONE',  ( 3.044812012439969795, 216.5253028482143520, 9.398862081921436129 ) ) ;
#17207 = CARTESIAN_POINT ( 'NONE',  ( 57.47499999726879594, 160.0630714827496206, -15.58253175000000823 ) ) ;
#17208 = VERTEX_POINT ( 'NONE', #8943 ) ;
#17209 = CARTESIAN_POINT ( 'NONE',  ( -4.984841277089726574, 200.2242689037092305, 54.05113791807856671 ) ) ;
#17210 = CARTESIAN_POINT ( 'NONE',  ( 3.500000000000004885, 2.020725942163676070, -2.899999999999999911 ) ) ;
#17211 = DIRECTION ( 'NONE',  ( 1.000000000000000000, -0.000000000000000000, -0.000000000000000000 ) ) ;
#17212 = CARTESIAN_POINT ( 'NONE',  ( 3.044812012439969795, 216.5253028482143520, 99.39886208192145034 ) ) ;
#17213 = CARTESIAN_POINT ( 'NONE',  ( 58.37499999726881583, 155.0000000000000000, 15.58253174999999402 ) ) ;
#17214 = CARTESIAN_POINT ( 'NONE',  ( -6.139770520408369237, 215.5359834540460042, 33.95113791807855108 ) ) ;
#17215 = FILL_AREA_STYLE_COLOUR ( '', #4568 ) ;
#17216 = EDGE_CURVE ( 'NONE', #23772, #10719, #21719, .T. ) ;
#17217 = CARTESIAN_POINT ( 'NONE',  ( -3.044812012440131443, 216.5253028482142952, 16.10113791807856742 ) ) ;
#17218 = AXIS2_PLACEMENT_3D ( 'NONE', #4973, #2084, #12470 ) ;
#17219 = CARTESIAN_POINT ( 'NONE',  ( 60.00000000000000000, 7.347880794884118356E-15, 45.00000000000000711 ) ) ;
#17220 = CARTESIAN_POINT ( 'NONE',  ( 80.00000000000001421, 139.7537977485451393, -4.138211985947621020E-15 ) ) ;
#17221 = CARTESIAN_POINT ( 'NONE',  ( -57.69437687863553776, 194.9296432668266732, -2.372230612754127499 ) ) ;
#17222 = PLANE ( 'NONE',  #7739 ) ;
#17223 = CARTESIAN_POINT ( 'NONE',  ( 3.662846001190051659, 195.5725841191953691, 2.601137918078566091 ) ) ;
#17224 = DIRECTION ( 'NONE',  ( 1.000000000000000000, 0.000000000000000000, 0.000000000000000000 ) ) ;
#17225 = CARTESIAN_POINT ( 'NONE',  ( 45.77499999726881441, 169.8198683612136222, -4.815267126137197984 ) ) ;
#17226 = CARTESIAN_POINT ( 'NONE',  ( 3.135527875058820690, 216.4958274776887492, 46.40113791807857524 ) ) ;
#17227 = AXIS2_PLACEMENT_3D ( 'NONE', #8143, #16118, #18195 ) ;
#17228 = CARTESIAN_POINT ( 'NONE',  ( 83.42499999726882720, 168.2552932293087906, -9.630534252274385310 ) ) ;
#17229 = EDGE_CURVE ( 'NONE', #28697, #10467, #11001, .T. ) ;
#17230 = PLANE ( 'NONE',  #28804 ) ;
#17231 = DIRECTION ( 'NONE',  ( -1.000000000000000000, -0.000000000000000000, -0.000000000000000000 ) ) ;
#17232 = CARTESIAN_POINT ( 'NONE',  ( 49.89999999453762314, 150.2886644046228639, -14.50000000000000888 ) ) ;
#17233 = ORIENTED_EDGE ( 'NONE', *, *, #25637, .F. ) ;
#17234 = CARTESIAN_POINT ( 'NONE',  ( 9.736236675707914401, 214.0148392665762458, 31.70113791807856529 ) ) ;
#17235 = CARTESIAN_POINT ( 'NONE',  ( 103.4083388212532810, 155.0000000000000000, 32.00000000000002842 ) ) ;
#17236 = CARTESIAN_POINT ( 'NONE',  ( 0.000000000000000000, 0.000000000000000000, -25.03750572909317285 ) ) ;
#17237 = VERTEX_POINT ( 'NONE', #29724 ) ;
#17238 = CARTESIAN_POINT ( 'NONE',  ( -7.456977232089471386, 217.1783343296987709, 44.94886208192144039 ) ) ;
#17239 = CARTESIAN_POINT ( 'NONE',  ( 8.118202686958039038, 212.8392687619912635, 4.701137918078565292 ) ) ;
#17240 = CARTESIAN_POINT ( 'NONE',  ( -6.220909254589537696, 198.5229672870051161, 57.05113791807857382 ) ) ;
#17241 = ADVANCED_FACE ( 'NONE', ( #8772 ), #21546, .F. ) ;
#17242 = CARTESIAN_POINT ( 'NONE',  ( 2.426778023690075337, 214.6231898156240447, 27.39886208192143613 ) ) ;
#17243 = AXIS2_PLACEMENT_3D ( 'NONE', #25709, #28441, #10225 ) ;
#17244 = DIRECTION ( 'NONE',  ( 0.000000000000000000, 0.000000000000000000, -1.000000000000000000 ) ) ;
#17245 = VERTEX_POINT ( 'NONE', #19162 ) ;
#17246 = CARTESIAN_POINT ( 'NONE',  ( -0.05014649552807731031, 198.5883022060938572, -0.2488620819214341084 ) ) ;
#17247 = ADVANCED_FACE ( 'NONE', ( #27173 ), #11673, .T. ) ;
#17248 = CARTESIAN_POINT ( 'NONE',  ( -1.994931997373328159E-14, -8.660254037844390851, -1.000000000000000888 ) ) ;
#17249 = CARTESIAN_POINT ( 'NONE',  ( 3.662846001189864698, 218.4274158808046593, 87.39886208192143613 ) ) ;
#17250 = CARTESIAN_POINT ( 'NONE',  ( 35.27499999726881441, 149.9369285172503510, -15.58253175000000823 ) ) ;
#17252 = ORIENTED_EDGE ( 'NONE', *, *, #13514, .F. ) ;
#17251 = VECTOR ( 'NONE', #20022, 1000.000000000000000 ) ;
#17253 = CARTESIAN_POINT ( 'NONE',  ( 45.82499999726881157, 168.2552932293087906, 9.630534252274372875 ) ) ;
#17254 = DIRECTION ( 'NONE',  ( 1.000000000000000000, 0.000000000000000000, 0.000000000000000000 ) ) ;
#17255 = DIRECTION ( 'NONE',  ( -1.000000000000000000, -0.000000000000000000, -0.000000000000000000 ) ) ;
#17256 = CARTESIAN_POINT ( 'NONE',  ( -10.00000000000000711, 206.9523078486584495, 59.49886208192143755 ) ) ;
#17257 = CARTESIAN_POINT ( 'NONE',  ( 38.87499999726880873, 138.6155565068815463, -3.929120461958505118E-15 ) ) ;
#17258 = DIRECTION ( 'NONE',  ( -0.1045284632676463932, 0.000000000000000000, 0.9945218953682741780 ) ) ;
#17259 = CARTESIAN_POINT ( 'NONE',  ( 9.984503880673470277, 203.7031108863295401, 2.151137918078565914 ) ) ;
#17260 = CARTESIAN_POINT ( 'NONE',  ( 94.70964751525852421, 155.0000000000000000, 0.000000000000000000 ) ) ;
#17261 = CARTESIAN_POINT ( 'NONE',  ( 61.40000000000000568, 159.7113355953771077, 14.49999999999999289 ) ) ;
#17262 = CARTESIAN_POINT ( 'NONE',  ( -1.750000000000016209, -3.031088913245524985, 0.000000000000000000 ) ) ;
#17263 = CARTESIAN_POINT ( 'NONE',  ( -7.984503880673422316, 204.3529502787951628, 86.34886208192143897 ) ) ;
#17264 = CIRCLE ( 'NONE', #31919, 50.00000000000000000 ) ;
#17265 = CARTESIAN_POINT ( 'NONE',  ( 77.50000000000000000, 155.0000000000000000, 13.50000000000000355 ) ) ;
#17266 = DIRECTION ( 'NONE',  ( -0.000000000000000000, -0.000000000000000000, -1.000000000000000000 ) ) ;
#17267 = CARTESIAN_POINT ( 'NONE',  ( 12.01549611932659367, 203.1486557965466773, 85.14886208192143613 ) ) ;
#17268 = CARTESIAN_POINT ( 'NONE',  ( 65.32499999726881867, 164.1591823560292198, -12.60653300113719766 ) ) ;
#17270 = VERTEX_POINT ( 'NONE', #19333 ) ;
#17269 = CARTESIAN_POINT ( 'NONE',  ( -10.01549611932653860, 203.7984951890123000, 21.35113791807856387 ) ) ;
#17271 = AXIS2_PLACEMENT_3D ( 'NONE', #24602, #30392, #11658 ) ;
#17272 = CARTESIAN_POINT ( 'NONE',  ( 60.63708498984762940, 155.0000000000000000, 6.938893903907228378E-15 ) ) ;
#17273 = CARTESIAN_POINT ( 'NONE',  ( 82.17499999726882720, 164.1591823560292198, 12.60653300113718167 ) ) ;
#17274 = CARTESIAN_POINT ( 'NONE',  ( -7.456977232089304408, 196.8216656703010301, 84.05113791807858092 ) ) ;
#17275 = EDGE_CURVE ( 'NONE', #8245, #11257, #31936, .T. ) ;
#17276 = EDGE_CURVE ( 'NONE', #6511, #18293, #22984, .T. ) ;
#17277 = CARTESIAN_POINT ( 'NONE',  ( -10.00000000000019362, 205.9534653805592654, 104.4507591396482127 ) ) ;
#17278 = AXIS2_PLACEMENT_3D ( 'NONE', #29343, #18782, #26770 ) ;
#17279 = EDGE_LOOP ( 'NONE', ( #9965, #32961 ) ) ;
#17280 = CARTESIAN_POINT ( 'NONE',  ( 7.375838497908012492, 217.2372850707501186, 66.54886208192144181 ) ) ;
#17281 = CARTESIAN_POINT ( 'NONE',  ( 0.05014649552828275014, 196.4853777576173002, 73.74886208192144466 ) ) ;
#17282 = CARTESIAN_POINT ( 'NONE',  ( 7.456977232089471386, 196.8216656703012006, 16.44886208192143684 ) ) ;
#17283 = CARTESIAN_POINT ( 'NONE',  ( 111.1125082318798007, 155.0000000000000000, 0.000000000000000000 ) ) ;
#17284 = CARTESIAN_POINT ( 'NONE',  ( 10.01549611932653860, 210.2015048109876716, 34.85113791807856387 ) ) ;
#17285 = ORIENTED_EDGE ( 'NONE', *, *, #22941, .T. ) ;
#17286 = PRODUCT_DEFINITION ( 'UNKNOWN', '', #26254, #18513 ) ;
#17287 = ADVANCED_FACE ( 'NONE', ( #19003 ), #29393, .F. ) ;
#17288 = CARTESIAN_POINT ( 'NONE',  ( -10.01549611932659722, 210.2015048109875011, 101.6488620819214361 ) ) ;
#17289 = CARTESIAN_POINT ( 'NONE',  ( 115.4999999999999858, 155.0000000000000000, -6.938893903907228378E-15 ) ) ;
#17290 = VERTEX_POINT ( 'NONE', #26828 ) ;
#17291 = CARTESIAN_POINT ( 'NONE',  ( -1.474514954580286030E-14, 206.9977241638431167, -6.000000000000014211 ) ) ;
#17292 = CARTESIAN_POINT ( 'NONE',  ( 8.015496119326595448, 204.4483345814782638, 82.14886208192143613 ) ) ;
#17293 = VECTOR ( 'NONE', #16156, 1000.000000000000000 ) ;
#17294 = EDGE_CURVE ( 'NONE', #5005, #21724, #3492, .T. ) ;
#17295 = ORIENTED_EDGE ( 'NONE', *, *, #7924, .T. ) ;
#17296 = AXIS2_PLACEMENT_3D ( 'NONE', #21725, #22232, #17125 ) ;
#17297 = CARTESIAN_POINT ( 'NONE',  ( 83.92499999726882720, 164.1591823560292198, 12.60653300113718167 ) ) ;
#17299 = VERTEX_POINT ( 'NONE', #29559 ) ;
#17298 = B_SPLINE_CURVE_WITH_KNOTS ( 'NONE', 3,
 ( #4531, #1976, #28036, #25652, #4871, #12367, #22763, #33156, #2319, #20200, #30600, #7265, #25480, #17648, #4697, #2154, #12537, #22927 ),
 .UNSPECIFIED., .F., .F.,
 ( 4, 2, 2, 2, 2, 2, 2, 2, 4 ),
 ( 0.000000000000000000, 0.06249999999999940326, 0.1249999999999987788, 0.1874999999999981681, 0.2499999999999975298, 0.3124999999999981681, 0.3749999999999987788, 0.4374999999999994449, 0.5000000000000000000 ),
 .UNSPECIFIED. ) ;
#17300 = DIRECTION ( 'NONE',  ( 0.000000000000000000, 0.000000000000000000, 1.000000000000000000 ) ) ;
#17301 = CARTESIAN_POINT ( 'NONE',  ( 75.02499999726879309, 149.9369285172503510, -15.58253175000000823 ) ) ;
#17302 = CARTESIAN_POINT ( 'NONE',  ( 22.98492866215539365, -18.48391005502968198, -16.91127448208918338 ) ) ;
#17303 = CARTESIAN_POINT ( 'NONE',  ( 2.517493886308900919, 214.5937144450984420, 79.40113791807858945 ) ) ;
#17304 = DIRECTION ( 'NONE',  ( 0.9945218953682719576, 0.000000000000000000, -0.1045284632676662384 ) ) ;
#17305 = CIRCLE ( 'NONE', #31440, 2.500000000000000000 ) ;
#17306 = CARTESIAN_POINT ( 'NONE',  ( 42.70000000000000284, 163.5228861582408797, -11.73074641843674470 ) ) ;
#17307 = CARTESIAN_POINT ( 'NONE',  ( -8.015496119326597224, 209.5516654185217362, 53.64886208192143613 ) ) ;
#17308 = DIRECTION ( 'NONE',  ( -1.000000000000000000, 0.000000000000000000, -0.000000000000000000 ) ) ;
#17309 = CARTESIAN_POINT ( 'NONE',  ( -7.549004593702459687, 4.358419834287835748, -7.700121441565839220 ) ) ;
#17310 = DIRECTION ( 'NONE',  ( 1.000000000000000000, -0.000000000000000000, -0.000000000000000000 ) ) ;
#17311 = CARTESIAN_POINT ( 'NONE',  ( 50.32499999726881157, 145.8408176439707802, 12.60653300113718345 ) ) ;
#17312 = CARTESIAN_POINT ( 'NONE',  ( 66.77499999726880731, 140.1801316387863778, 4.815267126137185549 ) ) ;
#17313 = CARTESIAN_POINT ( 'NONE',  ( -3.662846001190052991, 218.4274158808045740, 55.10113791807857808 ) ) ;
#17314 = DIRECTION ( 'NONE',  ( -0.2649168722799616349, 0.9642688156137669830, -0.002168413296787739895 ) ) ;
#17315 = AXIS2_PLACEMENT_3D ( 'NONE', #30583, #10144, #2140 ) ;
#17316 = CARTESIAN_POINT ( 'NONE',  ( -3.753561863808691168, 195.6020594897209435, 2.901137918078565470 ) ) ;
#17317 = CARTESIAN_POINT ( 'NONE',  ( -3.044812012440131443, 216.5253028482142952, 82.10113791807857808 ) ) ;
#17318 = AXIS2_PLACEMENT_3D ( 'NONE', #32491, #29777, #27726 ) ;
#17319 = CARTESIAN_POINT ( 'NONE',  ( 0.05014649552828288198, 194.3824533091408000, 37.74886208192143755 ) ) ;
#17320 = CARTESIAN_POINT ( 'NONE',  ( -8.118202686958138514, 212.8392687619910930, 44.79886208192143471 ) ) ;
#17321 = CARTESIAN_POINT ( 'NONE',  ( -6.500000000000000000, 2.536640449112271156, -0.3753468889000206032 ) ) ;
#17322 = CARTESIAN_POINT ( 'NONE',  ( -3.753561863808691168, 195.6020594897209435, 86.90113791807857524 ) ) ;
#17323 = PLANE ( 'NONE',  #3395 ) ;
#17324 = CARTESIAN_POINT ( 'NONE',  ( -0.05014649552810635652, 196.4853777576173002, -0.2488620819214343305 ) ) ;
#17325 = CARTESIAN_POINT ( 'NONE',  ( 3.135527875058981895, 197.5041725223112792, 73.59886208192143897 ) ) ;
#17326 = FACE_OUTER_BOUND ( 'NONE', #14897, .T. ) ;
#17327 = CIRCLE ( 'NONE', #29832, 17.00000000000000711 ) ;
#17328 = ORIENTED_EDGE ( 'NONE', *, *, #26552, .F. ) ;
#17329 = CARTESIAN_POINT ( 'NONE',  ( -7.375838497908014268, 196.7627149292498530, 71.04886208192142760 ) ) ;
#17330 = ORIENTED_EDGE ( 'NONE', *, *, #4490, .T. ) ;
#17331 = CARTESIAN_POINT ( 'NONE',  ( 69.47499999726881015, 160.0630714827496206, -15.58253175000000823 ) ) ;
#17332 = CARTESIAN_POINT ( 'NONE',  ( -4.903702542908436435, 200.1653181626580249, 47.04886208192144892 ) ) ;
#17333 = VERTEX_POINT ( 'NONE', #6213 ) ;
#17334 = CARTESIAN_POINT ( 'NONE',  ( 82.27499999726880731, 160.0630714827496206, 15.58253174999999224 ) ) ;
#17335 = CARTESIAN_POINT ( 'NONE',  ( 74.71132485994280614, 155.0000000000000000, 15.00000000000001243 ) ) ;
#17336 = CARTESIAN_POINT ( 'NONE',  ( 32.50000000000000000, 155.0000000000000000, 15.00000000000001243 ) ) ;
#17337 = AXIS2_PLACEMENT_3D ( 'NONE', #9637, #20032, #30432 ) ;
#17338 = CARTESIAN_POINT ( 'NONE',  ( 56.32499999726881157, 145.8408176439707802, 12.60653300113718345 ) ) ;
#17339 = CARTESIAN_POINT ( 'NONE',  ( 60.63708498984762940, 120.3589838486224579, -20.00000000000000000 ) ) ;
#17340 = AXIS2_PLACEMENT_3D ( 'NONE', #23955, #289, #13389 ) ;
#17341 = CARTESIAN_POINT ( 'NONE',  ( 6.220909254589681581, 198.5229672870052582, 43.44886208192143329 ) ) ;
#17342 = ORIENTED_EDGE ( 'NONE', *, *, #7897, .T. ) ;
#17343 = DIRECTION ( 'NONE',  ( -1.000000000000000000, -0.000000000000000000, -0.000000000000000000 ) ) ;
#17344 = AXIS2_PLACEMENT_3D ( 'NONE', #3259, #5978, #24041 ) ;
#17345 = PLANE ( 'NONE',  #13969 ) ;
#17346 = DIRECTION ( 'NONE',  ( 0.000000000000000000, -0.5000000000000011102, -0.8660254037844379305 ) ) ;
#17347 = CARTESIAN_POINT ( 'NONE',  ( 8.000000000000008882, 207.0476921513415220, 27.99886208192144110 ) ) ;
#17348 = CARTESIAN_POINT ( 'NONE',  ( 9.984503880673470277, 203.7031108863295401, 59.15113791807858235 ) ) ;
#17349 = CARTESIAN_POINT ( 'NONE',  ( -3.135527875058821579, 197.5041725223112223, 47.90113791807857524 ) ) ;
#17350 = CARTESIAN_POINT ( 'NONE',  ( 66.98867513459482836, 163.8167787843871110, -12.13525491562423397 ) ) ;
#17351 = AXIS2_PLACEMENT_3D ( 'NONE', #1724, #10092, #1564 ) ;
#17352 = CONTEXT_DEPENDENT_SHAPE_REPRESENTATION ( #24451, #5451 ) ;
#17353 = CARTESIAN_POINT ( 'NONE',  ( -6.220909254589537696, 198.5229672870051161, 18.05113791807856671 ) ) ;
#17354 = CARTESIAN_POINT ( 'NONE',  ( 4.984841277089725686, 213.7757310962907411, 1.551137918078566047 ) ) ;
#17355 = CARTESIAN_POINT ( 'NONE',  ( 43.62499999726880162, 171.3844434931184253, -7.942151717890132712E-15 ) ) ;
#17356 = CARTESIAN_POINT ( 'NONE',  ( 34.82499999726881157, 141.7447067706911810, -9.630534252274387086 ) ) ;
#17357 = CARTESIAN_POINT ( 'NONE',  ( 11.98450388067348271, 203.0532714938637753, 32.15113791807856103 ) ) ;
#17358 = PLANE ( 'NONE',  #11858 ) ;
#17359 = CARTESIAN_POINT ( 'NONE',  ( 8.118202686958039038, 212.8392687619912635, 79.70113791807857240 ) ) ;
#17360 = CARTESIAN_POINT ( 'NONE',  ( -3.044812012440131443, 216.5253028482142952, 46.10113791807857098 ) ) ;
#17361 = DIRECTION ( 'NONE',  ( 1.000000000000000000, 0.000000000000000000, 0.000000000000000000 ) ) ;
#17362 = CARTESIAN_POINT ( 'NONE',  ( 34.78867513459482552, 155.0000000000000000, -15.00000000000002487 ) ) ;
#17363 = CARTESIAN_POINT ( 'NONE',  ( 12.01549611932659367, 203.1486557965466773, 13.14886208192143613 ) ) ;
#17364 = CARTESIAN_POINT ( 'NONE',  ( 6.139770520408223575, 215.5359834540460611, 18.54886208192143826 ) ) ;
#17365 = CARTESIAN_POINT ( 'NONE',  ( 75.59999999453764019, 141.2096805137202580, -4.480746418436742040 ) ) ;
#17366 = ORIENTED_EDGE ( 'NONE', *, *, #31990, .T. ) ;
#17367 = CARTESIAN_POINT ( 'NONE',  ( 11.98450388067348271, 203.0532714938637753, 62.15113791807858945 ) ) ;
#17368 = CIRCLE ( 'NONE', #1579, 12.10452846326767684 ) ;
#17369 = CARTESIAN_POINT ( 'NONE',  ( -0.05014649552807731031, 198.5883022060938572, 74.75113791807856956 ) ) ;
#17370 = CARTESIAN_POINT ( 'NONE',  ( 3.044812012439969795, 216.5253028482143520, 33.39886208192143613 ) ) ;
#17371 = SURFACE_STYLE_FILL_AREA ( #17027 ) ;
#17372 = ORIENTED_EDGE ( 'NONE', *, *, #13328, .T. ) ;
#17373 = ORIENTED_EDGE ( 'NONE', *, *, #17229, .T. ) ;
#17374 = VERTEX_POINT ( 'NONE', #16601 ) ;
#17375 = EDGE_CURVE ( 'NONE', #8324, #10227, #28836, .T. ) ;
#17376 = DIRECTION ( 'NONE',  ( 0.000000000000000000, 0.000000000000000000, -1.000000000000000000 ) ) ;
#17377 = CARTESIAN_POINT ( 'NONE',  ( 108.1100194822685836, 155.0000000000000000, 13.00000000000003908 ) ) ;
#17378 = ORIENTED_EDGE ( 'NONE', *, *, #15438, .T. ) ;
#17379 = CARTESIAN_POINT ( 'NONE',  ( 2.517493886308900919, 214.5937144450984420, 31.40113791807857879 ) ) ;
#17380 = CYLINDRICAL_SURFACE ( 'NONE', #15616, 31.00000000000000000 ) ;
#17381 = CARTESIAN_POINT ( 'NONE',  ( -0.05014649552828403384, 217.5146222423826714, 12.24886208192143755 ) ) ;
#17382 = CARTESIAN_POINT ( 'NONE',  ( 56.87499999726880162, 138.6155565068815747, -3.929120461958505118E-15 ) ) ;
#17383 = ORIENTED_EDGE ( 'NONE', *, *, #23038, .F. ) ;
#17384 = CARTESIAN_POINT ( 'NONE',  ( 2.517493886308900919, 214.5937144450984420, 49.40113791807856813 ) ) ;
#17385 = CARTESIAN_POINT ( 'NONE',  ( -47.49999999999998579, 155.0000000000000000, 11.99999999999999645 ) ) ;
#17386 = DIRECTION ( 'NONE',  ( -1.000000000000000000, -0.000000000000000000, -0.000000000000000000 ) ) ;
#17387 = VECTOR ( 'NONE', #28132, 1000.000000000000000 ) ;
#17388 = CARTESIAN_POINT ( 'NONE',  ( -8.118202686958138514, 212.8392687619910930, 98.79886208192144181 ) ) ;
#17389 = CARTESIAN_POINT ( 'NONE',  ( 66.17499999726881299, 164.1591823560292198, 12.60653300113718167 ) ) ;
#17390 = CARTESIAN_POINT ( 'NONE',  ( -6.139770520408369237, 215.5359834540460042, 36.95113791807857240 ) ) ;
#17391 = CARTESIAN_POINT ( 'NONE',  ( -8.062137200540920645, 212.9164362838581894, 15.80113791807856849 ) ) ;
#17392 = DIRECTION ( 'NONE',  ( 0.000000000000000000, 0.7071067811865437980, -0.7071067811865512365 ) ) ;
#17393 = CARTESIAN_POINT ( 'NONE',  ( 77.10000000000000853, 168.7903194862797420, 4.480746418436729606 ) ) ;
#17394 = CARTESIAN_POINT ( 'NONE',  ( -56.61815514298172758, 194.9659613751070140, -1.653849335561433209 ) ) ;
#17395 = CARTESIAN_POINT ( 'NONE',  ( 42.49999999999999289, -72.99999999999998579, -51.04834939252008041 ) ) ;
#17396 = CARTESIAN_POINT ( 'NONE',  ( 8.062137200540920645, 201.0835637161417822, 101.3011379180785809 ) ) ;
#17397 = FACE_OUTER_BOUND ( 'NONE', #9608, .T. ) ;
#17398 = CARTESIAN_POINT ( 'NONE',  ( 50.57499999726881157, 145.8408176439707802, 12.60653300113718345 ) ) ;
#17399 = CARTESIAN_POINT ( 'NONE',  ( 10.01549611932653860, 210.2015048109876716, 43.85113791807854966 ) ) ;
#17400 = CARTESIAN_POINT ( 'NONE',  ( 83.62499999726881583, 171.3844434931184253, -7.942151717890132712E-15 ) ) ;
#17401 = CARTESIAN_POINT ( 'NONE',  ( -0.6511518506208974211, 8.763486134561267349, -7.907570769506047981 ) ) ;
#17402 = DIRECTION ( 'NONE',  ( 0.000000000000000000, 1.000000000000000000, -1.290957005378097920E-14 ) ) ;
#17403 = CARTESIAN_POINT ( 'NONE',  ( 48.49999999453761745, 170.2462022514548323, -7.872454543227099337E-15 ) ) ;
#17404 = ORIENTED_EDGE ( 'NONE', *, *, #7089, .T. ) ;
#17405 =( BOUNDED_SURFACE ( )  B_SPLINE_SURFACE ( 3, 2, ( 
 ( #15221, #30046, #32761 ),
 ( #19825, #7393, #17774 ),
 ( #27489, #25611, #6712 ),
 ( #2277, #4144, #14538 ),
 ( #33110, #22721, #9776 ),
 ( #14878, #17607, #30557 ),
 ( #15047, #2115, #1759 ),
 ( #27997, #9433, #1597 ) ),
 .UNSPECIFIED., .F., .F., .T. ) 
 B_SPLINE_SURFACE_WITH_KNOTS ( ( 4, 2, 2, 4 ),
 ( 3, 3 ),
 ( 0.03861844051980969916, 0.04325213341840641879, 0.04556897986770477860, 0.04788582631700313841 ),
 ( 0.000000000000000000, 1.000000000000000000 ),
 .UNSPECIFIED. ) 
 GEOMETRIC_REPRESENTATION_ITEM ( )  RATIONAL_B_SPLINE_SURFACE ( (
 ( 1.000000000000000000, 0.8047781759831920123, 1.000000000000000000),
 ( 1.000000000000000000, 0.8123762462803147955, 1.000000000000000000),
 ( 1.000000000000000000, 0.8190659850619289584, 1.000000000000000000),
 ( 1.000000000000000000, 0.8191937571012362085, 1.000000000000000000),
 ( 1.000000000000000000, 0.8176092952779873135, 1.000000000000000000),
 ( 1.000000000000000000, 0.8122962088597077690, 1.000000000000000000),
 ( 1.000000000000000000, 0.8086311330827508081, 1.000000000000000000),
 ( 1.000000000000000000, 0.8047712282214326551, 1.000000000000000000) ) ) 
 REPRESENTATION_ITEM ( '' )  SURFACE ( )  );
#17406 = CARTESIAN_POINT ( 'NONE',  ( 9.680171189290831535, 199.9079932115568852, 29.30113791807857027 ) ) ;
#17407 = CARTESIAN_POINT ( 'NONE',  ( 61.41132485994281609, 142.2402378747194405, -9.270509831248439525 ) ) ;
#17408 = CARTESIAN_POINT ( 'NONE',  ( 8.118202686958138514, 201.1607312380088501, 4.298862081921434708 ) ) ;
#17409 = CARTESIAN_POINT ( 'NONE',  ( -9.658740382312574368, 207.9902050807892522, 102.7419814567561360 ) ) ;
#17410 = ORIENTED_EDGE ( 'NONE', *, *, #32838, .T. ) ;
#17411 = CARTESIAN_POINT ( 'NONE',  ( 9.984503880673470277, 203.7031108863295401, 5.151137918078567246 ) ) ;
#17412 = CARTESIAN_POINT ( 'NONE',  ( 3.044812012440130555, 197.4746971517856764, 65.60113791807857808 ) ) ;
#17413 = CARTESIAN_POINT ( 'NONE',  ( 6.444103211790928043, 211.7408657792734061, 27.69886208192143684 ) ) ;
#17414 = EDGE_CURVE ( 'NONE', #27498, #3666, #33125, .T. ) ;
#17415 = CARTESIAN_POINT ( 'NONE',  ( 90.49452189536829394, 155.0000000000000000, 0.000000000000000000 ) ) ;
#17416 = ORIENTED_EDGE ( 'NONE', *, *, #13146, .T. ) ;
#17417 = CARTESIAN_POINT ( 'NONE',  ( 4.903702542908601636, 200.1653181626581102, -0.5488620819214340418 ) ) ;
#17418 = CARTESIAN_POINT ( 'NONE',  ( -58.50000000000002132, 185.0000000000000000, 0.000000000000000000 ) ) ;
#17419 = CARTESIAN_POINT ( 'NONE',  ( 9.680171189290716072, 214.0920067884432854, 90.69886208192143329 ) ) ;
#17420 = CARTESIAN_POINT ( 'NONE',  ( 38.07499999726880446, 168.2552932293087906, 9.630534252274372875 ) ) ;
#17421 = EDGE_LOOP ( 'NONE', ( #6567, #27624, #7831, #16438 ) ) ;
#17422 = CARTESIAN_POINT ( 'NONE',  ( 45.32499999726881157, 164.1591823560292198, -12.60653300113719766 ) ) ;
#17423 = DIRECTION ( 'NONE',  ( 0.000000000000000000, 0.000000000000000000, 1.000000000000000000 ) ) ;
#17424 = EDGE_CURVE ( 'NONE', #13306, #33027, #20278, .T. ) ;
#17425 = CARTESIAN_POINT ( 'NONE',  ( 54.11132485994280472, 169.2658477444273331, -4.635254915624224203 ) ) ;
#17426 = CARTESIAN_POINT ( 'NONE',  ( -10.01549611932659722, 210.2015048109875011, 71.64886208192143613 ) ) ;
#17427 = CARTESIAN_POINT ( 'NONE',  ( 48.57499999726881157, 145.8408176439707802, 12.60653300113718345 ) ) ;
#17428 = DIRECTION ( 'NONE',  ( -1.000000000000000000, -0.000000000000000000, -0.000000000000000000 ) ) ;
#17429 = CARTESIAN_POINT ( 'NONE',  ( 10.01549611932653860, 210.2015048109876716, 7.851137918078566535 ) ) ;
#17430 = DIRECTION ( 'NONE',  ( 1.000000000000000000, 0.000000000000000000, 0.000000000000000000 ) ) ;
#17431 = CARTESIAN_POINT ( 'NONE',  ( 58.80000000000000426, 167.3344367211045096, -8.961492836873482304 ) ) ;
#17432 = CARTESIAN_POINT ( 'NONE',  ( 8.118202686958039038, 212.8392687619912635, 85.70113791807858661 ) ) ;
#17433 = DIRECTION ( 'NONE',  ( 0.000000000000000000, 0.000000000000000000, 1.000000000000000000 ) ) ;
#17434 = CARTESIAN_POINT ( 'NONE',  ( 0.000000000000000000, 0.000000000000000000, -2.899999999999999911 ) ) ;
#17435 = CARTESIAN_POINT ( 'NONE',  ( 27.50000000000000000, 13.30988860919481809, -1.715101482986582715 ) ) ;
#17436 = EDGE_CURVE ( 'NONE', #20186, #20607, #12596, .T. ) ;
#17437 = CARTESIAN_POINT ( 'NONE',  ( -11.98450388067341876, 203.0532714938636047, 89.34886208192143897 ) ) ;
#17438 = CARTESIAN_POINT ( 'NONE',  ( 65.42499999726881299, 168.2552932293087906, -9.630534252274385310 ) ) ;
#17440 = ORIENTED_EDGE ( 'NONE', *, *, #28348, .T. ) ;
#17439 = CARTESIAN_POINT ( 'NONE',  ( -10.01549611932653860, 203.7984951890123000, 24.35113791807856387 ) ) ;
#17441 = CARTESIAN_POINT ( 'NONE',  ( 121.3406204335659879, 155.0000000000000000, -6.938893903907228378E-15 ) ) ;
#17442 = CARTESIAN_POINT ( 'NONE',  ( 84.77499999726880731, 140.1801316387863778, 4.815267126137185549 ) ) ;
#17443 = CARTESIAN_POINT ( 'NONE',  ( 12.00000000000000711, 206.9523078486586485, 86.00113791807856956 ) ) ;
#17444 = EDGE_CURVE ( 'NONE', #14311, #14728, #7235, .T. ) ;
#17445 = CARTESIAN_POINT ( 'NONE',  ( 5.000000000000000000, -4.685197434473814759, 3.903127820947815962E-15 ) ) ;
#17446 = AXIS2_PLACEMENT_3D ( 'NONE', #28303, #31033, #8025 ) ;
#17447 = ORIENTED_EDGE ( 'NONE', *, *, #1692, .F. ) ;
#17448 = CARTESIAN_POINT ( 'NONE',  ( 9.680171189290716072, 214.0920067884432854, 69.69886208192143329 ) ) ;
#17449 = CARTESIAN_POINT ( 'NONE',  ( -6.139770520408224463, 198.4640165459539105, 74.04886208192144181 ) ) ;
#17450 = CARTESIAN_POINT ( 'NONE',  ( -9.680171189290716072, 199.9079932115567146, 14.19886208192143684 ) ) ;
#17451 = DIRECTION ( 'NONE',  ( -1.000000000000000000, 0.000000000000000000, -0.000000000000000000 ) ) ;
#17452 = CARTESIAN_POINT ( 'NONE',  ( -6.139770520408369237, 215.5359834540460042, 36.95113791807857240 ) ) ;
#17453 = CARTESIAN_POINT ( 'NONE',  ( 94.70964751525852421, 155.0000000000000000, -32.10452846326766974 ) ) ;
#17454 = CARTESIAN_POINT ( 'NONE',  ( 3.135527875058981895, 197.5041725223112792, 94.59886208192143897 ) ) ;
#17455 = ADVANCED_FACE ( 'NONE', ( #32777, #15061 ), #14722, .T. ) ;
#17456 = CARTESIAN_POINT ( 'NONE',  ( 32.50000000000000000, 155.0000000000000000, -6.938893903907228378E-15 ) ) ;
#17457 = ORIENTED_EDGE ( 'NONE', *, *, #10604, .F. ) ;
#17458 = LINE ( 'NONE', #14902, #18393 ) ;
#17459 = CARTESIAN_POINT ( 'NONE',  ( -6.500168698208244500, 211.6636982574061676, 83.79886208192144181 ) ) ;
#17460 = ORIENTED_EDGE ( 'NONE', *, *, #30591, .T. ) ;
#17461 = CARTESIAN_POINT ( 'NONE',  ( -67.50000000000000000, 155.0000000000000000, 6.938893903907228378E-15 ) ) ;
#17462 = VERTEX_POINT ( 'NONE', #22903 ) ;
#17463 = CARTESIAN_POINT ( 'NONE',  ( 81.01132485994281751, 142.2402378747194405, 9.270509831248432420 ) ) ;
#17464 = CARTESIAN_POINT ( 'NONE',  ( 85.32499999726880446, 164.1591823560292198, -12.60653300113719766 ) ) ;
#17465 = FACE_BOUND ( 'NONE', #22519, .T. ) ;
#17466 = CARTESIAN_POINT ( 'NONE',  ( -6.500168698208129925, 202.3363017425936050, 75.20113791807857240 ) ) ;
#17467 = EDGE_CURVE ( 'NONE', #11974, #3872, #27334, .T. ) ;
#17468 = DIRECTION ( 'NONE',  ( 0.000000000000000000, 0.000000000000000000, -1.000000000000000000 ) ) ;
#17469 = CARTESIAN_POINT ( 'NONE',  ( 38.90000000000000568, 168.7903194862797420, -4.480746418436745593 ) ) ;
#17470 = CARTESIAN_POINT ( 'NONE',  ( 8.015496119326595448, 204.4483345814782638, 49.14886208192145034 ) ) ;
#17471 = EDGE_CURVE ( 'NONE', #25247, #26344, #26264, .T. ) ;
#17472 = CARTESIAN_POINT ( 'NONE',  ( -7.500000000000000000, 4.330127018922191873, -10.00000000000000000 ) ) ;
#17473 = CARTESIAN_POINT ( 'NONE',  ( 72.81132485994282888, 150.1262045565064227, 15.00000000000001599 ) ) ;
#17474 = DIRECTION ( 'NONE',  ( 0.000000000000000000, -0.000000000000000000, 1.000000000000000000 ) ) ;
#17475 = CARTESIAN_POINT ( 'NONE',  ( 51.42499999726879878, 168.2552932293087906, -9.630534252274387086 ) ) ;
#17476 = CARTESIAN_POINT ( 'NONE',  ( 62.07499999726881157, 168.2552932293087906, 9.630534252274372875 ) ) ;
#17477 = CARTESIAN_POINT ( 'NONE',  ( -11.98450388067348804, 210.9467285061362247, 57.65113791807858945 ) ) ;
#17478 = LINE ( 'NONE', #21912, #2655 ) ;
#17479 = CARTESIAN_POINT ( 'NONE',  ( -3.044812012440131443, 216.5253028482142952, 100.1011379180785781 ) ) ;
#17480 = CARTESIAN_POINT ( 'NONE',  ( 8.118202686958039038, 212.8392687619912635, 82.70113791807857240 ) ) ;
#17481 = CARTESIAN_POINT ( 'NONE',  ( 9.736236675708031640, 199.9851607334238963, 46.29886208192144181 ) ) ;
#17482 = CARTESIAN_POINT ( 'NONE',  ( 8.062137200540822946, 212.9164362838583315, 45.69886208192143329 ) ) ;
#17483 = DIRECTION ( 'NONE',  ( -1.000000000000000000, 0.000000000000000000, 0.000000000000000000 ) ) ;
#17484 = CARTESIAN_POINT ( 'NONE',  ( -12.01549611932652972, 203.1486557965464499, 87.35113791807857808 ) ) ;
#17485 = CARTESIAN_POINT ( 'NONE',  ( 83.11132485994279762, 140.7341522555726669, 4.635254915624211769 ) ) ;
#17486 = CARTESIAN_POINT ( 'NONE',  ( -3.135527875058821579, 197.5041725223112223, 2.901137918078565914 ) ) ;
#17487 = CARTESIAN_POINT ( 'NONE',  ( -8.062137200540822946, 201.0835637161416400, 71.19886208192144750 ) ) ;
#17488 = DIRECTION ( 'NONE',  ( -0.000000000000000000, -0.000000000000000000, 1.000000000000000000 ) ) ;
#17489 = ORIENTED_EDGE ( 'NONE', *, *, #21478, .T. ) ;
#17490 = CARTESIAN_POINT ( 'NONE',  ( -0.05014649552828442242, 219.6175466908591716, 72.24886208192143044 ) ) ;
#17491 = AXIS2_PLACEMENT_3D ( 'NONE', #27995, #27652, #20331 ) ;
#17492 = ORIENTED_EDGE ( 'NONE', *, *, #5854, .T. ) ;
#17493 = CARTESIAN_POINT ( 'NONE',  ( 80.77499999726880731, 140.1801316387863778, 4.815267126137185549 ) ) ;
#17494 = CARTESIAN_POINT ( 'NONE',  ( 4.903702542908435547, 213.8346818373419751, 51.54886208192144181 ) ) ;
#17495 = VERTEX_POINT ( 'NONE', #6555 ) ;
#17496 = CARTESIAN_POINT ( 'NONE',  ( 74.12499999726881583, 155.0000000000000000, 15.58253174999999402 ) ) ;
#17497 = CARTESIAN_POINT ( 'NONE',  ( 6.500000000000001776, -4.012858516023013244, -6.470130706010830401 ) ) ;
#17498 = CARTESIAN_POINT ( 'NONE',  ( 71.71132485994280614, 155.0000000000000000, -15.00000000000002487 ) ) ;
#17499 = AXIS2_PLACEMENT_3D ( 'NONE', #9638, #7093, #22081 ) ;
#17500 = CARTESIAN_POINT ( 'NONE',  ( 59.82499999726879736, 168.2552932293087906, 9.630534252274372875 ) ) ;
#17501 = ADVANCED_FACE ( 'NONE', ( #17119 ), #33297, .F. ) ;
#17502 = CARTESIAN_POINT ( 'NONE',  ( 125.5000000000000000, 154.9999999999996305, -106.0000000000000142 ) ) ;
#17503 = EDGE_CURVE ( 'NONE', #16763, #21649, #9958, .T. ) ;
#17504 = CARTESIAN_POINT ( 'NONE',  ( -9.984503880673420539, 203.7031108863293980, 44.34886208192142476 ) ) ;
#17505 = VERTEX_POINT ( 'NONE', #30235 ) ;
#17506 = CARTESIAN_POINT ( 'NONE',  ( 92.60208470531341618, 155.0000000000000000, 0.000000000000000000 ) ) ;
#17507 = DIRECTION ( 'NONE',  ( 0.000000000000000000, 1.000000000000000000, 0.000000000000000000 ) ) ;
#17508 = CARTESIAN_POINT ( 'NONE',  ( 68.71132485994280614, 155.0000000000000000, 15.00000000000001243 ) ) ;
#17509 = CARTESIAN_POINT ( 'NONE',  ( 2.517493886309087436, 199.4062855549015865, 28.59886208192143897 ) ) ;
#17510 = CARTESIAN_POINT ( 'NONE',  ( -6.220909254589537696, 198.5229672870051161, 72.05113791807853829 ) ) ;
#17511 = CARTESIAN_POINT ( 'NONE',  ( 115.4999999999999858, 246.7986928011511907, 52.99999999999882760 ) ) ;
#17512 = EDGE_CURVE ( 'NONE', #6439, #20904, #14289, .T. ) ;
#17513 = CARTESIAN_POINT ( 'NONE',  ( 0.05014649552810505201, 217.5146222423826714, 43.25113791807856956 ) ) ;
#17514 = CONTEXT_DEPENDENT_SHAPE_REPRESENTATION ( #19220, #21227 ) ;
#17515 = CARTESIAN_POINT ( 'NONE',  ( -10.01549611932653860, 203.7984951890123284, 18.35113791807856742 ) ) ;
#17516 = AXIS2_PLACEMENT_3D ( 'NONE', #22165, #14833, #17056 ) ;
#17517 = CARTESIAN_POINT ( 'NONE',  ( 6.500168698208129925, 211.6636982574063381, 1.701137918078565958 ) ) ;
#17518 = CARTESIAN_POINT ( 'NONE',  ( 53.32499999726881157, 164.1591823560292198, -12.60653300113719766 ) ) ;
#17519 = CARTESIAN_POINT ( 'NONE',  ( 87.50000000000002842, 156.3310307509052279, -15.36965516068564597 ) ) ;
#17520 = CARTESIAN_POINT ( 'NONE',  ( -7.456977232089304408, 196.8216656703010301, 30.05113791807857027 ) ) ;
#17521 = DIRECTION ( 'NONE',  ( -0.1045284632676344722, 0.000000000000000000, 0.9945218953682752883 ) ) ;
#17522 = B_SPLINE_CURVE_WITH_KNOTS ( 'NONE', 3,
 ( #5164, #15387, #5328, #23722, #7900, #23399, #15551, #10625, #18281, #21162 ),
 .UNSPECIFIED., .F., .F.,
 ( 4, 2, 2, 2, 4 ),
 ( 0.01606529487141864984, 0.01806591702017408541, 0.02006653916892951403, 0.02406778346644038169, 0.03207027206146211007 ),
 .UNSPECIFIED. ) ;
#17523 = CARTESIAN_POINT ( 'NONE',  ( 6.139770520408368348, 198.4640165459539674, 80.45113791807857240 ) ) ;
#17524 = CARTESIAN_POINT ( 'NONE',  ( 8.062137200540920645, 201.0835637161417822, 47.30113791807857382 ) ) ;
#17525 = UNCERTAINTY_MEASURE_WITH_UNIT (LENGTH_MEASURE( 1.000000000000000082E-05 ), #12784, 'distance_accuracy_value', 'NONE');
#17526 = FACE_OUTER_BOUND ( 'NONE', #3149, .T. ) ;
#17527 = CARTESIAN_POINT ( 'NONE',  ( 84.98867513459481415, 163.8167787843871110, -12.13525491562423397 ) ) ;
#17528 = CARTESIAN_POINT ( 'NONE',  ( -7.375838497908014268, 196.7627149292498530, 14.04886208192143471 ) ) ;
#17529 = CARTESIAN_POINT ( 'NONE',  ( -6.220909254589682469, 215.4770327129947134, 20.94886208192143684 ) ) ;
#17530 = CARTESIAN_POINT ( 'NONE',  ( 70.99999999453763166, 155.0000000000000000, 14.49999999999999467 ) ) ;
#17531 = AXIS2_PLACEMENT_3D ( 'NONE', #18696, #6238, #21410 ) ;
#17532 = ORIENTED_EDGE ( 'NONE', *, *, #11366, .T. ) ;
#17533 = CARTESIAN_POINT ( 'NONE',  ( 9.680171189290831535, 199.9079932115568852, 59.30113791807857382 ) ) ;
#17534 = CARTESIAN_POINT ( 'NONE',  ( -2.426778023690262742, 214.6231898156240163, 79.10113791807857808 ) ) ;
#17535 = CARTESIAN_POINT ( 'NONE',  ( -6.220909254589682469, 215.4770327129946850, 41.94886208192144039 ) ) ;
#17536 = CARTESIAN_POINT ( 'NONE',  ( 74.81132485994281467, 150.1262045565064227, 15.00000000000001599 ) ) ;
#17537 = ORIENTED_EDGE ( 'NONE', *, *, #29987, .F. ) ;
#17538 = EDGE_LOOP ( 'NONE', ( #9240, #33261, #8619, #27469 ) ) ;
#17539 = VERTEX_POINT ( 'NONE', #24787 ) ;
#17540 = CARTESIAN_POINT ( 'NONE',  ( -63.49999999999884892, 215.0000000000000000, -2.500000000000000000 ) ) ;
#17541 = AXIS2_PLACEMENT_3D ( 'NONE', #8423, #18809, #29202 ) ;
#17542 = DIRECTION ( 'NONE',  ( -1.000000000000000000, -0.000000000000000000, -0.000000000000000000 ) ) ;
#17543 = ORIENTED_EDGE ( 'NONE', *, *, #26586, .T. ) ;
#17544 = CARTESIAN_POINT ( 'NONE',  ( 8.000000000000008882, 206.9523078486586485, 35.00113791807857666 ) ) ;
#17545 = CARTESIAN_POINT ( 'NONE',  ( 6.139770520408223575, 215.5359834540460611, 9.548862081921431155 ) ) ;
#17546 = CARTESIAN_POINT ( 'NONE',  ( 54.77499999726881441, 140.1801316387863778, 4.815267126137185549 ) ) ;
#17547 = ORIENTED_EDGE ( 'NONE', *, *, #299, .F. ) ;
#17548 = CARTESIAN_POINT ( 'NONE',  ( 8.000000000000008882, 206.9523078486586485, 56.00113791807857666 ) ) ;
#17549 = DIRECTION ( 'NONE',  ( 1.000000000000000000, 0.000000000000000000, 0.000000000000000000 ) ) ;
#17550 = AXIS2_PLACEMENT_3D ( 'NONE', #22412, #1306, #17308 ) ;
#17551 = FILL_AREA_STYLE ('',( #7514 ) ) ;
#17552 = CARTESIAN_POINT ( 'NONE',  ( 0.000000000000000000, 0.000000000000000000, 0.000000000000000000 ) ) ;
#17553 = CARTESIAN_POINT ( 'NONE',  ( -6.220909254589682469, 215.4770327129946850, 95.94886208192143329 ) ) ;
#17554 = AXIS2_PLACEMENT_3D ( 'NONE', #27670, #4504, #25113 ) ;
#17555 = CARTESIAN_POINT ( 'NONE',  ( 64.07499999726881867, 168.2552932293087906, 9.630534252274372875 ) ) ;
#17556 = CARTESIAN_POINT ( 'NONE',  ( -6.220909254589537696, 198.5229672870051161, 36.05113791807857382 ) ) ;
#17557 = CARTESIAN_POINT ( 'NONE',  ( -2.927447417349541059, 2.351289329882138457, -0.1217565302851113529 ) ) ;
#17558 = CARTESIAN_POINT ( 'NONE',  ( 9.984503880673470277, 203.7031108863295401, 14.15113791807856458 ) ) ;
#17559 = DIRECTION ( 'NONE',  ( 1.000000000000000000, 0.000000000000000000, 0.000000000000000000 ) ) ;
#17560 = CARTESIAN_POINT ( 'NONE',  ( 85.70000000000000284, 146.4771138417591203, 11.73074641843673227 ) ) ;
#17561 = CARTESIAN_POINT ( 'NONE',  ( 4.250000000000000000, 0.000000000000000000, -0.5251556536572846712 ) ) ;
#17562 = CARTESIAN_POINT ( 'NONE',  ( 3.499999999999993339, -2.020725942163723143, -0.3126073911696551910 ) ) ;
#17563 = CARTESIAN_POINT ( 'NONE',  ( -11.98450388067348804, 210.9467285061362247, 0.6511379180785656917 ) ) ;
#17564 = LINE ( 'NONE', #25234, #18930 ) ;
#17565 = CARTESIAN_POINT ( 'NONE',  ( 52.57499999726881157, 145.8408176439707802, 12.60653300113718345 ) ) ;
#17566 = CARTESIAN_POINT ( 'NONE',  ( 6.220909254589536808, 215.4770327129947702, 46.55113791807856671 ) ) ;
#17567 = CARTESIAN_POINT ( 'NONE',  ( 83.92499999726882720, 164.1591823560292198, 12.60653300113718167 ) ) ;
#17568 = VECTOR ( 'NONE', #6285, 999.9999999999998863 ) ;
#17569 = LINE ( 'NONE', #15354, #12481 ) ;
#17570 = DIRECTION ( 'NONE',  ( 1.000000000000000000, 0.000000000000000000, 0.000000000000000000 ) ) ;
#17571 = CARTESIAN_POINT ( 'NONE',  ( 51.09999999453761887, 150.2886644046228639, 14.49999999999999645 ) ) ;
#17572 = ORIENTED_EDGE ( 'NONE', *, *, #10155, .F. ) ;
#17573 = CARTESIAN_POINT ( 'NONE',  ( 3.662846001190051659, 195.5725841191953691, 32.60113791807857098 ) ) ;
#17574 = DIRECTION ( 'NONE',  ( 1.000000000000000000, 0.000000000000000000, 0.000000000000000000 ) ) ;
#17575 = CARTESIAN_POINT ( 'NONE',  ( -0.05014649552828403384, 217.5146222423826714, 9.248862081921432221 ) ) ;
#17576 = DIRECTION ( 'NONE',  ( -1.000000000000000000, -0.000000000000000000, -0.000000000000000000 ) ) ;
#17577 = ORIENTED_EDGE ( 'NONE', *, *, #6042, .F. ) ;
#17578 = AXIS2_PLACEMENT_3D ( 'NONE', #26848, #18846, #8787 ) ;
#17579 = CARTESIAN_POINT ( 'NONE',  ( -3.135527875058821579, 197.5041725223112223, 2.901137918078565914 ) ) ;
#17580 = CARTESIAN_POINT ( 'NONE',  ( -8.062137200540920645, 212.9164362838581894, 57.80113791807857382 ) ) ;
#17581 = VECTOR ( 'NONE', #5347, 1000.000000000000000 ) ;
#17582 = ORIENTED_EDGE ( 'NONE', *, *, #27856, .T. ) ;
#17583 = CARTESIAN_POINT ( 'NONE',  ( -8.000000000000008882, 206.9523078486584780, 23.49886208192144110 ) ) ;
#17584 = AXIS2_PLACEMENT_3D ( 'NONE', #26348, #3010, #8292 ) ;
#17585 = CARTESIAN_POINT ( 'NONE',  ( -63.50000000000001421, 210.0000000000000000, 0.000000000000000000 ) ) ;
#17586 = ORIENTED_EDGE ( 'NONE', *, *, #12723, .F. ) ;
#17587 = CARTESIAN_POINT ( 'NONE',  ( 6.500168698208129925, 211.6636982574063381, 4.701137918078565292 ) ) ;
#17588 = CYLINDRICAL_SURFACE ( 'NONE', #13781, 2.500000000000000000 ) ;
#17589 = CARTESIAN_POINT ( 'NONE',  ( -7.456977232089471386, 217.1783343296987709, 86.94886208192144750 ) ) ;
#17590 = CARTESIAN_POINT ( 'NONE',  ( 36.77499999726881441, 140.1801316387863778, 4.815267126137185549 ) ) ;
#17591 = ORIENTED_EDGE ( 'NONE', *, *, #1239, .T. ) ;
#17592 = CARTESIAN_POINT ( 'NONE',  ( 43.62499999726880162, 171.3844434931184253, -7.942151717890132712E-15 ) ) ;
#17593 = DIRECTION ( 'NONE',  ( 0.000000000000000000, 0.4999999999999993339, -0.8660254037844389297 ) ) ;
#17594 = CARTESIAN_POINT ( 'NONE',  ( -0.05014649552810635652, 196.4853777576173002, 2.751137918078565114 ) ) ;
#17595 = AXIS2_PLACEMENT_3D ( 'NONE', #26146, #9981, #10491 ) ;
#17596 = CARTESIAN_POINT ( 'NONE',  ( -10.00000000000000711, 206.9523078486584495, 74.49886208192144466 ) ) ;
#17597 = CARTESIAN_POINT ( 'NONE',  ( 48.87499999726880873, 138.6155565068815463, -3.929120461958505118E-15 ) ) ;
#17598 = CARTESIAN_POINT ( 'NONE',  ( -67.50001199999998391, 138.1095834939503106, -2.225267283893253012 ) ) ;
#17599 = CARTESIAN_POINT ( 'NONE',  ( 8.062137200540920645, 201.0835637161417822, 2.301137918078566269 ) ) ;
#17600 = CARTESIAN_POINT ( 'NONE',  ( 6.500000000000000000, 3.149025070564758888, -0.5705737632551094451 ) ) ;
#17601 = AXIS2_PLACEMENT_3D ( 'NONE', #32894, #20286, #7177 ) ;
#17602 = CARTESIAN_POINT ( 'NONE',  ( 59.89999999999999858, 141.2096805137202580, 4.480746418436733158 ) ) ;
#17603 = CARTESIAN_POINT ( 'NONE',  ( 8.062137200540920645, 201.0835637161417822, 92.30113791807858092 ) ) ;
#17604 = CARTESIAN_POINT ( 'NONE',  ( -2.926493552096033124, -2.351840044243060035, -0.1388410611046252408 ) ) ;
#17605 = SHAPE_REPRESENTATION ( 'High-Force Belleville Spring Washer Pack', ( #2404 ), #30714 ) ;
#17606 = CARTESIAN_POINT ( 'NONE',  ( 6.220909254589536808, 215.4770327129947702, 79.55113791807855250 ) ) ;
#17607 = CARTESIAN_POINT ( 'NONE',  ( -6.439685834476978954, 4.942299687812971243, -7.659344964963200830 ) ) ;
#17608 = CIRCLE ( 'NONE', #30100, 100.0000000000000284 ) ;
#17609 = DIRECTION ( 'NONE',  ( -0.9891821073486152249, -0.1466927349985424900, -2.962715634069391535E-17 ) ) ;
#17610 = CARTESIAN_POINT ( 'NONE',  ( -3.753561863808878130, 218.3979405102790281, 84.09886208192143897 ) ) ;
#17611 = ADVANCED_FACE ( 'NONE', ( #11838 ), #22223, .T. ) ;
#17612 = AXIS2_PLACEMENT_3D ( 'NONE', #27293, #12128, #25074 ) ;
#17613 = CARTESIAN_POINT ( 'NONE',  ( 64.42499999726879878, 141.7447067706911810, 9.630534252274376428 ) ) ;
#17615 = ORIENTED_EDGE ( 'NONE', *, *, #32268, .F. ) ;
#17614 = CARTESIAN_POINT ( 'NONE',  ( 10.01549611932653860, 210.2015048109876716, 25.85113791807856742 ) ) ;
#17616 = CARTESIAN_POINT ( 'NONE',  ( -59.30608239026425821, 194.9296489543815483, 2.372148111071822996 ) ) ;
#17617 = CARTESIAN_POINT ( 'NONE',  ( 88.27499999726880731, 160.0630714827496206, 15.58253174999999402 ) ) ;
#17618 = CARTESIAN_POINT ( 'NONE',  ( 7.456977232089302632, 217.1783343296989131, 97.55113791807858092 ) ) ;
#17619 = DIRECTION ( 'NONE',  ( -1.000000000000000000, -4.625929269271485914E-16, 0.000000000000000000 ) ) ;
#17620 = ORIENTED_EDGE ( 'NONE', *, *, #2897, .T. ) ;
#17621 = CARTESIAN_POINT ( 'NONE',  ( 10.01549611932659367, 203.7984951890124421, 82.14886208192143613 ) ) ;
#17622 = CARTESIAN_POINT ( 'NONE',  ( -7.375838497908014268, 196.7627149292498530, 17.04886208192143471 ) ) ;
#17623 = CARTESIAN_POINT ( 'NONE',  ( -6.500000000000000000, -3.752776749732573247, -0.8000000000000003775 ) ) ;
#17624 = CARTESIAN_POINT ( 'NONE',  ( -3.135527875058821579, 197.5041725223112223, 35.90113791807856813 ) ) ;
#17625 = CARTESIAN_POINT ( 'NONE',  ( 4.336808689942017736E-16, 8.660254037844390851, -1.000000000000000888 ) ) ;
#17626 = CARTESIAN_POINT ( 'NONE',  ( -6.220909254589682469, 215.4770327129946850, 98.94886208192140487 ) ) ;
#17627 = FACE_OUTER_BOUND ( 'NONE', #9316, .T. ) ;
#17628 = AXIS2_PLACEMENT_3D ( 'NONE', #28760, #26195, #7477 ) ;
#17629 = ORIENTED_EDGE ( 'NONE', *, *, #5018, .T. ) ;
#17630 = CARTESIAN_POINT ( 'NONE',  ( -4.515071337844649868, -29.14748715311448279, -16.91127448208918338 ) ) ;
#17631 = CARTESIAN_POINT ( 'NONE',  ( 8.015496119326595448, 204.4483345814782638, 76.14886208192143613 ) ) ;
#17632 = VECTOR ( 'NONE', #7337, 1000.000000000000000 ) ;
#17633 = ORIENTED_EDGE ( 'NONE', *, *, #5778, .T. ) ;
#17634 = DIRECTION ( 'NONE',  ( -1.000000000000000000, 0.000000000000000000, 0.000000000000000000 ) ) ;
#17635 = EDGE_LOOP ( 'NONE', ( #32241, #10560, #29688, #20438 ) ) ;
#17636 = FACE_OUTER_BOUND ( 'NONE', #7913, .T. ) ;
#17637 = EDGE_CURVE ( 'NONE', #29444, #21593, #18652, .T. ) ;
#17638 = CARTESIAN_POINT ( 'NONE',  ( 81.62499999726878741, 171.3844434931184253, -7.942151717890132712E-15 ) ) ;
#17639 = DIRECTION ( 'NONE',  ( -0.000000000000000000, -0.000000000000000000, 1.000000000000000000 ) ) ;
#17640 = CARTESIAN_POINT ( 'NONE',  ( -2.426778023690262742, 214.6231898156240163, 76.10113791807854966 ) ) ;
#17641 = DIRECTION ( 'NONE',  ( -1.000000000000000000, -0.000000000000000000, -0.000000000000000000 ) ) ;
#17642 = FILL_AREA_STYLE ('',( #20028 ) ) ;
#17643 = CARTESIAN_POINT ( 'NONE',  ( 41.50000000000000000, 155.0000000000000000, 14.49999999999999467 ) ) ;
#17644 = CARTESIAN_POINT ( 'NONE',  ( 0.05014649552828262524, 198.5883022060938572, 49.74886208192144466 ) ) ;
#17645 = EDGE_CURVE ( 'NONE', #21522, #22313, #30062, .T. ) ;
#17646 = LINE ( 'NONE', #30255, #2313 ) ;
#17647 = CARTESIAN_POINT ( 'NONE',  ( 78.48867513459484258, 142.2402378747194405, -9.270509831248439525 ) ) ;
#17648 = CARTESIAN_POINT ( 'NONE',  ( -129.1982509225904607, 3.226370279868306490, 35.00001200000000523 ) ) ;
#17649 = CARTESIAN_POINT ( 'NONE',  ( 60.52499999726881441, 140.1801316387863778, 4.815267126137185549 ) ) ;
#17650 = CARTESIAN_POINT ( 'NONE',  ( 63.27499999726881441, 149.9369285172503510, -15.58253175000000823 ) ) ;
#17651 = CARTESIAN_POINT ( 'NONE',  ( -3.662846001190052991, 218.4274158808045740, 61.10113791807857808 ) ) ;
#17652 = DIRECTION ( 'NONE',  ( 0.7071067811865474617, 8.659560562354932858E-17, 0.7071067811865474617 ) ) ;
#17653 = CARTESIAN_POINT ( 'NONE',  ( -11.98450388067348804, 210.9467285061362247, 12.65113791807856636 ) ) ;
#17654 = CARTESIAN_POINT ( 'NONE',  ( 10.01549611932653860, 210.2015048109876716, 76.85113791807857808 ) ) ;
#17655 = EDGE_CURVE ( 'NONE', #12301, #11757, #17848, .T. ) ;
#17656 = CARTESIAN_POINT ( 'NONE',  ( 7.456977232089471386, 196.8216656703012006, 40.44886208192144039 ) ) ;
#17657 = CARTESIAN_POINT ( 'NONE',  ( 3.044812012439969795, 216.5253028482143520, 60.39886208192143613 ) ) ;
#17658 = DIRECTION ( 'NONE',  ( 1.000000000000000000, 0.000000000000000000, 0.000000000000000000 ) ) ;
#17659 = CARTESIAN_POINT ( 'NONE',  ( -12.01549611932652972, 203.1486557965464499, 84.35113791807857808 ) ) ;
#17660 = DIRECTION ( 'NONE',  ( 0.000000000000000000, 0.000000000000000000, -1.000000000000000000 ) ) ;
#17661 = CARTESIAN_POINT ( 'NONE',  ( 9.984503880673470277, 203.7031108863295401, 8.151137918078564581 ) ) ;
#17662 = CARTESIAN_POINT ( 'NONE',  ( -9.984503880673420539, 203.7031108863293980, 68.34886208192143897 ) ) ;
#17663 = DIRECTION ( 'NONE',  ( 1.000000000000000000, -0.000000000000000000, -0.000000000000000000 ) ) ;
#17664 = EDGE_LOOP ( 'NONE', ( #4935, #24918, #15941 ) ) ;
#17665 = CARTESIAN_POINT ( 'NONE',  ( -7.456977232089471386, 217.1783343296987709, 68.94886208192144750 ) ) ;
#17666 = STYLED_ITEM ( 'NONE', ( #29079 ), #13278 ) ;
#17667 = VERTEX_POINT ( 'NONE', #22738 ) ;
#17668 = CARTESIAN_POINT ( 'NONE',  ( 79.07499999726880446, 141.7447067706911810, -9.630534252274385310 ) ) ;
#17669 = CARTESIAN_POINT ( 'NONE',  ( 0.05014649552828262524, 198.5883022060938572, 55.74886208192144466 ) ) ;
#17670 = EDGE_LOOP ( 'NONE', ( #6255, #11128, #819, #11716 ) ) ;
#17671 = EDGE_CURVE ( 'NONE', #19176, #8611, #7069, .T. ) ;
#17672 = CARTESIAN_POINT ( 'NONE',  ( 71.02499999726882152, 149.9369285172503510, -15.58253175000000823 ) ) ;
#17673 = DIRECTION ( 'NONE',  ( 0.000000000000000000, 0.000000000000000000, -1.000000000000000000 ) ) ;
#17674 = CARTESIAN_POINT ( 'NONE',  ( -60.00000000000000000, -7.347880794884118356E-15, 20.00000000000000000 ) ) ;
#17675 = EDGE_CURVE ( 'NONE', #5679, #8568, #13478, .T. ) ;
#17676 = CARTESIAN_POINT ( 'NONE',  ( 65.22499999726881015, 160.0630714827496206, -15.58253175000000823 ) ) ;
#17677 = CARTESIAN_POINT ( 'NONE',  ( -58.50000000000001421, -88.00000000000000000, -20.00000000000000000 ) ) ;
#17678 = CARTESIAN_POINT ( 'NONE',  ( 10.01549611932659545, 203.7984951890123853, 46.14886208192143613 ) ) ;
#17679 = EDGE_LOOP ( 'NONE', ( #29731, #21503, #26377, #14733 ) ) ;
#17680 = DIRECTION ( 'NONE',  ( 2.312964634635740985E-16, -1.000000000000000000, 0.000000000000000000 ) ) ;
#17681 = SURFACE_STYLE_FILL_AREA ( #24504 ) ;
#17682 = FACE_OUTER_BOUND ( 'NONE', #14678, .T. ) ;
#17683 = CARTESIAN_POINT ( 'NONE',  ( 5.000000000000000000, -4.685197434473814759, 3.903127820947815962E-15 ) ) ;
#17684 = CARTESIAN_POINT ( 'NONE',  ( -8.015496119326597224, 209.5516654185217362, 20.64886208192143613 ) ) ;
#17685 = CARTESIAN_POINT ( 'NONE',  ( -10.01549611932653860, 203.7984951890123284, 66.35113791807853545 ) ) ;
#17686 = DIRECTION ( 'NONE',  ( -0.5000000000000046629, -0.8660254037844359321, 0.000000000000000000 ) ) ;
#17687 = CARTESIAN_POINT ( 'NONE',  ( -8.118202686958039038, 201.1607312380087080, 51.20113791807857240 ) ) ;
#17688 = CONTEXT_DEPENDENT_SHAPE_REPRESENTATION ( #7048, #3838 ) ;
#17689 = CARTESIAN_POINT ( 'NONE',  ( 8.118202686958039038, 212.8392687619912635, 16.70113791807856529 ) ) ;
#17690 = CARTESIAN_POINT ( 'NONE',  ( -4.903702542908602524, 213.8346818373418898, 6.951137918078566180 ) ) ;
#17691 = CARTESIAN_POINT ( 'NONE',  ( -1.750000000000014211, 3.031088913245526317, -2.899999999999999911 ) ) ;
#17692 = CARTESIAN_POINT ( 'NONE',  ( 38.22499999726881015, 149.9369285172503510, 15.58253174999999580 ) ) ;
#17693 = CARTESIAN_POINT ( 'NONE',  ( 11.98450388067348271, 203.0532714938637753, 26.15113791807857169 ) ) ;
#17694 = FACE_BOUND ( 'NONE', #27295, .T. ) ;
#17695 = CARTESIAN_POINT ( 'NONE',  ( -6.220909254589537696, 198.5229672870051161, 72.05113791807853829 ) ) ;
#17696 = CARTESIAN_POINT ( 'NONE',  ( -0.05014649552810635652, 196.4853777576173002, 53.75113791807857666 ) ) ;
#17697 = CARTESIAN_POINT ( 'NONE',  ( 32.81249999863440792, 155.0000000000000000, -15.04126587500000767 ) ) ;
#17698 = DIRECTION ( 'NONE',  ( -0.9891821073486152249, -0.1466927349985424900, -2.962715634069391535E-17 ) ) ;
#17699 = CARTESIAN_POINT ( 'NONE',  ( -7.456977232089471386, 217.1783343296987709, 14.94886208192143506 ) ) ;
#17700 = CARTESIAN_POINT ( 'NONE',  ( -9.984503880673420539, 203.7031108863293980, 20.34886208192143187 ) ) ;
#17701 = CARTESIAN_POINT ( 'NONE',  ( 72.29999999453761461, 167.3344367211045096, -8.961492836873482304 ) ) ;
#17702 = VERTEX_POINT ( 'NONE', #23241 ) ;
#17703 = CARTESIAN_POINT ( 'NONE',  ( 7.375838497908181246, 196.7627149292499666, 56.45113791807857240 ) ) ;
#17704 = CARTESIAN_POINT ( 'NONE',  ( -2.517493886308901807, 199.4062855549015012, 74.90113791807856103 ) ) ;
#17705 = EDGE_CURVE ( 'NONE', #33308, #11477, #23006, .T. ) ;
#17706 = CARTESIAN_POINT ( 'NONE',  ( -8.062137200540822946, 201.0835637161416400, 44.19886208192143329 ) ) ;
#17707 = EDGE_CURVE ( 'NONE', #6813, #31166, #20517, .T. ) ;
#17708 = CARTESIAN_POINT ( 'NONE',  ( 92.60208470531341618, 155.0000000000000000, 0.000000000000000000 ) ) ;
#17709 = ORIENTED_EDGE ( 'NONE', *, *, #18490, .T. ) ;
#17710 = ORIENTED_EDGE ( 'NONE', *, *, #21435, .F. ) ;
#17711 = ORIENTED_EDGE ( 'NONE', *, *, #21633, .T. ) ;
#17712 = EDGE_CURVE ( 'NONE', #6185, #10719, #31415, .T. ) ;
#17713 = FACE_OUTER_BOUND ( 'NONE', #18231, .T. ) ;
#17714 = CARTESIAN_POINT ( 'NONE',  ( 0.5619217318086654478, 7.564468822943301696, -6.443866470201762731 ) ) ;
#17715 = EDGE_LOOP ( 'NONE', ( #8777, #13318 ) ) ;
#17716 =( BOUNDED_CURVE ( )  B_SPLINE_CURVE ( 2, ( #15834, #29116, #664, #13605, #6271, #3550, #27229, #24170, #21606, #8497, #8666 ),
 .UNSPECIFIED., .F., .T. ) 
 B_SPLINE_CURVE_WITH_KNOTS ( ( 3, 2, 2, 2, 2, 3 ),
 ( 0.7857142857142856984, 0.7892857142857142572, 0.7928571428571428159, 0.7964285714285713746, 0.7999999999999999334, 0.8035714285714284921 ),
 .UNSPECIFIED. ) 
 CURVE ( )  GEOMETRIC_REPRESENTATION_ITEM ( )  RATIONAL_B_SPLINE_CURVE ( ( 1.000000000000000000, 0.9510565162951534202, 1.000000000000000000, 0.9510565162951534202, 1.000000000000000000, 0.9510565162951534202, 1.000000000000000000, 0.9510565162951534202, 1.000000000000000000, 0.9510565162951534202, 1.000000000000000000 ) ) 
 REPRESENTATION_ITEM ( '' )  );
#17717 = CARTESIAN_POINT ( 'NONE',  ( 8.000000000000008882, 206.9523078486586485, 32.00113791807856956 ) ) ;
#17718 = EDGE_CURVE ( 'NONE', #739, #8613, #28360, .T. ) ;
#17719 = FACE_OUTER_BOUND ( 'NONE', #13662, .T. ) ;
#17720 = CARTESIAN_POINT ( 'NONE',  ( -8.062137200540822946, 201.0835637161416400, 11.19886208192143506 ) ) ;
#17721 = CARTESIAN_POINT ( 'NONE',  ( 56.97499999726881015, 140.1801316387863778, -4.815267126137194431 ) ) ;
#17722 = ORIENTED_EDGE ( 'NONE', *, *, #4731, .T. ) ;
#17723 = CARTESIAN_POINT ( 'NONE',  ( 6.500168698208129925, 211.6636982574063381, 55.70113791807857240 ) ) ;
#17724 = CARTESIAN_POINT ( 'NONE',  ( 56.78867513459481842, 155.0000000000000000, -15.00000000000002487 ) ) ;
#17725 =( LENGTH_UNIT ( ) NAMED_UNIT ( * ) SI_UNIT ( .MILLI., .METRE. ) );
#17726 = LINE ( 'NONE', #4773, #19530 ) ;
#17727 = CARTESIAN_POINT ( 'NONE',  ( 9.984503880673420539, 210.2968891136705167, 102.8488620819214390 ) ) ;
#17728 = CARTESIAN_POINT ( 'NONE',  ( 66.07499999726881867, 168.2552932293087906, 9.630534252274372875 ) ) ;
#17729 = CARTESIAN_POINT ( 'NONE',  ( -6.139770520408369237, 215.5359834540460042, 42.95113791807856529 ) ) ;
#17730 = CARTESIAN_POINT ( 'NONE',  ( -3.500000000000001332, 2.020725942163676070, -0.3126073911696459207 ) ) ;
#17731 = CARTESIAN_POINT ( 'NONE',  ( 9.984503880673470277, 203.7031108863295401, 17.15113791807856103 ) ) ;
#17732 = CARTESIAN_POINT ( 'NONE',  ( -6.139770520408224463, 198.4640165459539105, 101.0488620819214276 ) ) ;
#17733 = DIRECTION ( 'NONE',  ( 1.000000000000000000, 0.000000000000000000, 0.000000000000000000 ) ) ;
#17734 = CARTESIAN_POINT ( 'NONE',  ( 86.50000000000000000, 155.0000000000000000, -14.50000000000000711 ) ) ;
#17735 = CARTESIAN_POINT ( 'NONE',  ( 40.78867513459481842, 155.0000000000000000, -15.00000000000002487 ) ) ;
#17736 = CARTESIAN_POINT ( 'NONE',  ( -0.05014649552807705357, 194.3824533091408000, -0.2488620819214344970 ) ) ;
#17737 = DIRECTION ( 'NONE',  ( 1.000000000000000000, 0.000000000000000000, 0.000000000000000000 ) ) ;
#17738 = CARTESIAN_POINT ( 'NONE',  ( 53.97499999726881015, 169.8198683612136222, 4.815267126137181997 ) ) ;
#17739 = CARTESIAN_POINT ( 'NONE',  ( 6.220909254589536808, 215.4770327129947702, 49.55113791807855250 ) ) ;
#17740 = CYLINDRICAL_SURFACE ( 'NONE', #7240, 15.00000000000001776 ) ;
#17741 = CARTESIAN_POINT ( 'NONE',  ( -52.50000000000002132, 155.0000000000000000, 6.938893903907228378E-15 ) ) ;
#17742 = CARTESIAN_POINT ( 'NONE',  ( 64.91132485994280898, 146.1832212156128890, 12.13525491562421976 ) ) ;
#17743 = CARTESIAN_POINT ( 'NONE',  ( 55.29999999453762882, 142.6655632788954620, 8.961492836873471646 ) ) ;
#17744 = ORIENTED_EDGE ( 'NONE', *, *, #4518, .F. ) ;
#17745 = CARTESIAN_POINT ( 'NONE',  ( 3.753561863808689836, 218.3979405102790565, 31.40113791807856813 ) ) ;
#17746 = DIRECTION ( 'NONE',  ( 0.000000000000000000, -0.5000000000000013323, -0.8660254037844379305 ) ) ;
#17747 = CARTESIAN_POINT ( 'NONE',  ( 6.139770520408223575, 215.5359834540460611, 9.548862081921431155 ) ) ;
#17748 = DIRECTION ( 'NONE',  ( 1.000000000000000000, 0.000000000000000000, 0.000000000000000000 ) ) ;
#17749 = ORIENTED_EDGE ( 'NONE', *, *, #16187, .F. ) ;
#17750 = CARTESIAN_POINT ( 'NONE',  ( -3.044812012440131443, 216.5253028482142952, 10.10113791807856565 ) ) ;
#17751 = CARTESIAN_POINT ( 'NONE',  ( -10.00000000000000711, 207.0476921513413515, 57.50113791807856956 ) ) ;
#17752 = ORIENTED_EDGE ( 'NONE', *, *, #33099, .F. ) ;
#17753 = CARTESIAN_POINT ( 'NONE',  ( -4.903702542908436435, 200.1653181626580249, 23.04886208192143826 ) ) ;
#17754 = CARTESIAN_POINT ( 'NONE',  ( -54.30000000000002558, -88.00000000000000000, -20.00000000000000000 ) ) ;
#17755 = EDGE_LOOP ( 'NONE', ( #16324, #8367 ) ) ;
#17756 = CARTESIAN_POINT ( 'NONE',  ( 7.984503880673485376, 204.3529502787953902, 2.151137918078566802 ) ) ;
#17757 = CARTESIAN_POINT ( 'NONE',  ( 12.01549611932659367, 203.1486557965466773, 88.14886208192143613 ) ) ;
#17758 = CARTESIAN_POINT ( 'NONE',  ( 39.37499999726880873, 155.0000000000000000, -15.58253175000000823 ) ) ;
#17759 = ORIENTED_EDGE ( 'NONE', *, *, #12049, .T. ) ;
#17760 = CARTESIAN_POINT ( 'NONE',  ( 43.52499999726881441, 169.8198683612136222, -4.815267126137197984 ) ) ;
#17761 = CARTESIAN_POINT ( 'NONE',  ( 119.7500000000000000, 3.125910954823619074E-14, 35.00000599999999906 ) ) ;
#17762 = CARTESIAN_POINT ( 'NONE',  ( -3.135527875058821579, 197.5041725223112223, 2.901137918078565914 ) ) ;
#17763 = CLOSED_SHELL ( 'NONE', ( #8555, #11338, #33480, #21398, #30761, #31230, #11809, #24796, #19938, #9313, #24389, #24485, #27217, #23467, #21442, #13105, #1244, #23566, #14436, #31457, #9164, #8321, #8739, #28651, #5149, #29130, #1055 ) ) ;
#17764 = CARTESIAN_POINT ( 'NONE',  ( -10.01549611932659722, 210.2015048109875011, 68.64886208192143613 ) ) ;
#17765 = CARTESIAN_POINT ( 'NONE',  ( 47.87499999726880162, 171.3844434931184253, -7.942151717890132712E-15 ) ) ;
#17766 = CARTESIAN_POINT ( 'NONE',  ( -67.50001199999998391, 147.4664294917440373, -15.28016032735712848 ) ) ;
#17767 = CARTESIAN_POINT ( 'NONE',  ( 3.044812012440130555, 197.4746971517856764, 14.60113791807856565 ) ) ;
#17768 = DIRECTION ( 'NONE',  ( 1.000000000000000000, 0.000000000000000000, 0.000000000000000000 ) ) ;
#17769 = AXIS2_PLACEMENT_3D ( 'NONE', #9673, #30123, #7467 ) ;
#17770 = CARTESIAN_POINT ( 'NONE',  ( 69.29999999999999716, 163.5228861582408797, 11.73074641843673049 ) ) ;
#17771 = CARTESIAN_POINT ( 'NONE',  ( -6.220909254589537696, 198.5229672870051161, 87.05113791807856671 ) ) ;
#17772 = DIRECTION ( 'NONE',  ( 0.000000000000000000, 0.000000000000000000, -1.000000000000000000 ) ) ;
#17773 = CARTESIAN_POINT ( 'NONE',  ( 3.044812012440130555, 197.4746971517856764, 77.60113791807857808 ) ) ;
#17774 = CARTESIAN_POINT ( 'NONE',  ( -1.249327701954873415, 8.410337540189265937, -7.776713651267812999 ) ) ;
#17775 = CARTESIAN_POINT ( 'NONE',  ( 34.49999999999997868, 7.979727989493303168E-15, 30.00000000000000000 ) ) ;
#17776 = CARTESIAN_POINT ( 'NONE',  ( 0.05014649552828288198, 194.3824533091408000, 91.74886208192144466 ) ) ;
#17777 = CARTESIAN_POINT ( 'NONE',  ( 63.12499999726880873, 155.0000000000000000, -15.58253175000000823 ) ) ;
#17779 = ORIENTED_EDGE ( 'NONE', *, *, #235, .T. ) ;
#17778 = CARTESIAN_POINT ( 'NONE',  ( -6.139770520408368348, 215.5359834540460042, 27.95113791807856529 ) ) ;
#17780 = CARTESIAN_POINT ( 'NONE',  ( -60.91988776943159678, 194.9950600780878460, 0.6490123436103525378 ) ) ;
#17781 = CARTESIAN_POINT ( 'NONE',  ( 88.17499999726881299, 164.1591823560292198, 12.60653300113718167 ) ) ;
#17782 = CARTESIAN_POINT ( 'NONE',  ( 7.375838497908181246, 196.7627149292499666, 92.45113791807857240 ) ) ;
#17783 = DIRECTION ( 'NONE',  ( -0.000000000000000000, -0.000000000000000000, 1.000000000000000000 ) ) ;
#17784 = CIRCLE ( 'NONE', #31921, 4.171999999999999709 ) ;
#17785 = ORIENTED_EDGE ( 'NONE', *, *, #25206, .T. ) ;
#17786 = VECTOR ( 'NONE', #21271, 1000.000000000000000 ) ;
#17787 = CARTESIAN_POINT ( 'NONE',  ( -3.044812012439970683, 197.4746971517856196, 85.89886208192143613 ) ) ;
#17788 = CARTESIAN_POINT ( 'NONE',  ( -11.98450388067341876, 203.0532714938636047, 23.34886208192143542 ) ) ;
#17789 = CARTESIAN_POINT ( 'NONE',  ( 11.41286821541922336, -25.16504226903143859, -0.07154745401829853968 ) ) ;
#17790 = CARTESIAN_POINT ( 'NONE',  ( -6.139770520408369237, 215.5359834540460042, 33.95113791807855108 ) ) ;
#17791 = ORIENTED_EDGE ( 'NONE', *, *, #24726, .F. ) ;
#17792 = CARTESIAN_POINT ( 'NONE',  ( 3.044812012439969795, 216.5253028482143520, 102.3988620819214361 ) ) ;
#17793 = AXIS2_PLACEMENT_3D ( 'NONE', #5200, #23433, #3145 ) ;
#17794 = CARTESIAN_POINT ( 'NONE',  ( 10.40000000000000036, 0.000000000000000000, 5.000000000000001776 ) ) ;
#17795 = ORIENTED_EDGE ( 'NONE', *, *, #17276, .T. ) ;
#17796 = DIRECTION ( 'NONE',  ( 1.000000000000000000, 0.000000000000000000, 0.000000000000000000 ) ) ;
#17797 = CARTESIAN_POINT ( 'NONE',  ( 6.444103211790928043, 211.7408657792734061, 84.69886208192144750 ) ) ;
#17798 = ORIENTED_EDGE ( 'NONE', *, *, #20196, .F. ) ;
#17799 = EDGE_CURVE ( 'NONE', #22995, #24364, #6659, .T. ) ;
#17800 = CARTESIAN_POINT ( 'NONE',  ( 34.50000000000000000, -103.0000000000000142, -30.00000000000000000 ) ) ;
#17801 = ORIENTED_EDGE ( 'NONE', *, *, #7454, .F. ) ;
#17802 = FACE_OUTER_BOUND ( 'NONE', #19208, .T. ) ;
#17803 = CARTESIAN_POINT ( 'NONE',  ( -8.000000000000008882, 207.0476921513413515, 60.50113791807857666 ) ) ;
#17804 = CIRCLE ( 'NONE', #22145, 3.499999999999999556 ) ;
#17805 = CARTESIAN_POINT ( 'NONE',  ( 83.82499999726880446, 168.2552932293087906, 9.630534252274372875 ) ) ;
#17806 = DIRECTION ( 'NONE',  ( -1.000000000000000000, 0.000000000000000000, 0.000000000000000000 ) ) ;
#17807 = CARTESIAN_POINT ( 'NONE',  ( 0.05014649552807626948, 215.4116977939061144, 79.25113791807856956 ) ) ;
#17808 = DIRECTION ( 'NONE',  ( 1.804112415015879625E-16, -1.000000000000000000, 0.000000000000000000 ) ) ;
#17809 = CIRCLE ( 'NONE', #31947, 15.00000000000001776 ) ;
#17810 = CARTESIAN_POINT ( 'NONE',  ( 45.10000000000000142, 168.7903194862797420, 4.480746418436729606 ) ) ;
#17811 = CARTESIAN_POINT ( 'NONE',  ( 0.05014649552828262524, 198.5883022060938572, 67.74886208192143044 ) ) ;
#17812 = CARTESIAN_POINT ( 'NONE',  ( -10.01549611932653860, 203.7984951890123000, 3.351137918078566091 ) ) ;
#17813 = CARTESIAN_POINT ( 'NONE',  ( -1.250000000000000444, 7.938566201357357244, -7.198902722707429369 ) ) ;
#17814 = CYLINDRICAL_SURFACE ( 'NONE', #16419, 5.000000000000001776 ) ;
#17815 = CARTESIAN_POINT ( 'NONE',  ( 54.42499999726881299, 141.7447067706911810, 9.630534252274376428 ) ) ;
#17816 = CARTESIAN_POINT ( 'NONE',  ( 71.47499999726879594, 160.0630714827496206, -15.58253175000000823 ) ) ;
#17817 = CARTESIAN_POINT ( 'NONE',  ( 9.736236675707914401, 214.0148392665762458, 70.70113791807857240 ) ) ;
#17818 = CARTESIAN_POINT ( 'NONE',  ( 9.680171189290831535, 199.9079932115568852, 11.30113791807856671 ) ) ;
#17819 = CARTESIAN_POINT ( 'NONE',  ( -10.01549611932653860, 203.7984951890123000, 84.35113791807856387 ) ) ;
#17820 = CARTESIAN_POINT ( 'NONE',  ( 9.680171189290716072, 214.0920067884432854, 51.69886208192144039 ) ) ;
#17821 = CARTESIAN_POINT ( 'NONE',  ( -8.062137200540822946, 201.0835637161416400, 62.19886208192143329 ) ) ;
#17822 = DIRECTION ( 'NONE',  ( 0.000000000000000000, 0.000000000000000000, -1.000000000000000000 ) ) ;
#17823 = CARTESIAN_POINT ( 'NONE',  ( 7.375838497908181246, 196.7627149292499666, 98.45113791807858661 ) ) ;
#17824 = CARTESIAN_POINT ( 'NONE',  ( 83.61132485994282604, 150.1262045565064227, -15.00000000000002665 ) ) ;
#17825 = CARTESIAN_POINT ( 'NONE',  ( -8.118202686958039038, 201.1607312380087080, 0.2011379180785657361 ) ) ;
#17826 = CARTESIAN_POINT ( 'NONE',  ( -8.118202686958138514, 212.8392687619910930, 65.79886208192144181 ) ) ;
#17827 = CIRCLE ( 'NONE', #14030, 3.500000000000000444 ) ;
#17828 = DIRECTION ( 'NONE',  ( -0.000000000000000000, -0.000000000000000000, 1.000000000000000000 ) ) ;
#17829 = ORIENTED_EDGE ( 'NONE', *, *, #18686, .F. ) ;
#17830 = CARTESIAN_POINT ( 'NONE',  ( 7.375838497908012492, 217.2372850707501186, 72.54886208192141339 ) ) ;
#17831 = CIRCLE ( 'NONE', #24371, 2.149999999999999023 ) ;
#17832 = CARTESIAN_POINT ( 'NONE',  ( -8.062137200540920645, 212.9164362838581894, 93.80113791807858092 ) ) ;
#17833 = VERTEX_POINT ( 'NONE', #7583 ) ;
#17834 = CARTESIAN_POINT ( 'NONE',  ( 78.07499999726880446, 168.2552932293087906, 9.630534252274372875 ) ) ;
#17835 = CARTESIAN_POINT ( 'NONE',  ( -4.903702542908436435, 200.1653181626580249, 53.04886208192144181 ) ) ;
#17836 = VERTEX_POINT ( 'NONE', #2967 ) ;
#17837 = EDGE_CURVE ( 'NONE', #7110, #13563, #19713, .T. ) ;
#17838 = AXIS2_PLACEMENT_3D ( 'NONE', #7861, #5461, #13128 ) ;
#17839 = CARTESIAN_POINT ( 'NONE',  ( 72.02499999726882152, 160.0630714827496206, 15.58253174999999224 ) ) ;
#17840 = CARTESIAN_POINT ( 'NONE',  ( 6.500000000000000888, 2.679956093905413450, -6.238387772031967593 ) ) ;
#17841 = CARTESIAN_POINT ( 'NONE',  ( -58.16962743627800592, 194.9217985566782829, 2.500000000000000000 ) ) ;
#17842 = EDGE_CURVE ( 'NONE', #25762, #23772, #2293, .T. ) ;
#17843 = CARTESIAN_POINT ( 'NONE',  ( 66.22499999726879594, 149.9369285172503510, 15.58253174999999580 ) ) ;
#17844 = CARTESIAN_POINT ( 'NONE',  ( -7.499999999999999112, 4.651022038490018495, -7.928862870699868282 ) ) ;
#17845 = CARTESIAN_POINT ( 'NONE',  ( 8.062137200540822946, 212.9164362838583315, 54.69886208192143329 ) ) ;
#17846 = ORIENTED_EDGE ( 'NONE', *, *, #25206, .F. ) ;
#17847 = CYLINDRICAL_SURFACE ( 'NONE', #29790, 2.428571428571428381 ) ;
#17848 = B_SPLINE_CURVE_WITH_KNOTS ( 'NONE', 3,
 ( #14556, #12342, #1774, #27502, #4338, #20008, #12175, #30408 ),
 .UNSPECIFIED., .F., .F.,
 ( 4, 2, 2, 4 ),
 ( 0.02832689070575898985, 0.03234239231761927569, 0.03635789392947955806, 0.04438889715320012280 ),
 .UNSPECIFIED. ) ;
#17849 = EDGE_CURVE ( 'NONE', #25762, #14984, #30650, .T. ) ;
#17850 =( NAMED_UNIT ( * ) PLANE_ANGLE_UNIT ( ) SI_UNIT ( $, .RADIAN. ) );
#17851 = CARTESIAN_POINT ( 'NONE',  ( 5.589124336234546853, -4.278671059401403021, -6.219623095963592974 ) ) ;
#17852 = DIRECTION ( 'NONE',  ( 1.000000000000000000, 0.000000000000000000, 0.000000000000000000 ) ) ;
#17853 = CARTESIAN_POINT ( 'NONE',  ( -0.05014649552828365914, 215.4116977939061144, 21.24886208192143755 ) ) ;
#17854 = AXIS2_PLACEMENT_3D ( 'NONE', #1582, #19305, #9076 ) ;
#17855 = CARTESIAN_POINT ( 'NONE',  ( -10.01549611932653860, 203.7984951890123284, 69.35113791807857808 ) ) ;
#17856 = LINE ( 'NONE', #25715, #13647 ) ;
#17857 = CARTESIAN_POINT ( 'NONE',  ( -3.044812012440131443, 216.5253028482142952, 52.10113791807857808 ) ) ;
#17858 = CONICAL_SURFACE ( 'NONE', #21137, 5.000000000000001776, 0.9599310885968795892 ) ;
#17859 = CARTESIAN_POINT ( 'NONE',  ( 6.139770520408368348, 198.4640165459539674, 26.45113791807856884 ) ) ;
#17860 = CARTESIAN_POINT ( 'NONE',  ( -0.05014649552807731031, 198.5883022060938572, 5.751137918078564226 ) ) ;
#17861 = DIRECTION ( 'NONE',  ( 1.000000000000000000, -0.000000000000000000, -0.000000000000000000 ) ) ;
#17862 = FACE_BOUND ( 'NONE', #26246, .T. ) ;
#17863 = CARTESIAN_POINT ( 'NONE',  ( 38.82499999726881157, 141.7447067706911810, -9.630534252274387086 ) ) ;
#17864 = CARTESIAN_POINT ( 'NONE',  ( -12.00000000000000711, 207.0476921513413515, 36.50113791807857666 ) ) ;
#17865 = CARTESIAN_POINT ( 'NONE',  ( 5.000000000000000000, -3.513898075855358183, 2.028750000000003606 ) ) ;
#17866 = ADVANCED_FACE ( 'NONE', ( #10805 ), #18677, .T. ) ;
#17867 =( BOUNDED_CURVE ( )  B_SPLINE_CURVE ( 2, ( #6179, #27138, #19131, #6525, #27301, #5842, #24073, #19637, #16904, #3623, #24238 ),
 .UNSPECIFIED., .F., .T. ) 
 B_SPLINE_CURVE_WITH_KNOTS ( ( 3, 2, 2, 2, 2, 3 ),
 ( 0.1428571428571427104, 0.1464285714285713247, 0.1499999999999999112, 0.1535714285714285254, 0.1571428571428572230, 0.1607142857142858372 ),
 .UNSPECIFIED. ) 
 CURVE ( )  GEOMETRIC_REPRESENTATION_ITEM ( )  RATIONAL_B_SPLINE_CURVE ( ( 1.000000000000001110, 0.9510565162951523099, 1.000000000000000000, 0.9510565162951534202, 1.000000000000000000, 0.9510565162951534202, 1.000000000000000000, 0.9510565162951534202, 1.000000000000000000, 0.9510565162951515328, 1.000000000000001998 ) ) 
 REPRESENTATION_ITEM ( '' )  );
#17868 = CARTESIAN_POINT ( 'NONE',  ( 6.220909254589536808, 215.4770327129947702, 82.55113791807858092 ) ) ;
#17869 = CARTESIAN_POINT ( 'NONE',  ( -10.01549611932653860, 203.7984951890123000, 51.35113791807857808 ) ) ;
#17870 = AXIS2_PLACEMENT_3D ( 'NONE', #27529, #4536, #17314 ) ;
#17871 = LINE ( 'NONE', #17697, #30114 ) ;
#17872 = CARTESIAN_POINT ( 'NONE',  ( 0.05014649552828288198, 194.3824533091408000, 16.74886208192143755 ) ) ;
#17873 = CARTESIAN_POINT ( 'NONE',  ( 6.139770520408223575, 215.5359834540460611, 30.54886208192143826 ) ) ;
#17874 = CARTESIAN_POINT ( 'NONE',  ( 72.89999999453765156, 159.7113355953771077, 14.49999999999999289 ) ) ;
#17875 = ORIENTED_EDGE ( 'NONE', *, *, #11183, .F. ) ;
#17876 = CARTESIAN_POINT ( 'NONE',  ( 0.05014649552807549926, 219.6175466908591716, 58.25113791807856245 ) ) ;
#17877 = CARTESIAN_POINT ( 'NONE',  ( 6.444103211791042618, 202.2591342207267644, 83.30113791807858092 ) ) ;
#17878 = EDGE_CURVE ( 'NONE', #28851, #2085, #2894, .T. ) ;
#17879 = CARTESIAN_POINT ( 'NONE',  ( -0.05014649552828403384, 217.5146222423826714, 42.24886208192143755 ) ) ;
#17880 = CARTESIAN_POINT ( 'NONE',  ( 75.41132485994282320, 142.2402378747194405, -9.270509831248439525 ) ) ;
#17881 = VERTEX_POINT ( 'NONE', #26295 ) ;
#17882 = CARTESIAN_POINT ( 'NONE',  ( 12.01549611932659367, 203.1486557965466773, 46.14886208192143613 ) ) ;
#17883 = ORIENTED_EDGE ( 'NONE', *, *, #24979, .F. ) ;
#17884 = CIRCLE ( 'NONE', #8093, 12.00000000000001066 ) ;
#17885 = ORIENTED_EDGE ( 'NONE', *, *, #31076, .F. ) ;
#17886 = PRODUCT ( 'air chamber shell rear', 'air chamber shell rear', '', ( #670 ) ) ;
#17887 = CYLINDRICAL_SURFACE ( 'NONE', #22204, 12.10452846326763598 ) ;
#17888 = CIRCLE ( 'NONE', #3187, 30.00000000000000000 ) ;
#17889 = DIRECTION ( 'NONE',  ( -0.000000000000000000, -0.000000000000000000, -1.000000000000000000 ) ) ;
#17890 = EDGE_LOOP ( 'NONE', ( #3402, #24944, #14651, #17447 ) ) ;
#17891 = CARTESIAN_POINT ( 'NONE',  ( 8.015496119326531499, 209.5516654185219636, 37.85113791807857098 ) ) ;
#17892 = CARTESIAN_POINT ( 'NONE',  ( 103.3032345859876102, 155.0000000000000000, 0.000000000000000000 ) ) ;
#17893 = CARTESIAN_POINT ( 'NONE',  ( -0.05014649552828403384, 217.5146222423826714, 24.24886208192143044 ) ) ;
#17894 = CARTESIAN_POINT ( 'NONE',  ( 54.07499999726880446, 168.2552932293087906, 9.630534252274372875 ) ) ;
#17895 = VERTEX_POINT ( 'NONE', #31088 ) ;
#17896 = CARTESIAN_POINT ( 'NONE',  ( 4.984841277089725686, 213.7757310962907411, 61.55113791807858092 ) ) ;
#17897 = CARTESIAN_POINT ( 'NONE',  ( -64.50000000000000000, -95.00000000000000000, 270.4495957273638282 ) ) ;
#17898 =( LENGTH_UNIT ( ) NAMED_UNIT ( * ) SI_UNIT ( .MILLI., .METRE. ) );
#17899 = CARTESIAN_POINT ( 'NONE',  ( -3.280815508853482498, -7.221948645665452915, -7.591546097228404122 ) ) ;
#17900 = CARTESIAN_POINT ( 'NONE',  ( 6.220909254589681581, 198.5229672870052582, 103.4488620819214049 ) ) ;
#17901 = CARTESIAN_POINT ( 'NONE',  ( 63.27499999726881441, 149.9369285172503510, -15.58253175000000823 ) ) ;
#17902 = CARTESIAN_POINT ( 'NONE',  ( -0.05014649552810635652, 196.4853777576173002, 41.75113791807855534 ) ) ;
#17903 =( LENGTH_UNIT ( ) NAMED_UNIT ( * ) SI_UNIT ( .MILLI., .METRE. ) );
#17904 = EDGE_CURVE ( 'NONE', #1328, #29866, #13345, .T. ) ;
#17905 = CARTESIAN_POINT ( 'NONE',  ( -10.00000000000000711, 207.0476921513413515, 30.50113791807856600 ) ) ;
#17906 = CARTESIAN_POINT ( 'NONE',  ( 6.139770520408223575, 215.5359834540460611, 99.54886208192144181 ) ) ;
#17907 = APPLICATION_PROTOCOL_DEFINITION ( 'draft international standard', 'automotive_design', 1998, #21167 ) ;
#17908 = CARTESIAN_POINT ( 'NONE',  ( 2.426778023690075337, 214.6231898156240447, 87.39886208192143613 ) ) ;
#17909 = CARTESIAN_POINT ( 'NONE',  ( 84.30000000000001137, 146.4771138417591203, -11.73074641843674470 ) ) ;
#17910 = CARTESIAN_POINT ( 'NONE',  ( 81.48867513459484258, 167.7597621252805880, 9.270509831248428867 ) ) ;
#17911 = CYLINDRICAL_SURFACE ( 'NONE', #17446, 15.00000000000001776 ) ;
#17912 = CARTESIAN_POINT ( 'NONE',  ( -9.680171189290831535, 214.0920067884431148, 3.801137918078565825 ) ) ;
#17913 = AXIS2_PLACEMENT_3D ( 'NONE', #28557, #12536, #2318 ) ;
#17914 = CARTESIAN_POINT ( 'NONE',  ( -0.2779000157839473517, -8.820699686765063774, -7.928862157988305626 ) ) ;
#17915 = CARTESIAN_POINT ( 'NONE',  ( 50.67499999726880588, 141.7447067706911810, 9.630534252274376428 ) ) ;
#17916 = EDGE_CURVE ( 'NONE', #21928, #10681, #7406, .T. ) ;
#17917 = CARTESIAN_POINT ( 'NONE',  ( 3.135527875058820690, 216.4958274776887492, 55.40113791807857524 ) ) ;
#17918 = CARTESIAN_POINT ( 'NONE',  ( 87.22499999726881015, 160.0630714827496206, -15.58253175000000823 ) ) ;
#17919 = VECTOR ( 'NONE', #22324, 1000.000000000000000 ) ;
#17920 = CARTESIAN_POINT ( 'NONE',  ( 90.49452189536829394, 155.0000000000000000, 32.10452846326766974 ) ) ;
#17921 = CARTESIAN_POINT ( 'NONE',  ( 40.02499999726881441, 160.0630714827496206, 15.58253174999999224 ) ) ;
#17922 = CARTESIAN_POINT ( 'NONE',  ( -6.220909254589682469, 215.4770327129947134, 2.948862081921434619 ) ) ;
#17923 = CARTESIAN_POINT ( 'NONE',  ( 56.19999999453763451, 163.5228861582408797, -11.73074641843674470 ) ) ;
#17924 = ORIENTED_EDGE ( 'NONE', *, *, #12703, .T. ) ;
#17925 = CARTESIAN_POINT ( 'NONE',  ( 7.375838497908181246, 196.7627149292499666, 26.45113791807857240 ) ) ;
#17926 = EDGE_CURVE ( 'NONE', #31055, #33588, #21947, .T. ) ;
#17927 = CARTESIAN_POINT ( 'NONE',  ( -0.05014649552828403384, 217.5146222423826714, 15.24886208192143044 ) ) ;
#17928 = VECTOR ( 'NONE', #27312, 1000.000000000000000 ) ;
#17929 = CYLINDRICAL_SURFACE ( 'NONE', #30830, 2.149999999999999023 ) ;
#17930 = VERTEX_POINT ( 'NONE', #13021 ) ;
#17931 =( BOUNDED_CURVE ( )  B_SPLINE_CURVE ( 2, ( #9254, #32926, #20148, #22878, #17425, #30546, #19979, #9766, #30380, #14865, #14697 ),
 .UNSPECIFIED., .F., .T. ) 
 B_SPLINE_CURVE_WITH_KNOTS ( ( 3, 2, 2, 2, 2, 3 ),
 ( 0.3571428571428570398, 0.3607142857142855985, 0.3642857142857141572, 0.3678571428571427715, 0.3714285714285713302, 0.3749999999999998890 ),
 .UNSPECIFIED. ) 
 CURVE ( )  GEOMETRIC_REPRESENTATION_ITEM ( )  RATIONAL_B_SPLINE_CURVE ( ( 1.000000000000001554, 0.9510565162951518658, 1.000000000000000000, 0.9510565162951534202, 1.000000000000000000, 0.9510565162951534202, 1.000000000000000000, 0.9510565162951534202, 1.000000000000000000, 0.9510565162951549745, 0.9999999999999984457 ) ) 
 REPRESENTATION_ITEM ( '' )  );
#17932 = CARTESIAN_POINT ( 'NONE',  ( -0.05014649552810635652, 196.4853777576173002, 11.75113791807856778 ) ) ;
#17933 = CARTESIAN_POINT ( 'NONE',  ( 3.044812012440130555, 197.4746971517856764, 71.60113791807857808 ) ) ;
#17934 = ORIENTED_EDGE ( 'NONE', *, *, #32890, .F. ) ;
#17935 = CARTESIAN_POINT ( 'NONE',  ( -8.015496119326597224, 209.5516654185217362, 29.64886208192143968 ) ) ;
#17936 = CARTESIAN_POINT ( 'NONE',  ( 79.78867513459482552, 155.0000000000000000, 15.00000000000001243 ) ) ;
#17937 = ORIENTED_EDGE ( 'NONE', *, *, #20489, .F. ) ;
#17938 = CARTESIAN_POINT ( 'NONE',  ( 4.984841277089725686, 213.7757310962907411, 4.551137918078565825 ) ) ;
#17939 = AXIS2_PLACEMENT_3D ( 'NONE', #10091, #27961, #1903 ) ;
#17940 = CARTESIAN_POINT ( 'NONE',  ( 12.00000000000000711, 207.0476921513415220, 87.99886208192144466 ) ) ;
#17941 = CARTESIAN_POINT ( 'NONE',  ( 39.87499999726879452, 171.3844434931184253, -7.942151717890134290E-15 ) ) ;
#17942 = ORIENTED_EDGE ( 'NONE', *, *, #1615, .T. ) ;
#17943 = CARTESIAN_POINT ( 'NONE',  ( 41.72499999726881015, 169.8198683612136222, 4.815267126137181997 ) ) ;
#17944 = CARTESIAN_POINT ( 'NONE',  ( 119.7499999999999858, 0.6872233929727994406, 35.00001200000000523 ) ) ;
#17945 = CARTESIAN_POINT ( 'NONE',  ( 0.05014649552810505201, 217.5146222423826714, 4.251137918078566003 ) ) ;
#17946 = CARTESIAN_POINT ( 'NONE',  ( -6.220909254589682469, 215.4770327129946850, 74.94886208192143329 ) ) ;
#17947 = CARTESIAN_POINT ( 'NONE',  ( 48.07499999726881867, 168.2552932293087906, 9.630534252274372875 ) ) ;
#17948 = CARTESIAN_POINT ( 'NONE',  ( -67.50001199999999812, 152.7747327161067403, -16.89041650604970002 ) ) ;
#17949 = CARTESIAN_POINT ( 'NONE',  ( 8.118202686958039038, 212.8392687619912635, 10.70113791807856529 ) ) ;
#17950 = CARTESIAN_POINT ( 'NONE',  ( 127.5000000000000000, 155.0000000000000000, 100.0000000000000000 ) ) ;
#17951 = EDGE_CURVE ( 'NONE', #30420, #33036, #20307, .T. ) ;
#17952 = CARTESIAN_POINT ( 'NONE',  ( 68.29999999999999716, 146.4771138417591203, -11.73074641843674470 ) ) ;
#17953 = CARTESIAN_POINT ( 'NONE',  ( 3.135527875058820690, 216.4958274776887492, 100.4011379180785752 ) ) ;
#17954 = CARTESIAN_POINT ( 'NONE',  ( 4.000000000000000000, 1.759474945355380404, -3.047500000000001652 ) ) ;
#17955 = CARTESIAN_POINT ( 'NONE',  ( -9.984503880673473830, 210.2968891136704315, 72.65113791807857524 ) ) ;
#17956 = CARTESIAN_POINT ( 'NONE',  ( 57.58867513459482979, 163.8167787843871110, 12.13525491562421621 ) ) ;
#17957 = CARTESIAN_POINT ( 'NONE',  ( 27.50000000000001066, 2.688867821578068806, -0.05704280876260246769 ) ) ;
#17958 = EDGE_CURVE ( 'NONE', #12741, #23132, #10165, .T. ) ;
#17959 = CARTESIAN_POINT ( 'NONE',  ( -3.662846001189865142, 195.5725841191952838, 82.89886208192143613 ) ) ;
#17960 = CARTESIAN_POINT ( 'NONE',  ( 72.02499999726882152, 160.0630714827496206, 15.58253174999999402 ) ) ;
#17961 = ORIENTED_EDGE ( 'NONE', *, *, #14161, .T. ) ;
#17962 = CARTESIAN_POINT ( 'NONE',  ( -60.74744875717816939, 194.9849611312037041, -1.107162489773501513 ) ) ;
#17963 = CARTESIAN_POINT ( 'NONE',  ( 34.59999999453763309, 168.7903194862797420, 4.480746418436729606 ) ) ;
#17964 = CARTESIAN_POINT ( 'NONE',  ( -0.05014649552807705357, 194.3824533091408000, 95.75113791807856956 ) ) ;
#17965 = DIRECTION ( 'NONE',  ( 0.000000000000000000, 0.000000000000000000, 1.000000000000000000 ) ) ;
#17966 = ORIENTED_EDGE ( 'NONE', *, *, #18983, .T. ) ;
#17967 = CARTESIAN_POINT ( 'NONE',  ( 8.062137200540822946, 212.9164362838583315, 87.69886208192144750 ) ) ;
#17968 = CARTESIAN_POINT ( 'NONE',  ( 7.375838497908012492, 217.2372850707501186, 27.54886208192144181 ) ) ;
#17969 = CARTESIAN_POINT ( 'NONE',  ( 7.940546747334011890, -27.16978800334334920, -0.4491195576436878278 ) ) ;
#17970 = CARTESIAN_POINT ( 'NONE',  ( 3.135527875058820690, 216.4958274776887492, 43.40113791807856813 ) ) ;
#17971 = ORIENTED_EDGE ( 'NONE', *, *, #21749, .F. ) ;
#17972 = CARTESIAN_POINT ( 'NONE',  ( 8.062137200540822946, 212.9164362838583315, 102.6988620819214475 ) ) ;
#17973 = CARTESIAN_POINT ( 'NONE',  ( 4.444974277457895973, 4.939246403833855936, -5.720331885005371042 ) ) ;
#17974 = EDGE_LOOP ( 'NONE', ( #20146, #24747 ) ) ;
#17975 = CARTESIAN_POINT ( 'NONE',  ( 2.426778023690075337, 214.6231898156240447, 84.39886208192143613 ) ) ;
#17976 = VERTEX_POINT ( 'NONE', #32074 ) ;
#17977 = CARTESIAN_POINT ( 'NONE',  ( 34.51132485994281041, 163.8167787843871110, 12.13525491562421621 ) ) ;
#17978 = ORIENTED_EDGE ( 'NONE', *, *, #18891, .T. ) ;
#17979 = CARTESIAN_POINT ( 'NONE',  ( 115.4999999999999858, 207.9999999999998010, -93.94869280115065635 ) ) ;
#17980 = CARTESIAN_POINT ( 'NONE',  ( -4.903702542908602524, 213.8346818373418898, 63.95113791807857240 ) ) ;
#17981 = CARTESIAN_POINT ( 'NONE',  ( 83.32499999726880446, 164.1591823560292198, -12.60653300113719766 ) ) ;
#17982 = CARTESIAN_POINT ( 'NONE',  ( 4.000000000000000000, -3.518949890710769246, 3.686287386450715076E-15 ) ) ;
#17983 = CARTESIAN_POINT ( 'NONE',  ( 0.05014649552807626948, 215.4116977939061144, 85.25113791807856956 ) ) ;
#17984 = CARTESIAN_POINT ( 'NONE',  ( 92.60208470531341618, 155.0000000000000000, 0.000000000000000000 ) ) ;
#17985 = SURFACE_STYLE_USAGE ( .BOTH. , #28207 ) ;
#17986 = CARTESIAN_POINT ( 'NONE',  ( 48.89999999999999858, 168.7903194862797420, -4.480746418436745593 ) ) ;
#17987 = CARTESIAN_POINT ( 'NONE',  ( 6.500168698208244500, 202.3363017425938324, 61.29886208192144892 ) ) ;
#17988 = CARTESIAN_POINT ( 'NONE',  ( 67.48867513459484258, 167.7597621252805880, 9.270509831248428867 ) ) ;
#17989 = EDGE_CURVE ( 'NONE', #25974, #5826, #26795, .T. ) ;
#17990 = DIRECTION ( 'NONE',  ( 1.000000000000000000, -0.000000000000000000, -0.000000000000000000 ) ) ;
#17991 = CARTESIAN_POINT ( 'NONE',  ( 13.75000000000002487, 23.81569860407205397, -18.00000000000000000 ) ) ;
#17992 = AXIS2_PLACEMENT_3D ( 'NONE', #26548, #18731, #5764 ) ;
#17993 = CARTESIAN_POINT ( 'NONE',  ( 27.50000000000000711, 10.70896984529284524, -16.90208611084169732 ) ) ;
#17994 = CARTESIAN_POINT ( 'NONE',  ( 55.62499999726881583, 171.3844434931184253, -7.942151717890134290E-15 ) ) ;
#17995 = CARTESIAN_POINT ( 'NONE',  ( 69.07499999726881867, 141.7447067706911810, -9.630534252274385310 ) ) ;
#17996 = CARTESIAN_POINT ( 'NONE',  ( -3.662846001190052991, 218.4274158808045740, 70.10113791807857808 ) ) ;
#17997 = CARTESIAN_POINT ( 'NONE',  ( 10.00000000000000888, 206.9523078486588474, -0.9988620819213797075 ) ) ;
#17998 = CARTESIAN_POINT ( 'NONE',  ( 11.98450388067348271, 203.0532714938637753, 14.15113791807856991 ) ) ;
#17999 = CARTESIAN_POINT ( 'NONE',  ( 10.00000000000000711, 206.9523078486586201, 86.00113791807858377 ) ) ;
#18000 = CARTESIAN_POINT ( 'NONE',  ( -12.00000000000000711, 206.9523078486584780, 56.49886208192144466 ) ) ;
#18001 = CARTESIAN_POINT ( 'NONE',  ( 3.044812012439969795, 216.5253028482143520, 54.39886208192143613 ) ) ;
#18002 = DIRECTION ( 'NONE',  ( 0.000000000000000000, -0.000000000000000000, 1.000000000000000000 ) ) ;
#18003 = CARTESIAN_POINT ( 'NONE',  ( 7.375838497908181246, 196.7627149292499666, 92.45113791807857240 ) ) ;
#18004 = CARTESIAN_POINT ( 'NONE',  ( 68.71132485994280614, 155.0000000000000000, 15.00000000000001243 ) ) ;
#18005 = CARTESIAN_POINT ( 'NONE',  ( -6.139770520408369237, 215.5359834540460042, 0.9511379180785658471 ) ) ;
#18006 = CARTESIAN_POINT ( 'NONE',  ( 10.01549611932659545, 203.7984951890123853, 70.14886208192139350 ) ) ;
#18007 = ORIENTED_EDGE ( 'NONE', *, *, #9529, .T. ) ;
#18008 = CARTESIAN_POINT ( 'NONE',  ( -0.05014649552828442242, 219.6175466908591716, 81.24886208192143044 ) ) ;
#18009 = CARTESIAN_POINT ( 'NONE',  ( -9.984503880673473830, 210.2968891136704315, 93.65113791807857524 ) ) ;
#18010 = ORIENTED_EDGE ( 'NONE', *, *, #30102, .F. ) ;
#18011 = CARTESIAN_POINT ( 'NONE',  ( 76.57499999726881867, 145.8408176439707802, 12.60653300113718345 ) ) ;
#18012 = CARTESIAN_POINT ( 'NONE',  ( 8.000000000000008882, 207.0476921513415220, 54.99886208192145176 ) ) ;
#18013 = ORIENTED_EDGE ( 'NONE', *, *, #31380, .F. ) ;
#18014 = CARTESIAN_POINT ( 'NONE',  ( 74.02499999726879309, 160.0630714827496206, 15.58253174999999224 ) ) ;
#18015 = CARTESIAN_POINT ( 'NONE',  ( 121.3406204335659879, 155.0000000000000000, -7.500000000000022204 ) ) ;
#18016 = DIRECTION ( 'NONE',  ( 0.000000000000000000, 0.000000000000000000, -1.000000000000000000 ) ) ;
#18017 = CIRCLE ( 'NONE', #19638, 100.0000000000000000 ) ;
#18018 = CARTESIAN_POINT ( 'NONE',  ( 63.52499999726880731, 169.8198683612136222, -4.815267126137197984 ) ) ;
#18019 = CARTESIAN_POINT ( 'NONE',  ( -7.922798540899431252, 4.627424769998836673, -8.057412477672047046 ) ) ;
#18020 = CARTESIAN_POINT ( 'NONE',  ( -3.135527875058982783, 216.4958274776886924, 48.09886208192143187 ) ) ;
#18021 = ORIENTED_EDGE ( 'NONE', *, *, #8231, .T. ) ;
#18022 = DIRECTION ( 'NONE',  ( -0.000000000000000000, -0.000000000000000000, 1.000000000000000000 ) ) ;
#18023 = CARTESIAN_POINT ( 'NONE',  ( 127.5000000000000000, 229.9533188057749555, 74.95331880577313655 ) ) ;
#18024 = CARTESIAN_POINT ( 'NONE',  ( -0.05014649552828365914, 215.4116977939061144, 39.24886208192144466 ) ) ;
#18025 = CARTESIAN_POINT ( 'NONE',  ( 6.220909254589536808, 215.4770327129947702, 67.55113791807853829 ) ) ;
#18026 = CARTESIAN_POINT ( 'NONE',  ( 117.5000000000000142, 155.0000000000000000, -100.0000000000000284 ) ) ;
#18027 = CARTESIAN_POINT ( 'NONE',  ( 6.139770520408368348, 198.4640165459539674, 56.45113791807857950 ) ) ;
#18028 = CARTESIAN_POINT ( 'NONE',  ( 6.220909254589536808, 215.4770327129947702, 31.55113791807857382 ) ) ;
#18029 = CARTESIAN_POINT ( 'NONE',  ( 6.500168698208129925, 211.6636982574063381, 13.70113791807856707 ) ) ;
#18030 = CARTESIAN_POINT ( 'NONE',  ( 46.08867513459482979, 142.2402378747194405, 9.270509831248432420 ) ) ;
#18031 = CARTESIAN_POINT ( 'NONE',  ( 0.5735064479039692076, -3.710337782248087191, -0.1388410611046418386 ) ) ;
#18032 = CARTESIAN_POINT ( 'NONE',  ( 38.02499999726881441, 160.0630714827496206, 15.58253174999999224 ) ) ;
#18033 = CARTESIAN_POINT ( 'NONE',  ( 9.680171189290831535, 199.9079932115568852, 35.30113791807856671 ) ) ;
#18034 = DIRECTION ( 'NONE',  ( -1.000000000000000000, -0.000000000000000000, -0.000000000000000000 ) ) ;
#18035 = CARTESIAN_POINT ( 'NONE',  ( -8.062137200540920645, 212.9164362838581894, 81.80113791807858092 ) ) ;
#18036 = EDGE_CURVE ( 'NONE', #28279, #20901, #27347, .T. ) ;
#18037 = CARTESIAN_POINT ( 'NONE',  ( -8.062137200540920645, 212.9164362838581894, 57.80113791807857382 ) ) ;
#18038 = DIRECTION ( 'NONE',  ( 1.000000000000000000, 0.000000000000000000, 0.000000000000000000 ) ) ;
#18039 = CARTESIAN_POINT ( 'NONE',  ( -9.736236675708031640, 214.0148392665760753, 26.79886208192143826 ) ) ;
#18040 = CARTESIAN_POINT ( 'NONE',  ( 3.135527875058981895, 197.5041725223112792, 31.59886208192143187 ) ) ;
#18041 = AXIS2_PLACEMENT_3D ( 'NONE', #23888, #24049, #21827 ) ;
#18042 = CARTESIAN_POINT ( 'NONE',  ( 74.09999999453764019, 159.7113355953771077, -14.50000000000000888 ) ) ;
#18043 = CARTESIAN_POINT ( 'NONE',  ( -9.736236675707914401, 199.9851607334237542, 63.20113791807857240 ) ) ;
#18044 = CARTESIAN_POINT ( 'NONE',  ( -2.426778023690262742, 214.6231898156240163, 76.10113791807854966 ) ) ;
#18045 = CARTESIAN_POINT ( 'NONE',  ( 8.062137200540822946, 212.9164362838583315, 36.69886208192143329 ) ) ;
#18046 = LINE ( 'NONE', #9876, #15079 ) ;
#18047 = ORIENTED_EDGE ( 'NONE', *, *, #8147, .T. ) ;
#18048 = ADVANCED_FACE ( 'NONE', ( #18795 ), #21341, .T. ) ;
#18049 = CARTESIAN_POINT ( 'NONE',  ( -11.98450388067341876, 203.0532714938636047, 53.34886208192144608 ) ) ;
#18050 = ORIENTED_EDGE ( 'NONE', *, *, #8553, .F. ) ;
#18051 = ORIENTED_EDGE ( 'NONE', *, *, #21846, .F. ) ;
#18052 = FACE_OUTER_BOUND ( 'NONE', #12267, .T. ) ;
#18053 = CARTESIAN_POINT ( 'NONE',  ( 32.50000000000000000, 155.0000000000000000, -6.938893903907228378E-15 ) ) ;
#18054 = VERTEX_POINT ( 'NONE', #29020 ) ;
#18055 = CARTESIAN_POINT ( 'NONE',  ( -8.000000000000008882, 207.0476921513413515, 39.50113791807857666 ) ) ;
#18056 = LINE ( 'NONE', #18227, #922 ) ;
#18057 = CARTESIAN_POINT ( 'NONE',  ( 3.044812012439969795, 216.5253028482143520, 21.39886208192143613 ) ) ;
#18058 = CARTESIAN_POINT ( 'NONE',  ( 61.27499999726881441, 149.9369285172503510, -15.58253175000000823 ) ) ;
#18059 = EDGE_LOOP ( 'NONE', ( #18010, #10 ) ) ;
#18060 = FACE_BOUND ( 'NONE', #23854, .T. ) ;
#18061 = DIRECTION ( 'NONE',  ( 0.000000000000000000, -0.7071067811865346942, 0.7071067811865604513 ) ) ;
#18062 = CARTESIAN_POINT ( 'NONE',  ( 2.517493886309087436, 199.4062855549015865, 1.598862081921434974 ) ) ;
#18063 = EDGE_CURVE ( 'NONE', #161, #9889, #29541, .T. ) ;
#18064 = CARTESIAN_POINT ( 'NONE',  ( -10.00000000000000711, 207.0476921513413515, 42.50113791807856956 ) ) ;
#18065 = CARTESIAN_POINT ( 'NONE',  ( 86.91132485994280898, 146.1832212156128890, 12.13525491562421976 ) ) ;
#18066 =( BOUNDED_CURVE ( )  B_SPLINE_CURVE ( 2, ( #25649, #32341, #1344, #14623, #11731, #9006, #6788, #4060, #7606, #20537, #2316 ),
 .UNSPECIFIED., .F., .F. ) 
 B_SPLINE_CURVE_WITH_KNOTS ( ( 3, 2, 2, 2, 2, 3 ),
 ( 0.07142857142857135522, 0.07499999999999992784, 0.07857142857142850045, 0.08214285714285708695, 0.08571428571428565957, 0.08928571428571423219 ),
 .UNSPECIFIED. ) 
 CURVE ( )  GEOMETRIC_REPRESENTATION_ITEM ( )  RATIONAL_B_SPLINE_CURVE ( ( 1.000000000000000888, 0.9510565162951523099, 1.000000000000000000, 0.9510565162951534202, 1.000000000000000000, 0.9510565162951534202, 1.000000000000000000, 0.9510565162951534202, 1.000000000000000000, 0.9510565162951541973, 0.9999999999999992228 ) ) 
 REPRESENTATION_ITEM ( '' )  );
#18067 = CARTESIAN_POINT ( 'NONE',  ( 3.044812012440130555, 197.4746971517856764, 29.60113791807856742 ) ) ;
#18068 = DIRECTION ( 'NONE',  ( -0.1045284632676344722, 1.217938055844717366E-16, -0.9945218953682752883 ) ) ;
#18069 = APPLICATION_PROTOCOL_DEFINITION ( 'draft international standard', 'automotive_design', 1998, #4855 ) ;
#18070 = CARTESIAN_POINT ( 'NONE',  ( -4.984841277089891776, 213.7757310962905990, 77.94886208192143329 ) ) ;
#18071 = VECTOR ( 'NONE', #6416, 1000.000000000000000 ) ;
#18072 = CARTESIAN_POINT ( 'NONE',  ( 85.00000000000001421, 170.2462022514548323, -7.872454543227099337E-15 ) ) ;
#18073 = DIRECTION ( 'NONE',  ( 0.000000000000000000, 0.000000000000000000, -1.000000000000000000 ) ) ;
#18074 = CARTESIAN_POINT ( 'NONE',  ( 115.4999999999999858, 244.6486928011512134, 52.99999999999884892 ) ) ;
#18075 = CARTESIAN_POINT ( 'NONE',  ( -11.98450388067348804, 210.9467285061362247, 12.65113791807856636 ) ) ;
#18076 = PLANE ( 'NONE',  #14575 ) ;
#18077 = CARTESIAN_POINT ( 'NONE',  ( 49.67499999726879878, 168.2552932293087906, -9.630534252274385310 ) ) ;
#18078 = CARTESIAN_POINT ( 'NONE',  ( -9.984503880673473830, 210.2968891136704315, 57.65113791807858235 ) ) ;
#18079 = ADVANCED_FACE ( 'NONE', ( #13670 ), #13847, .T. ) ;
#18080 = CARTESIAN_POINT ( 'NONE',  ( 35.31132485994280046, 140.7341522555726669, -4.635254915624220651 ) ) ;
#18081 = CARTESIAN_POINT ( 'NONE',  ( 52.41132485994280898, 167.7597621252805880, 9.270509831248428867 ) ) ;
#18082 = CARTESIAN_POINT ( 'NONE',  ( 9.984503880673420539, 210.2968891136705736, 3.848862081921434086 ) ) ;
#18083 = CARTESIAN_POINT ( 'NONE',  ( 51.29999999453762172, 142.6655632788954620, 8.961492836873471646 ) ) ;
#18084 = EDGE_LOOP ( 'NONE', ( #33426, #31262, #28653, #3040 ) ) ;
#18085 = CARTESIAN_POINT ( 'NONE',  ( -7.456977232089304408, 196.8216656703010301, 39.05113791807855961 ) ) ;
#18086 = CARTESIAN_POINT ( 'NONE',  ( 47.11132485994280472, 140.7341522555726669, 4.635254915624211769 ) ) ;
#18087 = CARTESIAN_POINT ( 'NONE',  ( 6.220909254589681581, 198.5229672870052582, 7.448862081921433287 ) ) ;
#18088 = CARTESIAN_POINT ( 'NONE',  ( 60.21132485994281325, 170.7719333635740497, -7.904646289410545231E-15 ) ) ;
#18089 = ORIENTED_EDGE ( 'NONE', *, *, #19742, .F. ) ;
#18090 = EDGE_CURVE ( 'NONE', #17374, #17299, #14183, .T. ) ;
#18091 = DIRECTION ( 'NONE',  ( 1.804112415015879625E-16, -1.000000000000000000, 0.000000000000000000 ) ) ;
#18092 = CARTESIAN_POINT ( 'NONE',  ( -3.135527875058821579, 197.5041725223112223, 11.90113791807856636 ) ) ;
#18093 = CARTESIAN_POINT ( 'NONE',  ( 0.05014649552810505201, 217.5146222423826714, 70.25113791807858377 ) ) ;
#18094 = VERTEX_POINT ( 'NONE', #29517 ) ;
#18095 = CARTESIAN_POINT ( 'NONE',  ( 7.984503880673422316, 209.6470497212048372, 30.84886208192143542 ) ) ;
#18096 = DIRECTION ( 'NONE',  ( 1.000000000000000000, 0.000000000000000000, 0.000000000000000000 ) ) ;
#18097 = EDGE_LOOP ( 'NONE', ( #13928, #16142, #24274, #22639, #31378 ) ) ;
#18098 = AXIS2_PLACEMENT_3D ( 'NONE', #7557, #31061, #28332 ) ;
#18099 = CARTESIAN_POINT ( 'NONE',  ( -2.426778023690262742, 214.6231898156240163, 16.10113791807856742 ) ) ;
#18100 = AXIS2_PLACEMENT_3D ( 'NONE', #8123, #18506, #28890 ) ;
#18101 = ADVANCED_FACE ( 'NONE', ( #3285, #570 ), #24067, .F. ) ;
#18102 = CARTESIAN_POINT ( 'NONE',  ( -12.00000000000000711, 206.9523078486584780, 98.49886208192143044 ) ) ;
#18103 = CARTESIAN_POINT ( 'NONE',  ( 46.87499999726880873, 138.6155565068815747, -3.929120461958505118E-15 ) ) ;
#18104 = VERTEX_POINT ( 'NONE', #6340 ) ;
#18105 = CARTESIAN_POINT ( 'NONE',  ( 51.52499999726881441, 169.8198683612136222, -4.815267126137197984 ) ) ;
#18106 = CARTESIAN_POINT ( 'NONE',  ( 125.5000000000000000, 261.0000000000000000, 0.000000000000000000 ) ) ;
#18107 = CARTESIAN_POINT ( 'NONE',  ( 9.984503880673470277, 203.7031108863295401, 11.15113791807856636 ) ) ;
#18108 = CARTESIAN_POINT ( 'NONE',  ( 6.220909254589681581, 198.5229672870052582, 79.44886208192143329 ) ) ;
#18109 = CARTESIAN_POINT ( 'NONE',  ( 47.07499999726880446, 141.7447067706911810, -9.630534252274385310 ) ) ;
#18110 = CARTESIAN_POINT ( 'NONE',  ( 79.11132485994279762, 140.7341522555726669, 4.635254915624211769 ) ) ;
#18111 = CARTESIAN_POINT ( 'NONE',  ( -6.139770520408369237, 215.5359834540460042, 9.951137918078567068 ) ) ;
#18112 = DIRECTION ( 'NONE',  ( -1.000000000000000000, 0.000000000000000000, 0.000000000000000000 ) ) ;
#18113 = AXIS2_PLACEMENT_3D ( 'NONE', #11414, #27076, #16679 ) ;
#18114 = CARTESIAN_POINT ( 'NONE',  ( 66.59999999999999432, 159.7113355953771077, -14.50000000000000888 ) ) ;
#18115 = CARTESIAN_POINT ( 'NONE',  ( 8.062137200540920645, 201.0835637161417822, 95.30113791807858092 ) ) ;
#18116 = CARTESIAN_POINT ( 'NONE',  ( 65.25000000000000000, 7.347880794884118356E-15, -20.00000000000000355 ) ) ;
#18117 = CARTESIAN_POINT ( 'NONE',  ( -8.062137200540920645, 212.9164362838581894, 84.80113791807856671 ) ) ;
#18118 = CARTESIAN_POINT ( 'NONE',  ( -27.49999999999999645, 10.70896984529281859, -1.097913889158296019 ) ) ;
#18119 = LINE ( 'NONE', #2116, #10216 ) ;
#18120 = CARTESIAN_POINT ( 'NONE',  ( 9.680171189290716072, 214.0920067884432854, 96.69886208192144750 ) ) ;
#18121 = CARTESIAN_POINT ( 'NONE',  ( 72.22499999726881015, 149.9369285172503510, 15.58253174999999580 ) ) ;
#18122 = ORIENTED_EDGE ( 'NONE', *, *, #3976, .T. ) ;
#18123 = FACE_OUTER_BOUND ( 'NONE', #4125, .T. ) ;
#18124 = AXIS2_PLACEMENT_3D ( 'NONE', #11696, #27857, #19531 ) ;
#18125 = CARTESIAN_POINT ( 'NONE',  ( 87.27499999726880731, 149.9369285172503510, -15.58253175000000823 ) ) ;
#18126 = CARTESIAN_POINT ( 'NONE',  ( 12.00000000000000711, 206.9523078486586485, 95.00113791807856956 ) ) ;
#18127 = AXIS2_PLACEMENT_3D ( 'NONE', #17456, #14727, #2298 ) ;
#18128 = CARTESIAN_POINT ( 'NONE',  ( -10.98061573408523195, 206.7617422472766009, 103.7067083923456039 ) ) ;
#18129 = ORIENTED_EDGE ( 'NONE', *, *, #14549, .T. ) ;
#18130 = CARTESIAN_POINT ( 'NONE',  ( 3.135527875058981895, 197.5041725223112792, 88.59886208192143897 ) ) ;
#18131 = CARTESIAN_POINT ( 'NONE',  ( -3.662846001189865142, 195.5725841191952838, 25.89886208192143613 ) ) ;
#18132 = CARTESIAN_POINT ( 'NONE',  ( 12.58016597185466345, -24.49110259512898935, -0.01440555954224961507 ) ) ;
#18133 = CARTESIAN_POINT ( 'NONE',  ( 6.220909254589536808, 215.4770327129947702, 37.55113791807856671 ) ) ;
#18134 = EDGE_LOOP ( 'NONE', ( #26139, #33632, #12855, #12096 ) ) ;
#18135 = CARTESIAN_POINT ( 'NONE',  ( -0.05014649552828365914, 215.4116977939061144, 6.248862081921434886 ) ) ;
#18136 = ADVANCED_FACE ( 'NONE', ( #10965 ), #24410, .F. ) ;
#18137 = ADVANCED_FACE ( 'NONE', ( #16732 ), #13227, .F. ) ;
#18138 = AXIS2_PLACEMENT_3D ( 'NONE', #1967, #9627, #25303 ) ;
#18139 = PLANE ( 'NONE',  #24679 ) ;
#18140 = VERTEX_POINT ( 'NONE', #31899 ) ;
#18141 = CARTESIAN_POINT ( 'NONE',  ( -4.984841277089891776, 213.7757310962905990, 89.94886208192144750 ) ) ;
#18142 = ORIENTED_EDGE ( 'NONE', *, *, #26173, .T. ) ;
#18143 = EDGE_CURVE ( 'NONE', #11140, #210, #18630, .T. ) ;
#18144 =( REPRESENTATION_RELATIONSHIP ('NONE','NONE', #25663, #30243 ) REPRESENTATION_RELATIONSHIP_WITH_TRANSFORMATION ( #23309 )SHAPE_REPRESENTATION_RELATIONSHIP( ) );
#18145 = CARTESIAN_POINT ( 'NONE',  ( -4.984841277089726574, 200.2242689037092305, 30.05113791807857027 ) ) ;
#18146 = CARTESIAN_POINT ( 'NONE',  ( 87.41151231482329820, 167.7028228021052314, -10.03192751310307784 ) ) ;
#18147 = ORIENTED_EDGE ( 'NONE', *, *, #13554, .F. ) ;
#18148 = CARTESIAN_POINT ( 'NONE',  ( 0.000000000000000000, 0.000000000000000000, -16.57418492358057094 ) ) ;
#18149 = AXIS2_PLACEMENT_3D ( 'NONE', #1381, #16371, #26939 ) ;
#18150 = CIRCLE ( 'NONE', #13252, 5.249999999999991118 ) ;
#18151 = EDGE_CURVE ( 'NONE', #11012, #28735, #16243, .T. ) ;
#18152 = CARTESIAN_POINT ( 'NONE',  ( 84.92499999726882720, 145.8408176439707802, -12.60653300113719588 ) ) ;
#18153 = CARTESIAN_POINT ( 'NONE',  ( -7.500000000000000000, -4.330127018922198090, -10.00000000000000000 ) ) ;
#18154 = CARTESIAN_POINT ( 'NONE',  ( -8.015496119326531499, 204.4483345814780364, 90.35113791807857808 ) ) ;
#18155 = DIRECTION ( 'NONE',  ( 1.000000000000000000, 0.000000000000000000, 0.000000000000000000 ) ) ;
#18156 = DIRECTION ( 'NONE',  ( 0.000000000000000000, 0.000000000000000000, 1.000000000000000000 ) ) ;
#18157 = CARTESIAN_POINT ( 'NONE',  ( 48.59999999999999432, 159.7113355953771077, -14.50000000000000888 ) ) ;
#18158 = CARTESIAN_POINT ( 'NONE',  ( -6.500168698208244500, 211.6636982574061676, 62.79886208192144892 ) ) ;
#18159 = CARTESIAN_POINT ( 'NONE',  ( 27.50000000000001776, -15.87713240271472870, -2.456200930618646971 ) ) ;
#18160 = CARTESIAN_POINT ( 'NONE',  ( 50.02499999726880020, 160.0630714827496206, 15.58253174999999402 ) ) ;
#18161 = AXIS2_PLACEMENT_3D ( 'NONE', #2372, #20249, #18038 ) ;
#18162 = CARTESIAN_POINT ( 'NONE',  ( -6.220909254589537696, 198.5229672870051445, 3.051137918078565381 ) ) ;
#18163 = CARTESIAN_POINT ( 'NONE',  ( 0.000000000000000000, -1.759474945355381958, 3.047500000000001208 ) ) ;
#18164 = CARTESIAN_POINT ( 'NONE',  ( 54.32499999726880446, 145.8408176439707802, 12.60653300113718345 ) ) ;
#18165 = CARTESIAN_POINT ( 'NONE',  ( 73.07499999726880446, 141.7447067706911810, -9.630534252274385310 ) ) ;
#18166 = CARTESIAN_POINT ( 'NONE',  ( 0.05014649552807549926, 219.6175466908591716, 67.25113791807856956 ) ) ;
#18167 = LINE ( 'NONE', #17997, #24406 ) ;
#18168 = CARTESIAN_POINT ( 'NONE',  ( 3.662846001190051659, 195.5725841191953691, 5.601137918078566535 ) ) ;
#18169 = CARTESIAN_POINT ( 'NONE',  ( -3.044812012440131443, 216.5253028482142952, 91.10113791807857808 ) ) ;
#18170 = CARTESIAN_POINT ( 'NONE',  ( 3.662846001189864698, 218.4274158808046593, 51.39886208192144323 ) ) ;
#18171 = CARTESIAN_POINT ( 'NONE',  ( -3.044812012439970683, 197.4746971517856196, 55.89886208192143613 ) ) ;
#18172 = PRESENTATION_LAYER_ASSIGNMENT (  '', '', ( #3463 ) ) ;
#18173 = CARTESIAN_POINT ( 'NONE',  ( 0.05014649552807549926, 219.6175466908591716, 100.2511379180785696 ) ) ;
#18174 = DIRECTION ( 'NONE',  ( -0.5000000000000061062, 1.060575238724902601E-16, -0.8660254037844351549 ) ) ;
#18175 = CARTESIAN_POINT ( 'NONE',  ( -3.135527875058821579, 197.5041725223112223, 17.90113791807856458 ) ) ;
#18176 = AXIS2_PLACEMENT_3D ( 'NONE', #13975, #27258, #11259 ) ;
#18177 = CARTESIAN_POINT ( 'NONE',  ( 6.220909254589681581, 198.5229672870052582, 76.44886208192143329 ) ) ;
#18178 = ORIENTED_EDGE ( 'NONE', *, *, #22410, .F. ) ;
#18179 = CARTESIAN_POINT ( 'NONE',  ( 9.736236675708031640, 199.9851607334238963, 79.29886208192144181 ) ) ;
#18180 = CARTESIAN_POINT ( 'NONE',  ( -0.05014649552810635652, 196.4853777576173002, 95.75113791807856956 ) ) ;
#18181 = ORIENTED_EDGE ( 'NONE', *, *, #31340, .F. ) ;
#18182 = CARTESIAN_POINT ( 'NONE',  ( 79.67499999726881299, 168.2552932293087906, -9.630534252274385310 ) ) ;
#18183 = CARTESIAN_POINT ( 'NONE',  ( -2.426778023690076225, 199.3768101843759553, 52.89886208192144323 ) ) ;
#18184 = VERTEX_POINT ( 'NONE', #1075 ) ;
#18185 = CARTESIAN_POINT ( 'NONE',  ( 70.42499999726881299, 141.7447067706911810, 9.630534252274376428 ) ) ;
#18186 = DIRECTION ( 'NONE',  ( 0.000000000000000000, 0.000000000000000000, -1.000000000000000000 ) ) ;
#18187 = DIRECTION ( 'NONE',  ( 0.000000000000000000, -1.000000000000000000, 1.290957005378097920E-14 ) ) ;
#18188 = CARTESIAN_POINT ( 'NONE',  ( 60.62499999726879452, 138.6155565068815463, -3.929120461958505118E-15 ) ) ;
#18189 = CARTESIAN_POINT ( 'NONE',  ( -7.500000000000000000, -4.732323933430407692, -7.493854309896101462 ) ) ;
#18190 = CARTESIAN_POINT ( 'NONE',  ( -3.044812012439970683, 197.4746971517856196, 52.89886208192143613 ) ) ;
#18191 = ORIENTED_EDGE ( 'NONE', *, *, #16455, .T. ) ;
#18192 = DIRECTION ( 'NONE',  ( -1.000000000000000000, 0.000000000000000000, 0.000000000000000000 ) ) ;
#18193 = CIRCLE ( 'NONE', #3490, 31.00000000000000000 ) ;
#18194 =( LENGTH_UNIT ( ) NAMED_UNIT ( * ) SI_UNIT ( .MILLI., .METRE. ) );
#18195 = DIRECTION ( 'NONE',  ( 0.000000000000000000, 0.000000000000000000, -1.000000000000000000 ) ) ;
#18196 = CARTESIAN_POINT ( 'NONE',  ( 8.000000000000008882, 207.0476921513415220, 30.99886208192143400 ) ) ;
#18197 = CONICAL_SURFACE ( 'NONE', #27372, 1.610000000000000098, 0.7853981633974652654 ) ;
#18198 = CARTESIAN_POINT ( 'NONE',  ( 0.05014649552810505201, 217.5146222423826714, 73.25113791807855534 ) ) ;
#18199 = CARTESIAN_POINT ( 'NONE',  ( 44.88867513459483405, 159.8737954434937478, -14.99999999999993072 ) ) ;
#18200 = CARTESIAN_POINT ( 'NONE',  ( -3.044812012440131443, 216.5253028482142952, 58.10113791807857808 ) ) ;
#18201 = CARTESIAN_POINT ( 'NONE',  ( -8.062137200540920645, 212.9164362838581894, 27.80113791807856671 ) ) ;
#18202 = CARTESIAN_POINT ( 'NONE',  ( 6.444103211791042618, 202.2591342207267644, 17.30113791807856671 ) ) ;
#18203 = CARTESIAN_POINT ( 'NONE',  ( 46.48867513459483547, 142.2402378747194405, -9.270509831248439525 ) ) ;
#18204 = DIRECTION ( 'NONE',  ( -0.000000000000000000, -0.000000000000000000, 1.000000000000000000 ) ) ;
#18205 = CARTESIAN_POINT ( 'NONE',  ( 39.52499999726881441, 169.8198683612136222, -4.815267126137197984 ) ) ;
#18206 = CARTESIAN_POINT ( 'NONE',  ( 12.01549611932652972, 210.8513442034534933, 34.85113791807856387 ) ) ;
#18207 = CARTESIAN_POINT ( 'NONE',  ( 3.783380760145018981E-16, -7.895640089090872671, -6.564402953523720718 ) ) ;
#18208 = CARTESIAN_POINT ( 'NONE',  ( 6.139770520408368348, 198.4640165459539674, 83.45113791807858661 ) ) ;
#18209 = CARTESIAN_POINT ( 'NONE',  ( 10.00000000000000711, 206.9523078486586201, 56.00113791807856956 ) ) ;
#18210 = CARTESIAN_POINT ( 'NONE',  ( 37.71132485994279904, 155.0000000000000000, -15.00000000000002487 ) ) ;
#18211 = CARTESIAN_POINT ( 'NONE',  ( 3.662846001189864698, 218.4274158808046593, 24.39886208192143258 ) ) ;
#18212 = CARTESIAN_POINT ( 'NONE',  ( 6.139770520408223575, 215.5359834540460611, 24.54886208192143471 ) ) ;
#18213 = CARTESIAN_POINT ( 'NONE',  ( 78.29999999453762882, 167.3344367211045096, -8.961492836873482304 ) ) ;
#18214 = CARTESIAN_POINT ( 'NONE',  ( 12.01549611932652972, 210.8513442034534933, 64.85113791807857808 ) ) ;
#18215 = CARTESIAN_POINT ( 'NONE',  ( -6.444103211791042618, 211.7408657792732356, 87.80113791807858092 ) ) ;
#18216 = CARTESIAN_POINT ( 'NONE',  ( 6.220909254589681581, 198.5229672870052582, 40.44886208192141908 ) ) ;
#18217 = CARTESIAN_POINT ( 'NONE',  ( 100.2066581602377653, 155.0000000000000000, 13.00000000000001066 ) ) ;
#18219 = VERTEX_POINT ( 'NONE', #11463 ) ;
#18218 = B_SPLINE_CURVE_WITH_KNOTS ( 'NONE', 3,
 ( #26721, #31834, #3383, #511, #667, #21281, #13778, #11070, #21610, #8500 ),
 .UNSPECIFIED., .F., .F.,
 ( 4, 2, 2, 2, 4 ),
 ( 0.000000000000000000, 0.002305503304226490767, 0.004611006608452981534, 0.006916509912679473168, 0.009222013216905964803 ),
 .UNSPECIFIED. ) ;
#18220 = CARTESIAN_POINT ( 'NONE',  ( 12.01549611932659367, 203.1486557965466773, 55.14886208192143613 ) ) ;
#18221 = ORIENTED_EDGE ( 'NONE', *, *, #3675, .T. ) ;
#18222 = ORIENTED_EDGE ( 'NONE', *, *, #2730, .F. ) ;
#18223 = CARTESIAN_POINT ( 'NONE',  ( 78.71132485994280614, 155.0000000000000000, 15.00000000000001243 ) ) ;
#18224 = DIRECTION ( 'NONE',  ( 1.000000000000000000, 0.000000000000000000, 0.000000000000000000 ) ) ;
#18225 = EDGE_LOOP ( 'NONE', ( #4052, #29768, #3367, #19666, #19213 ) ) ;
#18226 = CARTESIAN_POINT ( 'NONE',  ( 4.903702542908601636, 200.1653181626581102, 41.45113791807857240 ) ) ;
#18227 = CARTESIAN_POINT ( 'NONE',  ( -67.50000000000000000, 155.0000000000000000, 37.00000000000001421 ) ) ;
#18228 = EDGE_CURVE ( 'NONE', #26841, #5147, #26810, .T. ) ;
#18229 = CARTESIAN_POINT ( 'NONE',  ( 10.00000000000000711, 207.0476921513415220, 21.99886208192143755 ) ) ;
#18230 = CARTESIAN_POINT ( 'NONE',  ( 61.37499999726880873, 155.0000000000000000, -15.58253175000000823 ) ) ;
#18231 = EDGE_LOOP ( 'NONE', ( #21602, #17709, #9763, #32072 ) ) ;
#18232 = LINE ( 'NONE', #10073, #18889 ) ;
#18233 = SURFACE_STYLE_FILL_AREA ( #31178 ) ;
#18234 = DIRECTION ( 'NONE',  ( 0.000000000000000000, 0.000000000000000000, -1.000000000000000000 ) ) ;
#18235 = CARTESIAN_POINT ( 'NONE',  ( 8.000000000000008882, 207.0476921513415220, 6.998862081921435774 ) ) ;
#18236 = CARTESIAN_POINT ( 'NONE',  ( 3.044812012440130555, 197.4746971517856764, 41.60113791807857808 ) ) ;
#18237 = PRODUCT_DEFINITION_SHAPE ( 'NONE', 'NONE',  #33707 ) ;
#18238 = CARTESIAN_POINT ( 'NONE',  ( 0.05014649552810505201, 217.5146222423826714, 28.25113791807855890 ) ) ;
#18239 = CARTESIAN_POINT ( 'NONE',  ( 97.30927364589244632, 155.0000000000000000, -31.00000000000000000 ) ) ;
#18240 = PRODUCT_CONTEXT ( 'NONE', #28141, 'mechanical' ) ;
#18241 = CARTESIAN_POINT ( 'NONE',  ( -2.426778023690076225, 199.3768101843759553, 94.89886208192145034 ) ) ;
#18242 = CARTESIAN_POINT ( 'NONE',  ( 35.32499999726881157, 164.1591823560292198, -12.60653300113719766 ) ) ;
#18243 = CARTESIAN_POINT ( 'NONE',  ( -4.406842699996122548, 6.115962218725288224, 1.165517335421917267E-15 ) ) ;
#18244 = CARTESIAN_POINT ( 'NONE',  ( 77.30950000000004252, 4.898587196589413815E-16, -4.000000000000000000 ) ) ;
#18245 = CARTESIAN_POINT ( 'NONE',  ( -3.753561863808691168, 195.6020594897209435, 8.901137918078566358 ) ) ;
#18246 = DIRECTION ( 'NONE',  ( 1.000000000000000000, 0.000000000000000000, 0.000000000000000000 ) ) ;
#18247 = CARTESIAN_POINT ( 'NONE',  ( 56.47499999726881015, 149.9369285172503510, 15.58253174999999580 ) ) ;
#18248 = CARTESIAN_POINT ( 'NONE',  ( -3.135527875058821579, 197.5041725223112223, 53.90113791807857524 ) ) ;
#18249 = CARTESIAN_POINT ( 'NONE',  ( 34.91132485994280188, 146.1832212156128890, 12.13525491562421976 ) ) ;
#18250 = FACE_OUTER_BOUND ( 'NONE', #33047, .T. ) ;
#18251 = CARTESIAN_POINT ( 'NONE',  ( 77.50000000000000000, 155.0000000000000000, -70.00000000000000000 ) ) ;
#18252 = CARTESIAN_POINT ( 'NONE',  ( 53.89999999453762314, 150.2886644046228639, -14.50000000000000888 ) ) ;
#18253 = ORIENTED_EDGE ( 'NONE', *, *, #6673, .F. ) ;
#18254 = CARTESIAN_POINT ( 'NONE',  ( -9.680171189290831535, 214.0920067884431148, 39.80113791807857382 ) ) ;
#18255 = CARTESIAN_POINT ( 'NONE',  ( -65.24999999999998579, -6.704941225331758828E-15, 35.00000000000000000 ) ) ;
#18256 = CARTESIAN_POINT ( 'NONE',  ( -3.135527875058982783, 216.4958274776886924, 12.09886208192143542 ) ) ;
#18257 = FACE_OUTER_BOUND ( 'NONE', #19008, .T. ) ;
#18258 = ORIENTED_EDGE ( 'NONE', *, *, #16025, .F. ) ;
#18259 = CARTESIAN_POINT ( 'NONE',  ( 3.135527875058820690, 216.4958274776887492, 67.40113791807857524 ) ) ;
#18260 = ORIENTED_EDGE ( 'NONE', *, *, #21976, .T. ) ;
#18261 = CARTESIAN_POINT ( 'NONE',  ( 4.903702542908435547, 213.8346818373419751, 36.54886208192144892 ) ) ;
#18262 = CARTESIAN_POINT ( 'NONE',  ( 80.58867513459483689, 146.1832212156128890, -12.13525491562423042 ) ) ;
#18263 = ORIENTED_EDGE ( 'NONE', *, *, #30736, .F. ) ;
#18264 = CARTESIAN_POINT ( 'NONE',  ( 8.015496119326531499, 209.5516654185219636, 16.85113791807856742 ) ) ;
#18265 =( BOUNDED_CURVE ( )  B_SPLINE_CURVE ( 2, ( #18302, #28694, #13349, #23743, #5352, #15742, #26138, #2805, #21185, #13187, #23585 ),
 .UNSPECIFIED., .F., .T. ) 
 B_SPLINE_CURVE_WITH_KNOTS ( ( 3, 2, 2, 2, 2, 3 ),
 ( 0.7142857142857141906, 0.7178571428571427493, 0.7214285714285713080, 0.7249999999999999778, 0.7285714285714285365, 0.7321428571428570953 ),
 .UNSPECIFIED. ) 
 CURVE ( )  GEOMETRIC_REPRESENTATION_ITEM ( )  RATIONAL_B_SPLINE_CURVE ( ( 1.000000000000001554, 0.9510565162951518658, 1.000000000000000000, 0.9510565162951534202, 1.000000000000000000, 0.9510565162951534202, 1.000000000000000000, 0.9510565162951534202, 1.000000000000000000, 0.9510565162951534202, 1.000000000000000000 ) ) 
 REPRESENTATION_ITEM ( '' )  );
#18266 = EDGE_CURVE ( 'NONE', #576, #10439, #1914, .T. ) ;
#18267 = CARTESIAN_POINT ( 'NONE',  ( -12.00000000000000711, 206.9523078486584780, 95.49886208192144466 ) ) ;
#18268 = CARTESIAN_POINT ( 'NONE',  ( 41.17499999726881299, 145.8408176439707802, -12.60653300113719588 ) ) ;
#18269 = VERTEX_POINT ( 'NONE', #22691 ) ;
#18270 = CARTESIAN_POINT ( 'NONE',  ( 52.42499999726880588, 141.7447067706911810, 9.630534252274376428 ) ) ;
#18271 = CARTESIAN_POINT ( 'NONE',  ( 79.71132485994280614, 155.0000000000000000, -15.00000000000002487 ) ) ;
#18272 = CARTESIAN_POINT ( 'NONE',  ( 9.984503880673470277, 203.7031108863295401, 8.151137918078564581 ) ) ;
#18273 = CARTESIAN_POINT ( 'NONE',  ( -0.05014649552828403384, 217.5146222423826714, 78.24886208192144466 ) ) ;
#18274 = CARTESIAN_POINT ( 'NONE',  ( 50.37499999726881583, 155.0000000000000000, 15.58253174999999402 ) ) ;
#18275 = CARTESIAN_POINT ( 'NONE',  ( 79.71132485994280614, 155.0000000000000000, -15.00000000000002487 ) ) ;
#18276 = CARTESIAN_POINT ( 'NONE',  ( 6.220909254589536808, 215.4770327129947702, 16.55113791807857027 ) ) ;
#18277 = CARTESIAN_POINT ( 'NONE',  ( 115.4999999999999858, 155.0000000000000000, 112.0000000000000426 ) ) ;
#18278 = ADVANCED_FACE ( 'NONE', ( #9408 ), #25248, .T. ) ;
#18279 = CARTESIAN_POINT ( 'NONE',  ( 65.40000000000000568, 159.7113355953771077, 14.49999999999999289 ) ) ;
#18280 = CARTESIAN_POINT ( 'NONE',  ( -0.05014649552810635652, 196.4853777576173002, 98.75113791807854113 ) ) ;
#18281 = CARTESIAN_POINT ( 'NONE',  ( 25.25629716696159122, 17.17253483735094832, -1.708299986272424853 ) ) ;
#18282 = CARTESIAN_POINT ( 'NONE',  ( -0.05014649552810635652, 196.4853777576173002, 83.75113791807856956 ) ) ;
#18283 = CARTESIAN_POINT ( 'NONE',  ( 91.60208470531341618, 155.0000000000000000, 12.00000000000001066 ) ) ;
#18284 = CARTESIAN_POINT ( 'NONE',  ( 38.27499999726881441, 160.0630714827496206, 15.58253174999999402 ) ) ;
#18285 = CARTESIAN_POINT ( 'NONE',  ( -7.375838497908014268, 196.7627149292498530, 101.0488620819214276 ) ) ;
#18286 = CARTESIAN_POINT ( 'NONE',  ( 73.72499999726881015, 169.8198683612136222, 4.815267126137181997 ) ) ;
#18287 = ORIENTED_EDGE ( 'NONE', *, *, #23034, .F. ) ;
#18288 = CARTESIAN_POINT ( 'NONE',  ( 115.4999999999999858, 65.35130719884917028, -52.99999999999947420 ) ) ;
#18289 = CARTESIAN_POINT ( 'NONE',  ( 35.39999999453763024, 141.2096805137202580, 4.480746418436733158 ) ) ;
#18290 = CARTESIAN_POINT ( 'NONE',  ( 0.05014649552807549926, 219.6175466908591716, 100.2511379180785696 ) ) ;
#18291 = EDGE_CURVE ( 'NONE', #19123, #21804, #14315, .T. ) ;
#18292 = LINE ( 'NONE', #33459, #21359 ) ;
#18293 = VERTEX_POINT ( 'NONE', #27627 ) ;
#18294 = CARTESIAN_POINT ( 'NONE',  ( -8.118202686958138514, 212.8392687619910930, 83.79886208192144181 ) ) ;
#18295 = CARTESIAN_POINT ( 'NONE',  ( 3.662846001189864698, 218.4274158808046593, 24.39886208192143258 ) ) ;
#18296 = DIRECTION ( 'NONE',  ( 1.000000000000000000, -0.000000000000000000, -0.000000000000000000 ) ) ;
#18297 = CARTESIAN_POINT ( 'NONE',  ( -3.044812012440131443, 216.5253028482142952, 46.10113791807857098 ) ) ;
#18298 = ADVANCED_FACE ( 'NONE', ( #29862 ), #30711, .T. ) ;
#18299 = VERTEX_POINT ( 'NONE', #18833 ) ;
#18300 = CARTESIAN_POINT ( 'NONE',  ( -6.444103211790928043, 202.2591342207265939, 8.198862081921436840 ) ) ;
#18301 = AXIS2_PLACEMENT_3D ( 'NONE', #32259, #14539, #30221 ) ;
#18302 = CARTESIAN_POINT ( 'NONE',  ( 73.71132485994280614, 155.0000000000000000, -15.00000000000002487 ) ) ;
#18303 = ORIENTED_EDGE ( 'NONE', *, *, #12655, .T. ) ;
#18304 = CARTESIAN_POINT ( 'NONE',  ( 7.984503880673422316, 209.6470497212048372, 90.84886208192142476 ) ) ;
#18305 = ORIENTED_EDGE ( 'NONE', *, *, #6476, .F. ) ;
#18306 = CARTESIAN_POINT ( 'NONE',  ( -6.500168698208129925, 202.3363017425936050, 27.20113791807857240 ) ) ;
#18307 = CARTESIAN_POINT ( 'NONE',  ( 7.500000000000001776, 0.000000000000000000, 0.000000000000000000 ) ) ;
#18309 = ORIENTED_EDGE ( 'NONE', *, *, #15569, .F. ) ;
#18308 = VECTOR ( 'NONE', #25013, 1000.000000000000000 ) ;
#18310 = CARTESIAN_POINT ( 'NONE',  ( 33.62499999726881583, 171.3844434931184253, -7.942151717890132712E-15 ) ) ;
#18311 = CARTESIAN_POINT ( 'NONE',  ( 34.27499999726880731, 160.0630714827496206, 15.58253174999999402 ) ) ;
#18312 = CARTESIAN_POINT ( 'NONE',  ( 0.000000000000000000, 0.000000000000000000, -7.554475477074173106 ) ) ;
#18313 = CARTESIAN_POINT ( 'NONE',  ( -8.015496119326531499, 204.4483345814780364, 87.35113791807857808 ) ) ;
#18314 = CARTESIAN_POINT ( 'NONE',  ( 112.4999999999999858, 155.0000000000000000, 49.99999999999999289 ) ) ;
#18315 = CARTESIAN_POINT ( 'NONE',  ( 45.39999999999999858, 159.7113355953771077, 14.49999999999999289 ) ) ;
#18316 = CARTESIAN_POINT ( 'NONE',  ( 0.05014649552828262524, 198.5883022060938572, 64.74886208192143044 ) ) ;
#18317 = LINE ( 'NONE', #16084, #33583 ) ;
#18318 = ADVANCED_FACE ( 'NONE', ( #16277 ), #5611, .T. ) ;
#18319 = ADVANCED_FACE ( 'NONE', ( #8284 ), #7958, .F. ) ;
#18320 = CARTESIAN_POINT ( 'NONE',  ( 50.72499999726881725, 140.1801316387863778, -4.815267126137194431 ) ) ;
#18321 = CARTESIAN_POINT ( 'NONE',  ( 10.00000000000000711, 206.9523078486586201, 5.001137918078565114 ) ) ;
#18322 = CARTESIAN_POINT ( 'NONE',  ( -67.50000000000000000, 0.000000000000000000, 270.4495957273638282 ) ) ;
#18323 = CARTESIAN_POINT ( 'NONE',  ( 66.12499999726881583, 155.0000000000000000, 15.58253174999999402 ) ) ;
#18324 = CARTESIAN_POINT ( 'NONE',  ( 67.37499999726881583, 155.0000000000000000, -15.58253175000000823 ) ) ;
#18325 = CARTESIAN_POINT ( 'NONE',  ( -12.01549611932652972, 203.1486557965464499, 66.35113791807857808 ) ) ;
#18326 = CARTESIAN_POINT ( 'NONE',  ( 45.71132485994280614, 155.0000000000000000, -15.00000000000002487 ) ) ;
#18327 = CARTESIAN_POINT ( 'NONE',  ( 0.05014649552807549926, 219.6175466908591716, 13.25113791807856423 ) ) ;
#18328 = EDGE_CURVE ( 'NONE', #6680, #17702, #6477, .T. ) ;
#18329 = CARTESIAN_POINT ( 'NONE',  ( 10.00000000000000711, 206.9523078486586201, 92.00113791807858377 ) ) ;
#18330 = CARTESIAN_POINT ( 'NONE',  ( 109.0104235265664272, 155.0000000000000000, 0.000000000000000000 ) ) ;
#18331 = VECTOR ( 'NONE', #14734, 1000.000000000000000 ) ;
#18332 = CARTESIAN_POINT ( 'NONE',  ( 9.680171189290716072, 214.0920067884432854, 48.69886208192144039 ) ) ;
#18333 = CARTESIAN_POINT ( 'NONE',  ( -3.135527875058982783, 216.4958274776886924, 60.09886208192143897 ) ) ;
#18334 = CARTESIAN_POINT ( 'NONE',  ( 11.98450388067348271, 203.0532714938637753, 101.1511379180785895 ) ) ;
#18335 = CARTESIAN_POINT ( 'NONE',  ( 33.88867513459481984, 150.1262045565062806, 14.99999999999992006 ) ) ;
#18336 = CARTESIAN_POINT ( 'NONE',  ( -10.00000000000000711, 207.0476921513413515, 15.50113791807856600 ) ) ;
#18337 = EDGE_CURVE ( 'NONE', #17930, #16872, #1284, .T. ) ;
#18338 = CARTESIAN_POINT ( 'NONE',  ( 8.062137200540822946, 212.9164362838583315, 78.69886208192143329 ) ) ;
#18339 = ORIENTED_EDGE ( 'NONE', *, *, #2525, .T. ) ;
#18340 = CARTESIAN_POINT ( 'NONE',  ( -7.456977232089471386, 217.1783343296987709, 80.94886208192143329 ) ) ;
#18341 = CARTESIAN_POINT ( 'NONE',  ( 10.00000000000000711, 206.9523078486586201, 98.00113791807856956 ) ) ;
#18342 = ORIENTED_EDGE ( 'NONE', *, *, #29441, .T. ) ;
#18343 = CARTESIAN_POINT ( 'NONE',  ( 3.500000000000004885, 2.020725942163702715, -0.3126073911696551910 ) ) ;
#18344 = CARTESIAN_POINT ( 'NONE',  ( -8.000000000000008882, 206.9523078486584780, 62.49886208192144466 ) ) ;
#18345 = AXIS2_PLACEMENT_3D ( 'NONE', #24612, #13876, #21876 ) ;
#18346 = ORIENTED_EDGE ( 'NONE', *, *, #9576, .T. ) ;
#18347 = CIRCLE ( 'NONE', #920, 0.7733184030943203169 ) ;
#18348 = CARTESIAN_POINT ( 'NONE',  ( 79.82499999726881867, 168.2552932293087906, 9.630534252274372875 ) ) ;
#18349 = CARTESIAN_POINT ( 'NONE',  ( -2.141486166123589996, 6.269165884987821791, -0.07763482564820804732 ) ) ;
#18350 = CARTESIAN_POINT ( 'NONE',  ( -6.902527771671634227, -4.675077770780906583, -0.7026937717022867513 ) ) ;
#18351 = CARTESIAN_POINT ( 'NONE',  ( 62.12499999726880873, 155.0000000000000000, 15.58253174999999402 ) ) ;
#18352 = CARTESIAN_POINT ( 'NONE',  ( 32.50000000000000000, 155.0000000000000000, -6.938893903907228378E-15 ) ) ;
#18353 = CARTESIAN_POINT ( 'NONE',  ( -6.220909254589682469, 215.4770327129946850, 47.94886208192144039 ) ) ;
#18354 = EDGE_CURVE ( 'NONE', #12982, #19514, #1115, .T. ) ;
#18355 = ORIENTED_EDGE ( 'NONE', *, *, #26058, .T. ) ;
#18356 = AXIS2_PLACEMENT_3D ( 'NONE', #8419, #21353, #31588 ) ;
#18357 = DIRECTION ( 'NONE',  ( -1.000000000000000000, 0.000000000000000000, 0.000000000000000000 ) ) ;
#18358 =( NAMED_UNIT ( * ) SI_UNIT ( $, .STERADIAN. ) SOLID_ANGLE_UNIT ( ) );
#18359 = CARTESIAN_POINT ( 'NONE',  ( -4.250000000000000000, 5.204748896376250699E-16, -0.5251556536572846712 ) ) ;
#18360 = CARTESIAN_POINT ( 'NONE',  ( 7.984503880673422316, 209.6470497212048372, 30.84886208192143542 ) ) ;
#18361 = CARTESIAN_POINT ( 'NONE',  ( 8.118202686958039038, 212.8392687619912635, 82.70113791807857240 ) ) ;
#18362 = CARTESIAN_POINT ( 'NONE',  ( 63.08867513459481557, 167.7597621252805880, -9.270509831248443078 ) ) ;
#18363 = CARTESIAN_POINT ( 'NONE',  ( 3.044812012440130555, 197.4746971517856764, 53.60113791807857098 ) ) ;
#18364 = EDGE_CURVE ( 'NONE', #16076, #33380, #24656, .T. ) ;
#18365 = CARTESIAN_POINT ( 'NONE',  ( -3.135527875058821579, 197.5041725223112223, 29.90113791807856813 ) ) ;
#18366 = CARTESIAN_POINT ( 'NONE',  ( 2.517493886308900919, 214.5937144450984420, 10.40113791807856636 ) ) ;
#18367 = CARTESIAN_POINT ( 'NONE',  ( 8.000000000000000000, 5.388445916248354013E-16, 4.400000000000001243 ) ) ;
#18368 = DIRECTION ( 'NONE',  ( -1.000000000000000000, -0.000000000000000000, -0.000000000000000000 ) ) ;
#18369 = CARTESIAN_POINT ( 'NONE',  ( 35.92499999726880588, 164.1591823560292198, 12.60653300113718167 ) ) ;
#18370 = CARTESIAN_POINT ( 'NONE',  ( 12.01549611932652972, 210.8513442034534933, 37.85113791807856387 ) ) ;
#18371 = CARTESIAN_POINT ( 'NONE',  ( -5.357619327558936585E-16, 7.505553499465137612, -6.064240316920400886 ) ) ;
#18372 = AXIS2_PLACEMENT_3D ( 'NONE', #12906, #27697, #11184 ) ;
#18373 = CARTESIAN_POINT ( 'NONE',  ( 3.044812012440130555, 197.4746971517856764, 89.60113791807857808 ) ) ;
#18374 = CARTESIAN_POINT ( 'NONE',  ( -6.139770520408368348, 215.5359834540460042, 57.95113791807855819 ) ) ;
#18375 = PRESENTATION_LAYER_ASSIGNMENT (  '', '', ( #28149 ) ) ;
#18376 = CARTESIAN_POINT ( 'NONE',  ( -7.375838497908014268, 196.7627149292498530, 26.04886208192144181 ) ) ;
#18377 = CARTESIAN_POINT ( 'NONE',  ( -6.139770520408224463, 198.4640165459539105, 32.04886208192143471 ) ) ;
#18378 = CARTESIAN_POINT ( 'NONE',  ( 81.69999999453762030, 142.6655632788954620, -8.961492836873480528 ) ) ;
#18379 = CARTESIAN_POINT ( 'NONE',  ( 9.736236675707914401, 214.0148392665762458, 70.70113791807857240 ) ) ;
#18380 = CARTESIAN_POINT ( 'NONE',  ( -4.903702542908602524, 213.8346818373418898, 90.95113791807855819 ) ) ;
#18381 = CARTESIAN_POINT ( 'NONE',  ( 0.05014649552828275708, 196.4853777576173002, 52.74886208192143044 ) ) ;
#18382 = DIRECTION ( 'NONE',  ( -0.000000000000000000, -0.000000000000000000, -1.000000000000000000 ) ) ;
#18383 = VECTOR ( 'NONE', #14034, 1000.000000000000000 ) ;
#18384 = VERTEX_POINT ( 'NONE', #6391 ) ;
#18385 = CARTESIAN_POINT ( 'NONE',  ( 0.05014649552828288198, 194.3824533091408000, 52.74886208192143755 ) ) ;
#18386 = ORIENTED_EDGE ( 'NONE', *, *, #21820, .F. ) ;
#18387 = ORIENTED_EDGE ( 'NONE', *, *, #22179, .T. ) ;
#18388 = FACE_OUTER_BOUND ( 'NONE', #1705, .T. ) ;
#18389 = CARTESIAN_POINT ( 'NONE',  ( 54.75000000000000000, 7.990820364436479461E-15, 20.00000000000000000 ) ) ;
#18390 = CARTESIAN_POINT ( 'NONE',  ( 6.500168698208129925, 211.6636982574063381, 46.70113791807857240 ) ) ;
#18391 = AXIS2_PLACEMENT_3D ( 'NONE', #21351, #31747, #1414 ) ;
#18392 = DIRECTION ( 'NONE',  ( 0.000000000000000000, -1.000000000000000000, 0.000000000000000000 ) ) ;
#18393 = VECTOR ( 'NONE', #9799, 1000.000000000000114 ) ;
#18394 = CARTESIAN_POINT ( 'NONE',  ( -0.05014649552828403384, 217.5146222423826714, 27.24886208192142689 ) ) ;
#18395 = CARTESIAN_POINT ( 'NONE',  ( 64.57499999726881867, 145.8408176439707802, 12.60653300113718345 ) ) ;
#18396 = VERTEX_POINT ( 'NONE', #3833 ) ;
#18397 = CARTESIAN_POINT ( 'NONE',  ( 68.78867513459482552, 155.0000000000000000, -15.00000000000002487 ) ) ;
#18398 = CIRCLE ( 'NONE', #25445, 1.610000000000000098 ) ;
#18399 = DIRECTION ( 'NONE',  ( 1.000000000000000000, 0.000000000000000000, 0.000000000000000000 ) ) ;
#18400 = CARTESIAN_POINT ( 'NONE',  ( -4.903702542908436435, 200.1653181626580249, 5.048862081921433820 ) ) ;
#18401 = CARTESIAN_POINT ( 'NONE',  ( -9.984503880673473830, 210.2968891136704315, 45.65113791807855392 ) ) ;
#18402 = CARTESIAN_POINT ( 'NONE',  ( 87.11132485994279762, 140.7341522555726669, 4.635254915624211769 ) ) ;
#18403 = CARTESIAN_POINT ( 'NONE',  ( 6.220909254589536808, 215.4770327129947702, 25.55113791807856671 ) ) ;
#18404 = CARTESIAN_POINT ( 'NONE',  ( -0.05014649552828402690, 217.5146222423826714, 99.24886208192144466 ) ) ;
#18405 = VECTOR ( 'NONE', #24517, 1000.000000000000000 ) ;
#18406 = APPLICATION_PROTOCOL_DEFINITION ( 'draft international standard', 'automotive_design', 1998, #28786 ) ;
#18407 = CARTESIAN_POINT ( 'NONE',  ( -6.500168698208244500, 211.6636982574061676, 89.79886208192142760 ) ) ;
#18408 = CARTESIAN_POINT ( 'NONE',  ( 41.22499999726881015, 160.0630714827496206, -15.58253175000000823 ) ) ;
#18409 = CARTESIAN_POINT ( 'NONE',  ( -56.97195197156149504, 194.9507991595696694, 1.985452284598899553 ) ) ;
#18410 = DIRECTION ( 'NONE',  ( 0.000000000000000000, -1.295896757998781966E-15, -1.000000000000000000 ) ) ;
#18411 = CARTESIAN_POINT ( 'NONE',  ( -7.456977232089304408, 196.8216656703010301, 12.05113791807856849 ) ) ;
#18412 = CARTESIAN_POINT ( 'NONE',  ( 63.98867513459482836, 146.1832212156128890, 12.13525491562421976 ) ) ;
#18413 = CARTESIAN_POINT ( 'NONE',  ( 60.07499999726879736, 168.2552932293087906, 9.630534252274372875 ) ) ;
#18414 = CARTESIAN_POINT ( 'NONE',  ( -6.139770520408369237, 215.5359834540460042, 51.95113791807857950 ) ) ;
#18415 = CARTESIAN_POINT ( 'NONE',  ( -8.062137200540920645, 212.9164362838581894, 30.80113791807856671 ) ) ;
#18416 = CARTESIAN_POINT ( 'NONE',  ( 87.62499999726880162, 171.3844434931184253, -7.942151717890132712E-15 ) ) ;
#18417 = CARTESIAN_POINT ( 'NONE',  ( -12.58016597185465457, 24.49110259512897159, -17.98559444045776345 ) ) ;
#18418 = CARTESIAN_POINT ( 'NONE',  ( 10.00000000000000711, 207.0476921513415220, 0.9988620819214341084 ) ) ;
#18419 = CARTESIAN_POINT ( 'NONE',  ( 61.79999999453762882, 146.4771138417591203, -11.73074641843674470 ) ) ;
#18420 = EDGE_LOOP ( 'NONE', ( #29736, #31084, #13374, #899 ) ) ;
#18421 = CARTESIAN_POINT ( 'NONE',  ( -11.98450388067348804, 210.9467285061362247, 42.65113791807856813 ) ) ;
#18422 = AXIS2_PLACEMENT_3D ( 'NONE', #12198, #22585, #32971 ) ;
#18423 = DIRECTION ( 'NONE',  ( -1.000000000000000000, 0.000000000000000000, 0.000000000000000000 ) ) ;
#18424 = ADVANCED_FACE ( 'NONE', ( #29397 ), #30076, .T. ) ;
#18425 = CARTESIAN_POINT ( 'NONE',  ( 6.220909254589681581, 198.5229672870052582, 22.44886208192143329 ) ) ;
#18426 = CIRCLE ( 'NONE', #24399, 12.00000000000001066 ) ;
#18427 = CARTESIAN_POINT ( 'NONE',  ( 72.61132485994281183, 159.8737954434936057, 15.00000000000001421 ) ) ;
#18428 = ORIENTED_EDGE ( 'NONE', *, *, #31380, .T. ) ;
#18429 = CARTESIAN_POINT ( 'NONE',  ( 9.984503880673470277, 203.7031108863295401, 71.15113791807857524 ) ) ;
#18430 = ORIENTED_EDGE ( 'NONE', *, *, #11822, .T. ) ;
#18431 = VECTOR ( 'NONE', #22461, 1000.000000000000000 ) ;
#18432 = CARTESIAN_POINT ( 'NONE',  ( 70.71132485994280614, 155.0000000000000000, 15.00000000000001243 ) ) ;
#18433 = CARTESIAN_POINT ( 'NONE',  ( 32.50000000000000000, 155.0000000000000000, 13.00000000000001066 ) ) ;
#18434 = VERTEX_POINT ( 'NONE', #14224 ) ;
#18435 = CARTESIAN_POINT ( 'NONE',  ( 2.426778023690261410, 199.3768101843759837, 17.60113791807856742 ) ) ;
#18436 = CARTESIAN_POINT ( 'NONE',  ( 0.05014649552828288198, 194.3824533091408000, 100.7488620819214304 ) ) ;
#18437 = CARTESIAN_POINT ( 'NONE',  ( 44.87499999726880873, 138.6155565068815747, -3.929120461958505118E-15 ) ) ;
#18438 = EDGE_LOOP ( 'NONE', ( #15944, #14885, #18886, #17372, #691 ) ) ;
#18439 = CARTESIAN_POINT ( 'NONE',  ( 53.62499999726881583, 171.3844434931184253, -7.942151717890132712E-15 ) ) ;
#18440 = CARTESIAN_POINT ( 'NONE',  ( 129.5873785388598662, 2.643999646947254867, 35.00001199999999812 ) ) ;
#18441 = CARTESIAN_POINT ( 'NONE',  ( -6.139770520408369237, 215.5359834540460042, 12.95113791807856352 ) ) ;
#18442 = AXIS2_PLACEMENT_3D ( 'NONE', #18322, #20377, #20709 ) ;
#18443 = CARTESIAN_POINT ( 'NONE',  ( 6.220909254589681581, 198.5229672870052582, 85.44886208192140487 ) ) ;
#18444 = CARTESIAN_POINT ( 'NONE',  ( 54.57499999726881157, 145.8408176439707802, 12.60653300113718345 ) ) ;
#18445 = CARTESIAN_POINT ( 'NONE',  ( 52.38867513459481984, 140.7341522555726669, -4.635254915624220651 ) ) ;
#18446 = CARTESIAN_POINT ( 'NONE',  ( -8.062137200540920645, 212.9164362838581894, 12.80113791807856671 ) ) ;
#18447 = LINE ( 'NONE', #18277, #29010 ) ;
#18448 = VECTOR ( 'NONE', #1206, 1000.000000000000000 ) ;
#18449 = CARTESIAN_POINT ( 'NONE',  ( -3.750000000000007105, -6.495190528383289141, 0.000000000000000000 ) ) ;
#18450 = CARTESIAN_POINT ( 'NONE',  ( 68.09999999999999432, 141.2096805137202580, -4.480746418436742040 ) ) ;
#18451 = CARTESIAN_POINT ( 'NONE',  ( 3.044812012440130555, 197.4746971517856764, 95.60113791807857808 ) ) ;
#18452 = CARTESIAN_POINT ( 'NONE',  ( 38.58867513459482268, 146.1832212156128890, -12.13525491562423042 ) ) ;
#18453 = CARTESIAN_POINT ( 'NONE',  ( -8.118202686958039038, 201.1607312380087080, 87.20113791807858661 ) ) ;
#18454 = DIRECTION ( 'NONE',  ( 1.000000000000000000, 0.000000000000000000, 0.000000000000000000 ) ) ;
#18455 = CARTESIAN_POINT ( 'NONE',  ( 38.17499999726881299, 164.1591823560292198, 12.60653300113718167 ) ) ;
#18456 = CARTESIAN_POINT ( 'NONE',  ( 7.375838497908012492, 217.2372850707501186, 93.54886208192142760 ) ) ;
#18457 = AXIS2_PLACEMENT_3D ( 'NONE', #22011, #8271, #2826 ) ;
#18458 = CARTESIAN_POINT ( 'NONE',  ( 67.72499999726881015, 169.8198683612136222, 4.815267126137181997 ) ) ;
#18459 = VERTEX_POINT ( 'NONE', #24792 ) ;
#18460 = DIRECTION ( 'NONE',  ( 0.5526942671207055735, 0.1536855300543024383, 0.8190908404712107238 ) ) ;
#18461 = CARTESIAN_POINT ( 'NONE',  ( 41.09999999453763309, 150.2886644046228639, 14.49999999999999645 ) ) ;
#18462 = CARTESIAN_POINT ( 'NONE',  ( -7.375838497908014268, 196.7627149292498530, 2.048862081921434264 ) ) ;
#18463 = PLANE ( 'NONE',  #26806 ) ;
#18464 = EDGE_CURVE ( 'NONE', #7333, #33037, #14382, .T. ) ;
#18465 = ORIENTED_EDGE ( 'NONE', *, *, #19971, .F. ) ;
#18466 = CARTESIAN_POINT ( 'NONE',  ( 0.05014649552828275014, 196.4853777576173002, 94.74886208192141623 ) ) ;
#18467 = CARTESIAN_POINT ( 'NONE',  ( -3.753561863808878130, 218.3979405102790281, 27.09886208192143897 ) ) ;
#18468 = CARTESIAN_POINT ( 'NONE',  ( 117.5000000000000142, 155.0000000000000000, 70.00000000000000000 ) ) ;
#18469 = ADVANCED_FACE ( 'NONE', ( #32283, #9112 ), #22062, .T. ) ;
#18470 = CIRCLE ( 'NONE', #29895, 13.49999999999996980 ) ;
#18471 = CARTESIAN_POINT ( 'NONE',  ( -10.00000000000000711, 207.0476921513413515, 45.50113791807857666 ) ) ;
#18472 = VERTEX_POINT ( 'NONE', #13887 ) ;
#18473 = CARTESIAN_POINT ( 'NONE',  ( 8.118202686958138514, 201.1607312380088501, 103.2988620819214418 ) ) ;
#18474 = EDGE_CURVE ( 'NONE', #16441, #8613, #29906, .T. ) ;
#18475 = FACE_BOUND ( 'NONE', #12556, .T. ) ;
#18476 = ORIENTED_EDGE ( 'NONE', *, *, #8294, .F. ) ;
#18477 = CARTESIAN_POINT ( 'NONE',  ( 7.984503880673422316, 209.6470497212048372, 93.84886208192143897 ) ) ;
#18478 = CARTESIAN_POINT ( 'NONE',  ( 4.903702542908601636, 200.1653181626581102, 26.45113791807857240 ) ) ;
#18479 = DIRECTION ( 'NONE',  ( 1.000000000000000000, 0.000000000000000000, 0.000000000000000000 ) ) ;
#18480 = ORIENTED_EDGE ( 'NONE', *, *, #1000, .F. ) ;
#18481 = CARTESIAN_POINT ( 'NONE',  ( 5.335963852943280017, 6.035591050531201596, -7.593821156097048330 ) ) ;
#18482 = CARTESIAN_POINT ( 'NONE',  ( 33.77499999726880731, 169.8198683612136222, -4.815267126137197984 ) ) ;
#18483 = FACE_OUTER_BOUND ( 'NONE', #6126, .T. ) ;
#18484 = CARTESIAN_POINT ( 'NONE',  ( -2.517493886308901807, 199.4062855549015012, 92.90113791807857524 ) ) ;
#18485 = DIRECTION ( 'NONE',  ( 0.000000000000000000, 0.000000000000000000, 1.000000000000000000 ) ) ;
#18486 = CARTESIAN_POINT ( 'NONE',  ( 47.30000000000000426, 163.5228861582408797, 11.73074641843673049 ) ) ;
#18487 = CARTESIAN_POINT ( 'NONE',  ( -4.903702542908436435, 200.1653181626580249, 62.04886208192144181 ) ) ;
#18488 = AXIS2_PLACEMENT_3D ( 'NONE', #30480, #7142, #31287 ) ;
#18489 = CARTESIAN_POINT ( 'NONE',  ( 83.71132485994282035, 155.0000000000000000, -15.00000000000002487 ) ) ;
#18490 = EDGE_CURVE ( 'NONE', #7971, #14298, #27208, .T. ) ;
#18491 = CARTESIAN_POINT ( 'NONE',  ( 51.22499999726881015, 160.0630714827496206, -15.58253175000000823 ) ) ;
#18492 = CARTESIAN_POINT ( 'NONE',  ( -8.118202686958039038, 201.1607312380087080, 9.201137918078565292 ) ) ;
#18493 = CARTESIAN_POINT ( 'NONE',  ( 4.000000000000000000, -1.759474945355381958, 3.047500000000001208 ) ) ;
#18494 = CARTESIAN_POINT ( 'NONE',  ( 65.92499999726881299, 164.1591823560292198, 12.60653300113718167 ) ) ;
#18495 = CARTESIAN_POINT ( 'NONE',  ( 74.77499999726880731, 140.1801316387863778, 4.815267126137185549 ) ) ;
#18496 = CARTESIAN_POINT ( 'NONE',  ( -3.753561863808691168, 195.6020594897209435, 71.90113791807856103 ) ) ;
#18497 = DIRECTION ( 'NONE',  ( 0.000000000000000000, 0.000000000000000000, -1.000000000000000000 ) ) ;
#18498 = CARTESIAN_POINT ( 'NONE',  ( -6.220909254589537696, 198.5229672870051445, 90.05113791807858092 ) ) ;
#18499 = ADVANCED_FACE ( 'NONE', ( #31941 ), #15398, .F. ) ;
#18500 = CARTESIAN_POINT ( 'NONE',  ( 35.28867513459481842, 170.7719333635740497, -7.904646289410545231E-15 ) ) ;
#18501 = ORIENTED_EDGE ( 'NONE', *, *, #24317, .F. ) ;
#18502 = CARTESIAN_POINT ( 'NONE',  ( -9.736236675708031640, 214.0148392665760753, 47.79886208192143471 ) ) ;
#18503 = CARTESIAN_POINT ( 'NONE',  ( -10.00000000000000711, 206.9523078486584495, 62.49886208192143755 ) ) ;
#18504 = CARTESIAN_POINT ( 'NONE',  ( 9.680171189290831535, 199.9079932115568852, 95.30113791807858092 ) ) ;
#18505 = SHAPE_REPRESENTATION ( 'pad arm left_left', ( #2404 ), #29608 ) ;
#18506 = DIRECTION ( 'NONE',  ( -1.000000000000000000, 0.000000000000000000, 0.000000000000000000 ) ) ;
#18507 = CARTESIAN_POINT ( 'NONE',  ( 3.044812012440130555, 197.4746971517856764, 11.60113791807856742 ) ) ;
#18508 = CARTESIAN_POINT ( 'NONE',  ( -8.118202686958138514, 212.8392687619910930, 74.79886208192144181 ) ) ;
#18509 = ORIENTED_EDGE ( 'NONE', *, *, #21939, .F. ) ;
#18510 = CARTESIAN_POINT ( 'NONE',  ( -10.00000000000000711, 207.0476921513413515, 99.50113791807856956 ) ) ;
#18511 = ORIENTED_EDGE ( 'NONE', *, *, #17989, .T. ) ;
#18512 = CARTESIAN_POINT ( 'NONE',  ( 4.000000000000000000, 1.759474945355380404, -3.047500000000001652 ) ) ;
#18513 = PRODUCT_DEFINITION_CONTEXT ( 'detailed design', #282, 'design' ) ;
#18514 = CARTESIAN_POINT ( 'NONE',  ( -4.984841277089891776, 213.7757310962905990, 62.94886208192144039 ) ) ;
#18515 = EDGE_LOOP ( 'NONE', ( #32044, #20696 ) ) ;
#18516 = EDGE_CURVE ( 'NONE', #15495, #11974, #21723, .T. ) ;
#18517 = CARTESIAN_POINT ( 'NONE',  ( 78.82499999726881867, 141.7447067706911810, -9.630534252274387086 ) ) ;
#18518 = DIRECTION ( 'NONE',  ( 0.000000000000000000, 0.000000000000000000, 1.000000000000000000 ) ) ;
#18519 = DIRECTION ( 'NONE',  ( -1.000000000000000000, -0.000000000000000000, -0.000000000000000000 ) ) ;
#18520 = UNCERTAINTY_MEASURE_WITH_UNIT (LENGTH_MEASURE( 1.000000000000000082E-05 ), #23960, 'distance_accuracy_value', 'NONE');
#18521 = CARTESIAN_POINT ( 'NONE',  ( 72.02499999726882152, 160.0630714827496206, 15.58253174999999402 ) ) ;
#18522 = EDGE_CURVE ( 'NONE', #21262, #20010, #3661, .T. ) ;
#18523 = CARTESIAN_POINT ( 'NONE',  ( -4.984841277089726574, 200.2242689037092305, 63.05113791807858092 ) ) ;
#18524 = DIRECTION ( 'NONE',  ( 0.000000000000000000, -1.000000000000000000, 3.227392513445223895E-15 ) ) ;
#18525 = CARTESIAN_POINT ( 'NONE',  ( 64.50000000000000000, 0.000000000000000000, 30.00000000000000000 ) ) ;
#18526 = DIRECTION ( 'NONE',  ( 0.8191520442889923537, 0.000000000000000000, 0.5735764363510453823 ) ) ;
#18527 = CARTESIAN_POINT ( 'NONE',  ( -4.984841277089891776, 213.7757310962905990, 35.94886208192144039 ) ) ;
#18528 = CARTESIAN_POINT ( 'NONE',  ( 3.135527875058820690, 216.4958274776887492, 79.40113791807857524 ) ) ;
#18529 = CARTESIAN_POINT ( 'NONE',  ( 0.000000000000000000, 0.000000000000000000, 0.000000000000000000 ) ) ;
#18530 = CARTESIAN_POINT ( 'NONE',  ( -10.00000000000000711, 207.0476921513413515, 57.50113791807856956 ) ) ;
#18531 = AXIS2_PLACEMENT_3D ( 'NONE', #31841, #26559, #5945 ) ;
#18532 = CARTESIAN_POINT ( 'NONE',  ( -9.984503880673473830, 210.2968891136704315, 24.65113791807856103 ) ) ;
#18533 = CARTESIAN_POINT ( 'NONE',  ( -0.05014649552807731031, 198.5883022060938572, 14.75113791807856600 ) ) ;
#18534 = CARTESIAN_POINT ( 'NONE',  ( 86.97499999726882436, 140.1801316387863778, -4.815267126137194431 ) ) ;
#18535 = CARTESIAN_POINT ( 'NONE',  ( 60.28867513459481842, 139.2280666364260071, -4.041636747397287284E-15 ) ) ;
#18536 = CARTESIAN_POINT ( 'NONE',  ( 41.92499999726881299, 164.1591823560292198, 12.60653300113718167 ) ) ;
#18537 = CARTESIAN_POINT ( 'NONE',  ( -3.662846001190052991, 218.4274158808045740, 40.10113791807856387 ) ) ;
#18538 = CARTESIAN_POINT ( 'NONE',  ( 7.500000000000000000, 0.7723602884954153813, -7.026388801733942202 ) ) ;
#18539 = CARTESIAN_POINT ( 'NONE',  ( -3.135527875058821579, 197.5041725223112223, 80.90113791807858945 ) ) ;
#18540 = CARTESIAN_POINT ( 'NONE',  ( -10.01549611932653860, 203.7984951890123000, 60.35113791807857808 ) ) ;
#18541 = CARTESIAN_POINT ( 'NONE',  ( 3.753561863808876797, 195.6020594897209719, 19.59886208192143897 ) ) ;
#18542 = CARTESIAN_POINT ( 'NONE',  ( 3.135527875058981895, 197.5041725223112792, 28.59886208192143897 ) ) ;
#18543 = CARTESIAN_POINT ( 'NONE',  ( 82.49999999453764588, 170.2462022514548323, -7.872454543227099337E-15 ) ) ;
#18544 = CARTESIAN_POINT ( 'NONE',  ( 3.753561863808689836, 218.3979405102790565, 64.40113791807856103 ) ) ;
#18545 = CARTESIAN_POINT ( 'NONE',  ( 0.05014649552807626948, 215.4116977939061144, 91.25113791807856956 ) ) ;
#18546 = CARTESIAN_POINT ( 'NONE',  ( -3.135527875058982783, 216.4958274776886924, 54.09886208192143897 ) ) ;
#18547 = CARTESIAN_POINT ( 'NONE',  ( 3.783380760145018981E-16, -7.895640089090872671, -6.564402953523720718 ) ) ;
#18548 = ORIENTED_EDGE ( 'NONE', *, *, #1464, .F. ) ;
#18549 = CARTESIAN_POINT ( 'NONE',  ( 9.680171189290716072, 214.0920067884432854, 48.69886208192144039 ) ) ;
#18550 = ORIENTED_EDGE ( 'NONE', *, *, #29747, .F. ) ;
#18551 = ORIENTED_EDGE ( 'NONE', *, *, #7035, .T. ) ;
#18552 = EDGE_CURVE ( 'NONE', #29718, #25762, #7074, .T. ) ;
#18553 = ADVANCED_FACE ( 'NONE', ( #2135 ), #32782, .T. ) ;
#18554 = CARTESIAN_POINT ( 'NONE',  ( 78.57499999726881867, 145.8408176439707802, 12.60653300113718345 ) ) ;
#18555 = CARTESIAN_POINT ( 'NONE',  ( -5.007715329123872641E-16, -8.660254037844399733, -7.422398894150038728 ) ) ;
#18556 = CARTESIAN_POINT ( 'NONE',  ( 55.88867513459482694, 150.1262045565064227, 15.00000000000001599 ) ) ;
#18557 = CARTESIAN_POINT ( 'NONE',  ( -2.426778023690262742, 214.6231898156240163, 40.10113791807857098 ) ) ;
#18558 = EDGE_CURVE ( 'NONE', #5848, #4155, #30751, .T. ) ;
#18559 = EDGE_CURVE ( 'NONE', #9072, #8169, #4343, .T. ) ;
#18560 =( NAMED_UNIT ( * ) PLANE_ANGLE_UNIT ( ) SI_UNIT ( $, .RADIAN. ) );
#18561 = CARTESIAN_POINT ( 'NONE',  ( 6.220909254589681581, 198.5229672870052582, 22.44886208192143329 ) ) ;
#18562 = CARTESIAN_POINT ( 'NONE',  ( 62.87499999726880873, 138.6155565068815747, -3.929120461958505118E-15 ) ) ;
#18563 = ORIENTED_EDGE ( 'NONE', *, *, #24349, .T. ) ;
#18564 = CARTESIAN_POINT ( 'NONE',  ( 62.38867513459482694, 140.7341522555726669, -4.635254915624220651 ) ) ;
#18565 = FILL_AREA_STYLE ('',( #26717 ) ) ;
#18566 = CYLINDRICAL_SURFACE ( 'NONE', #7588, 2.149999999999979483 ) ;
#18567 = CARTESIAN_POINT ( 'NONE',  ( 6.500168698208244500, 202.3363017425938324, 10.29886208192143471 ) ) ;
#18568 = CARTESIAN_POINT ( 'NONE',  ( 6.220909254589536808, 215.4770327129947702, 52.55113791807858092 ) ) ;
#18569 = CARTESIAN_POINT ( 'NONE',  ( -58.50000000000001421, -88.00000000000000000, 20.00000000000000000 ) ) ;
#18570 = CARTESIAN_POINT ( 'NONE',  ( 6.220909254589536808, 215.4770327129947702, 28.55113791807855961 ) ) ;
#18571 = CARTESIAN_POINT ( 'NONE',  ( 86.57499999726880446, 145.8408176439707802, 12.60653300113718345 ) ) ;
#18572 = APPLICATION_PROTOCOL_DEFINITION ( 'draft international standard', 'automotive_design', 1998, #282 ) ;
#18573 = CIRCLE ( 'NONE', #31086, 3.499999999999999556 ) ;
#18574 = CARTESIAN_POINT ( 'NONE',  ( 8.015496119326595448, 204.4483345814782638, 91.14886208192143613 ) ) ;
#18575 = CARTESIAN_POINT ( 'NONE',  ( 38.32499999726881157, 145.8408176439707802, 12.60653300113718345 ) ) ;
#18576 = CARTESIAN_POINT ( 'NONE',  ( -125.0000000000000000, -95.00000000000000000, 270.4495957273638282 ) ) ;
#18577 = CARTESIAN_POINT ( 'NONE',  ( -52.50000000000002132, 155.0000000000000000, 6.938893903907228378E-15 ) ) ;
#18578 = CARTESIAN_POINT ( 'NONE',  ( 12.01549611932652972, 210.8513442034534933, 13.85113791807856742 ) ) ;
#18579 = DIRECTION ( 'NONE',  ( 0.000000000000000000, 0.000000000000000000, -1.000000000000000000 ) ) ;
#18580 = CARTESIAN_POINT ( 'NONE',  ( 58.77499999726881441, 140.1801316387863778, 4.815267126137185549 ) ) ;
#18581 = CARTESIAN_POINT ( 'NONE',  ( 10.00000000000000711, 206.9523078486586201, 53.00113791807857666 ) ) ;
#18582 = CARTESIAN_POINT ( 'NONE',  ( -0.05014649552810635652, 196.4853777576173002, 32.75113791807856956 ) ) ;
#18583 = LINE ( 'NONE', #525, #26800 ) ;
#18584 = DIRECTION ( 'NONE',  ( 0.000000000000000000, 0.000000000000000000, -1.000000000000000000 ) ) ;
#18585 = CARTESIAN_POINT ( 'NONE',  ( 10.00000000000000711, 207.0476921513415220, 3.998862081921434442 ) ) ;
#18586 = CARTESIAN_POINT ( 'NONE',  ( 60.09999999453762598, 159.7113355953771077, -14.50000000000000888 ) ) ;
#18587 = VERTEX_POINT ( 'NONE', #17794 ) ;
#18588 = CARTESIAN_POINT ( 'NONE',  ( 9.736236675707914401, 214.0148392665762458, 43.70113791807857240 ) ) ;
#18589 = CARTESIAN_POINT ( 'NONE',  ( 77.41132485994280898, 142.2402378747194405, -9.270509831248439525 ) ) ;
#18590 = CARTESIAN_POINT ( 'NONE',  ( 10.00000000000000711, 207.0476921513415220, 24.99886208192143400 ) ) ;
#18591 =( REPRESENTATION_RELATIONSHIP ('NONE','NONE', #25663, #16299 ) REPRESENTATION_RELATIONSHIP_WITH_TRANSFORMATION ( #12235 )SHAPE_REPRESENTATION_RELATIONSHIP( ) );
#18592 = DIRECTION ( 'NONE',  ( -1.000000000000000000, 0.000000000000000000, 0.000000000000000000 ) ) ;
#18593 = ORIENTED_EDGE ( 'NONE', *, *, #30216, .T. ) ;
#18594 = CARTESIAN_POINT ( 'NONE',  ( 0.05014649552810505201, 217.5146222423826714, 73.25113791807855534 ) ) ;
#18595 = ORIENTED_EDGE ( 'NONE', *, *, #27010, .T. ) ;
#18596 = DIRECTION ( 'NONE',  ( -0.000000000000000000, -0.000000000000000000, -1.000000000000000000 ) ) ;
#18597 = CARTESIAN_POINT ( 'NONE',  ( -58.50000000000002132, 185.0000000000000000, 0.000000000000000000 ) ) ;
#18598 = VECTOR ( 'NONE', #26119, 1000.000000000000000 ) ;
#18599 = VERTEX_POINT ( 'NONE', #15066 ) ;
#18600 = CARTESIAN_POINT ( 'NONE',  ( 6.500168698208129925, 211.6636982574063381, 13.70113791807856707 ) ) ;
#18601 = B_SPLINE_CURVE_WITH_KNOTS ( 'NONE', 3,
 ( #16177, #19907, #14796, #22467, #27747, #6631 ),
 .UNSPECIFIED., .F., .F.,
 ( 4, 2, 4 ),
 ( 0.004444412883774346255, 0.006655097293744437204, 0.008865781703714529019 ),
 .UNSPECIFIED. ) ;
#18602 = CARTESIAN_POINT ( 'NONE',  ( -11.98450388067341876, 203.0532714938636047, 101.3488620819214390 ) ) ;
#18603 = CARTESIAN_POINT ( 'NONE',  ( 46.27499999726881441, 160.0630714827496206, 15.58253174999999224 ) ) ;
#18604 = ORIENTED_EDGE ( 'NONE', *, *, #4398, .F. ) ;
#18605 = CARTESIAN_POINT ( 'NONE',  ( 47.72499999726881015, 169.8198683612136222, 4.815267126137181997 ) ) ;
#18606 = DIRECTION ( 'NONE',  ( 0.000000000000000000, 0.000000000000000000, 1.000000000000000000 ) ) ;
#18607 = CARTESIAN_POINT ( 'NONE',  ( -0.05014649552810635652, 196.4853777576173002, 5.751137918078563338 ) ) ;
#18608 = VECTOR ( 'NONE', #30086, 1000.000000000000000 ) ;
#18609 = CARTESIAN_POINT ( 'NONE',  ( -6.220909254589682469, 215.4770327129946850, 83.94886208192143329 ) ) ;
#18610 = CARTESIAN_POINT ( 'NONE',  ( 55.57499999726881157, 164.1591823560292198, -12.60653300113719766 ) ) ;
#18611 = CARTESIAN_POINT ( 'NONE',  ( -10.00000000000000711, 207.0476921513413515, 24.50113791807856600 ) ) ;
#18612 = FACE_OUTER_BOUND ( 'NONE', #20100, .T. ) ;
#18613 = CARTESIAN_POINT ( 'NONE',  ( 71.09999999999999432, 168.7903194862797420, 4.480746418436729606 ) ) ;
#18614 = CARTESIAN_POINT ( 'NONE',  ( 10.00000000000000711, 206.9523078486586201, 101.0011379180785696 ) ) ;
#18615 = CARTESIAN_POINT ( 'NONE',  ( 37.98867513459482126, 146.1832212156128890, 12.13525491562421976 ) ) ;
#18616 = CARTESIAN_POINT ( 'NONE',  ( -3.135527875058821579, 197.5041725223112223, 89.90113791807857524 ) ) ;
#18617 = DIRECTION ( 'NONE',  ( 0.000000000000000000, 1.000000000000000000, 0.000000000000000000 ) ) ;
#18618 = CARTESIAN_POINT ( 'NONE',  ( 40.97499999726881725, 140.1801316387863778, -4.815267126137194431 ) ) ;
#18619 = CARTESIAN_POINT ( 'NONE',  ( 12.00000000000000711, 207.0476921513415220, 96.99886208192143044 ) ) ;
#18620 = CARTESIAN_POINT ( 'NONE',  ( 76.42499999726879878, 141.7447067706911810, 9.630534252274376428 ) ) ;
#18621 = EDGE_LOOP ( 'NONE', ( #21889, #17961, #31617 ) ) ;
#18622 = DIRECTION ( 'NONE',  ( 0.000000000000000000, 0.000000000000000000, -1.000000000000000000 ) ) ;
#18623 = CARTESIAN_POINT ( 'NONE',  ( 39.09999999453763309, 150.2886644046228639, 14.49999999999999645 ) ) ;
#18624 = LINE ( 'NONE', #26954, #26313 ) ;
#18625 = DIRECTION ( 'NONE',  ( 1.000000000000000000, 0.000000000000000000, 0.000000000000000000 ) ) ;
#18626 = ORIENTED_EDGE ( 'NONE', *, *, #22085, .T. ) ;
#18627 = CARTESIAN_POINT ( 'NONE',  ( 10.01549611932659367, 203.7984951890124421, 91.14886208192142192 ) ) ;
#18628 = AXIS2_PLACEMENT_3D ( 'NONE', #18106, #25934, #2609 ) ;
#18629 = CARTESIAN_POINT ( 'NONE',  ( -0.05014649552828442242, 219.6175466908591716, 33.24886208192143755 ) ) ;
#18630 = LINE ( 'NONE', #11138, #22462 ) ;
#18631 = CARTESIAN_POINT ( 'NONE',  ( 6.139770520408368348, 198.4640165459539674, 38.45113791807855819 ) ) ;
#18632 = ORIENTED_EDGE ( 'NONE', *, *, #23130, .T. ) ;
#18633 = CIRCLE ( 'NONE', #12162, 6.500000000000000000 ) ;
#18634 = CARTESIAN_POINT ( 'NONE',  ( -6.139770520408224463, 198.4640165459539389, 104.0488620819214276 ) ) ;
#18635 = CYLINDRICAL_SURFACE ( 'NONE', #6713, 2.149999999999974598 ) ;
#18636 = ORIENTED_EDGE ( 'NONE', *, *, #21658, .F. ) ;
#18637 = CARTESIAN_POINT ( 'NONE',  ( 2.426778023690075337, 214.6231898156240447, 87.39886208192143613 ) ) ;
#18638 = CARTESIAN_POINT ( 'NONE',  ( -6.500168698208129925, 202.3363017425936050, 33.20113791807857240 ) ) ;
#18639 = DIRECTION ( 'NONE',  ( 0.000000000000000000, 0.000000000000000000, -1.000000000000000000 ) ) ;
#18640 = VERTEX_POINT ( 'NONE', #12006 ) ;
#18641 = CARTESIAN_POINT ( 'NONE',  ( 2.621328321948289020, 7.606199919103058704, -7.633618187056857352 ) ) ;
#18642 = AXIS2_PLACEMENT_3D ( 'NONE', #23599, #5197, #10658 ) ;
#18643 = CARTESIAN_POINT ( 'NONE',  ( 34.77499999726880731, 140.1801316387863778, 4.815267126137185549 ) ) ;
#18644 = DIRECTION ( 'NONE',  ( 1.000000000000000000, 0.000000000000000000, 0.000000000000000000 ) ) ;
#18645 = CARTESIAN_POINT ( 'NONE',  ( 8.000000000000008882, 206.9523078486586485, 86.00113791807856956 ) ) ;
#18646 = EDGE_CURVE ( 'NONE', #18911, #12386, #12135, .T. ) ;
#18648 = VECTOR ( 'NONE', #17965, 1000.000000000000000 ) ;
#18647 = DIRECTION ( 'NONE',  ( 1.000000000000000000, 0.000000000000000000, 0.000000000000000000 ) ) ;
#18649 = CARTESIAN_POINT ( 'NONE',  ( 56.99999999999999289, 170.2462022514548323, -7.872454543227099337E-15 ) ) ;
#18650 = CARTESIAN_POINT ( 'NONE',  ( 8.015496119326595448, 204.4483345814782638, 73.14886208192142192 ) ) ;
#18651 = CARTESIAN_POINT ( 'NONE',  ( 89.50000000000001421, 155.0000000000000000, -70.00000000000000000 ) ) ;
#18652 = CIRCLE ( 'NONE', #17554, 2.149999999999985256 ) ;
#18653 = CARTESIAN_POINT ( 'NONE',  ( 52.32499999726881157, 145.8408176439707802, 12.60653300113718345 ) ) ;
#18654 = CARTESIAN_POINT ( 'NONE',  ( 3.044812012440130555, 197.4746971517856764, 11.60113791807856742 ) ) ;
#18655 = CARTESIAN_POINT ( 'NONE',  ( 62.71132485994281325, 155.0000000000000000, 15.00000000000001243 ) ) ;
#18656 = CARTESIAN_POINT ( 'NONE',  ( 62.12499999726880873, 155.0000000000000000, 15.58253174999999402 ) ) ;
#18657 = CARTESIAN_POINT ( 'NONE',  ( 74.07499999726880446, 168.2552932293087906, 9.630534252274372875 ) ) ;
#18658 = CARTESIAN_POINT ( 'NONE',  ( 12.01549611932652972, 210.8513442034534933, 73.85113791807857808 ) ) ;
#18659 = CARTESIAN_POINT ( 'NONE',  ( 48.91132485994280188, 146.1832212156128890, 12.13525491562421976 ) ) ;
#18660 = CARTESIAN_POINT ( 'NONE',  ( -10.01549611932653860, 203.7984951890123000, 96.35113791807856387 ) ) ;
#18661 = DIRECTION ( 'NONE',  ( -1.000000000000000000, 0.000000000000000000, 0.000000000000000000 ) ) ;
#18662 = ORIENTED_EDGE ( 'NONE', *, *, #21677, .T. ) ;
#18663 = CARTESIAN_POINT ( 'NONE',  ( 7.375838497908012492, 217.2372850707501186, 60.54886208192144181 ) ) ;
#18664 = VECTOR ( 'NONE', #5072, 1000.000000000000000 ) ;
#18665 = CARTESIAN_POINT ( 'NONE',  ( 6.220909254589680693, 198.5229672870052582, 64.44886208192141908 ) ) ;
#18666 = CARTESIAN_POINT ( 'NONE',  ( 9.736236675708031640, 199.9851607334238963, 1.298862081921434264 ) ) ;
#18667 = CARTESIAN_POINT ( 'NONE',  ( 92.60208470531341618, 155.0000000000000000, 0.000000000000000000 ) ) ;
#18668 = CARTESIAN_POINT ( 'NONE',  ( 10.01549611932653860, 210.2015048109876716, 16.85113791807856032 ) ) ;
#18669 = CARTESIAN_POINT ( 'NONE',  ( 3.135527875058981895, 197.5041725223112792, 82.59886208192143897 ) ) ;
#18670 = ORIENTED_EDGE ( 'NONE', *, *, #5182, .T. ) ;
#18671 = DIRECTION ( 'NONE',  ( 1.000000000000000000, 0.000000000000000000, 0.000000000000000000 ) ) ;
#18672 = CIRCLE ( 'NONE', #1813, 2.149999999999984812 ) ;
#18673 = ORIENTED_EDGE ( 'NONE', *, *, #10323, .F. ) ;
#18674 = CARTESIAN_POINT ( 'NONE',  ( -3.999999999999999112, 0.000000000000000000, -7.974599999999998801 ) ) ;
#18675 = CARTESIAN_POINT ( 'NONE',  ( 8.000000000000008882, 207.0476921513415220, 63.99886208192143044 ) ) ;
#18676 = ADVANCED_FACE ( 'NONE', ( #1957 ), #22841, .F. ) ;
#18677 = CONICAL_SURFACE ( 'NONE', #1263, 32.00000000000000000, 0.1047197551197016768 ) ;
#18678 = EDGE_LOOP ( 'NONE', ( #29651, #21801, #16744, #26301 ) ) ;
#18679 = AXIS2_PLACEMENT_3D ( 'NONE', #25083, #27803, #19810 ) ;
#18680 = CARTESIAN_POINT ( 'NONE',  ( 80.62499999726880162, 138.6155565068815747, -3.929120461958505118E-15 ) ) ;
#18681 = CARTESIAN_POINT ( 'NONE',  ( 32.50000000000000000, 155.0000000000000000, -6.938893903907228378E-15 ) ) ;
#18682 = FACE_OUTER_BOUND ( 'NONE', #21486, .T. ) ;
#18683 = CARTESIAN_POINT ( 'NONE',  ( 70.12499999726881583, 155.0000000000000000, 15.58253174999999402 ) ) ;
#18684 = CARTESIAN_POINT ( 'NONE',  ( 8.000000000000008882, 206.9523078486586485, 62.00113791807856956 ) ) ;
#18685 = SURFACE_SIDE_STYLE ('',( #31954 ) ) ;
#18686 = EDGE_CURVE ( 'NONE', #9657, #32876, #9969, .T. ) ;
#18687 = CARTESIAN_POINT ( 'NONE',  ( -9.638035089578760761, 206.0123451664802587, 104.4144579948609390 ) ) ;
#18688 =( LENGTH_UNIT ( ) NAMED_UNIT ( * ) SI_UNIT ( .MILLI., .METRE. ) );
#18689 = CARTESIAN_POINT ( 'NONE',  ( 7.914984360234579519, -3.818534719232097974, -7.907701344400643428 ) ) ;
#18690 = MECHANICAL_DESIGN_GEOMETRIC_PRESENTATION_REPRESENTATION (  '', ( #14337 ), #3944 ) ;
#18691 = CARTESIAN_POINT ( 'NONE',  ( -8.000000000000008882, 206.9523078486584780, 44.49886208192143755 ) ) ;
#18692 = CARTESIAN_POINT ( 'NONE',  ( -3.044812012440131443, 216.5253028482142952, 85.10113791807857808 ) ) ;
#18693 = CARTESIAN_POINT ( 'NONE',  ( 117.5000000000000000, 207.9999999999998010, -91.79869280115066488 ) ) ;
#18694 = CARTESIAN_POINT ( 'NONE',  ( 3.135527875058820690, 216.4958274776887492, 67.40113791807857524 ) ) ;
#18695 = EDGE_CURVE ( 'NONE', #17290, #27125, #12683, .T. ) ;
#18696 = CARTESIAN_POINT ( 'NONE',  ( -125.0000000000000000, 0.000000000000000000, 35.00000000000000000 ) ) ;
#18697 = CARTESIAN_POINT ( 'NONE',  ( -4.903702542908602524, 213.8346818373418898, 15.95113791807856707 ) ) ;
#18698 = LINE ( 'NONE', #32304, #18970 ) ;
#18699 = COLOUR_RGB ( '', 0.66274510, 0.83137255, 0.94901961) ;
#18700 = CARTESIAN_POINT ( 'NONE',  ( 42.02499999726880731, 160.0630714827496206, 15.58253174999999224 ) ) ;
#18701 =( BOUNDED_CURVE ( )  B_SPLINE_CURVE ( 2, ( #22127, #32517, #19580, #29973, #27411, #27570, #4237, #32857, #4071, #1683, #23320 ),
 .UNSPECIFIED., .F., .T. ) 
 B_SPLINE_CURVE_WITH_KNOTS ( ( 3, 2, 2, 2, 2, 3 ),
 ( 0.1964285714285710915, 0.1999999999999996780, 0.2035714285714282368, 0.2071428571428568233, 0.2107142857142853820, 0.2142857142857139685 ),
 .UNSPECIFIED. ) 
 CURVE ( )  GEOMETRIC_REPRESENTATION_ITEM ( )  RATIONAL_B_SPLINE_CURVE ( ( 1.000000000000004219, 0.9510565162951492013, 1.000000000000000000, 0.9510565162951534202, 1.000000000000000000, 0.9510565162951534202, 1.000000000000000000, 0.9510565162951534202, 1.000000000000000000, 0.9510565162951564178, 0.9999999999999970024 ) ) 
 REPRESENTATION_ITEM ( '' )  );
#18702 = CARTESIAN_POINT ( 'NONE',  ( -12.00000000000000711, 207.0476921513413515, 48.50113791807856956 ) ) ;
#18703 = CARTESIAN_POINT ( 'NONE',  ( 7.894787914004607998, 0.7661396099416312166, -7.591390474663430865 ) ) ;
#18704 = AXIS2_PLACEMENT_3D ( 'NONE', #2770, #20481, #20982 ) ;
#18705 = CARTESIAN_POINT ( 'NONE',  ( -10.01549611932653860, 203.7984951890123284, 99.35113791807857808 ) ) ;
#18706 = CARTESIAN_POINT ( 'NONE',  ( 10.00000000000000711, 206.9523078486586201, 62.00113791807856956 ) ) ;
#18707 = VECTOR ( 'NONE', #33074, 1000.000000000000000 ) ;
#18708 = CARTESIAN_POINT ( 'NONE',  ( 11.98450388067341876, 210.9467285061363953, 18.84886208192143187 ) ) ;
#18709 = CARTESIAN_POINT ( 'NONE',  ( -6.139770520408224463, 198.4640165459539105, 38.04886208192143471 ) ) ;
#18710 = CARTESIAN_POINT ( 'NONE',  ( 78.79999999453762882, 163.5228861582408797, 11.73074641843673049 ) ) ;
#18711 = B_SPLINE_CURVE_WITH_KNOTS ( 'NONE', 3,
 ( #4838, #28352, #12667, #10632, #17616, #28677, #23064, #4669, #33456, #20341, #7907, #30740, #28522, #13014, #17780, #23571, #10128, #20508, #30911, #7576, #2794, #17962, #15557, #23406, #5006, #240, #15394, #2123, #25793, #69, #2458, #30563, #15053, #12839 ),
 .UNSPECIFIED., .F., .F.,
 ( 4, 2, 2, 2, 2, 2, 2, 2, 2, 2, 2, 2, 2, 2, 2, 2, 4 ),
 ( 0.000000000000000000, 0.0004886277888461246482, 0.0009772555776922492964, 0.001465883366538373945, 0.001954511155384498593, 0.002443138944230623458, 0.002931766733076747889, 0.003420394521922872320, 0.003909022310768997185, 0.004397650099615122050, 0.004886277888461246915, 0.005374905677307370913, 0.005863533466153495778, 0.006352161254999620643, 0.006840789043845744641, 0.007329416832691869506, 0.007818044621537994371 ),
 .UNSPECIFIED. ) ;
#18712 = CARTESIAN_POINT ( 'NONE',  ( 12.01549611932652972, 210.8513442034534933, 76.85113791807856387 ) ) ;
#18713 = CARTESIAN_POINT ( 'NONE',  ( -8.015496119326531499, 204.4483345814780364, 93.35113791807857808 ) ) ;
#18714 = EDGE_CURVE ( 'NONE', #17208, #23288, #10139, .T. ) ;
#18715 = CARTESIAN_POINT ( 'NONE',  ( -6.220909254589682469, 215.4770327129946850, 50.94886208192141908 ) ) ;
#18716 = CARTESIAN_POINT ( 'NONE',  ( 32.50000000000000000, 155.0000000000000000, -6.938893903907228378E-15 ) ) ;
#18717 = EDGE_LOOP ( 'NONE', ( #11430, #5407, #21551, #19796 ) ) ;
#18718 = CARTESIAN_POINT ( 'NONE',  ( 12.01549611932659367, 203.1486557965466773, 52.14886208192143613 ) ) ;
#18719 = ORIENTED_EDGE ( 'NONE', *, *, #863, .T. ) ;
#18720 = EDGE_CURVE ( 'NONE', #11477, #12975, #20521, .T. ) ;
#18721 = ORIENTED_EDGE ( 'NONE', *, *, #8088, .F. ) ;
#18722 = CARTESIAN_POINT ( 'NONE',  ( 76.97499999726881015, 140.1801316387863778, -4.815267126137194431 ) ) ;
#18723 = DIRECTION ( 'NONE',  ( 0.000000000000000000, -1.000000000000000000, 1.295896757998781966E-15 ) ) ;
#18724 = CARTESIAN_POINT ( 'NONE',  ( 59.08867513459482979, 167.7597621252805880, -9.270509831248443078 ) ) ;
#18725 = CARTESIAN_POINT ( 'NONE',  ( 0.05014649552807626948, 215.4116977939061144, 55.25113791807857666 ) ) ;
#18726 = VECTOR ( 'NONE', #29147, 1000.000000000000000 ) ;
#18727 = CARTESIAN_POINT ( 'NONE',  ( 6.220909254589681581, 198.5229672870052582, 31.44886208192142263 ) ) ;
#18728 = CARTESIAN_POINT ( 'NONE',  ( 64.87499999726881583, 138.6155565068815747, -3.929120461958505118E-15 ) ) ;
#18729 = VERTEX_POINT ( 'NONE', #1616 ) ;
#18730 = CARTESIAN_POINT ( 'NONE',  ( 36.21132485994281325, 170.7719333635740497, -7.904646289410545231E-15 ) ) ;
#18731 = DIRECTION ( 'NONE',  ( -0.000000000000000000, -0.000000000000000000, 1.000000000000000000 ) ) ;
#18732 = CARTESIAN_POINT ( 'NONE',  ( 2.426778023690075337, 214.6231898156240447, 6.398862081921435241 ) ) ;
#18733 = CARTESIAN_POINT ( 'NONE',  ( -0.05014649552810635652, 196.4853777576173002, 50.75113791807856956 ) ) ;
#18734 = DIRECTION ( 'NONE',  ( 0.000000000000000000, 0.000000000000000000, -1.000000000000000000 ) ) ;
#18735 = CARTESIAN_POINT ( 'NONE',  ( 6.139770520408368348, 198.4640165459539674, 35.45113791807857240 ) ) ;
#18736 = CARTESIAN_POINT ( 'NONE',  ( 81.97499999726881015, 169.8198683612136222, 4.815267126137181997 ) ) ;
#18737 = CONTEXT_DEPENDENT_SHAPE_REPRESENTATION ( #29029, #31569 ) ;
#18738 = CARTESIAN_POINT ( 'NONE',  ( 2.426778023690075337, 214.6231898156240447, 90.39886208192143613 ) ) ;
#18739 = CARTESIAN_POINT ( 'NONE',  ( 39.12499999726880873, 155.0000000000000000, -15.58253175000000823 ) ) ;
#18740 = CARTESIAN_POINT ( 'NONE',  ( 0.000000000000000000, 0.8865213383406687075, -1.535500000000000975 ) ) ;
#18741 = CARTESIAN_POINT ( 'NONE',  ( -9.680171189290831535, 214.0920067884431148, 12.80113791807856849 ) ) ;
#18742 = CARTESIAN_POINT ( 'NONE',  ( 82.28867513459483973, 139.2280666364260071, -4.041636747397287284E-15 ) ) ;
#18743 = CARTESIAN_POINT ( 'NONE',  ( 54.47499999726880304, 149.9369285172503510, 15.58253174999999580 ) ) ;
#18744 = EDGE_CURVE ( 'NONE', #24712, #8601, #6897, .T. ) ;
#18745 = CARTESIAN_POINT ( 'NONE',  ( -6.139770520408369237, 215.5359834540460042, 63.95113791807857950 ) ) ;
#18746 = ADVANCED_FACE ( 'NONE', ( #17627 ), #22392, .T. ) ;
#18747 = CARTESIAN_POINT ( 'NONE',  ( 0.05014649552810506589, 217.5146222423826714, 28.25113791807856245 ) ) ;
#18748 = DIRECTION ( 'NONE',  ( 0.000000000000000000, 0.000000000000000000, 1.000000000000000000 ) ) ;
#18749 = CARTESIAN_POINT ( 'NONE',  ( -7.500000000000000888, -3.608439182435167591, -7.298562697733108173 ) ) ;
#18750 = CARTESIAN_POINT ( 'NONE',  ( 6.139770520408223575, 215.5359834540460611, 9.548862081921432932 ) ) ;
#18751 = CONICAL_SURFACE ( 'NONE', #4049, 32.10452846326766974, 1.466076571675243301 ) ;
#18752 = CARTESIAN_POINT ( 'NONE',  ( 63.19999999453762740, 146.4771138417591203, 11.73074641843673227 ) ) ;
#18753 = ORIENTED_EDGE ( 'NONE', *, *, #19495, .F. ) ;
#18754 = CARTESIAN_POINT ( 'NONE',  ( -0.05014649552807705357, 194.3824533091408000, 38.75113791807856245 ) ) ;
#18755 = ADVANCED_FACE ( 'NONE', ( #7241 ), #12854, .T. ) ;
#18756 = DIRECTION ( 'NONE',  ( 0.000000000000000000, 0.7071067811865475727, 0.7071067811865475727 ) ) ;
#18757 = CARTESIAN_POINT ( 'NONE',  ( 10.01549611932659545, 203.7984951890123853, 19.14886208192142902 ) ) ;
#18758 = CARTESIAN_POINT ( 'NONE',  ( 58.91132485994280898, 146.1832212156128890, 12.13525491562421976 ) ) ;
#18759 = VERTEX_POINT ( 'NONE', #29024 ) ;
#18760 = CARTESIAN_POINT ( 'NONE',  ( -8.062137200540920645, 212.9164362838581894, 81.80113791807858092 ) ) ;
#18761 = EDGE_CURVE ( 'NONE', #15312, #20612, #30867, .T. ) ;
#18762 = ORIENTED_EDGE ( 'NONE', *, *, #24061, .F. ) ;
#18763 = FACE_OUTER_BOUND ( 'NONE', #16534, .T. ) ;
#18764 = CARTESIAN_POINT ( 'NONE',  ( 32.50000000000000000, 155.0000000000000000, 15.00000000000001243 ) ) ;
#18765 = ORIENTED_EDGE ( 'NONE', *, *, #16047, .T. ) ;
#18766 = CARTESIAN_POINT ( 'NONE',  ( -8.015496119326531499, 204.4483345814780364, 15.35113791807856387 ) ) ;
#18767 = LINE ( 'NONE', #3762, #16144 ) ;
#18768 = CARTESIAN_POINT ( 'NONE',  ( 9.680171189290716072, 214.0920067884432854, 99.69886208192144750 ) ) ;
#18769 = CARTESIAN_POINT ( 'NONE',  ( 44.17499999726881299, 164.1591823560292198, 12.60653300113718167 ) ) ;
#18770 = ORIENTED_EDGE ( 'NONE', *, *, #30829, .T. ) ;
#18771 = CARTESIAN_POINT ( 'NONE',  ( 50.12499999726881583, 155.0000000000000000, 15.58253174999999402 ) ) ;
#18772 = DIRECTION ( 'NONE',  ( 1.000000000000000000, 0.000000000000000000, 0.000000000000000000 ) ) ;
#18773 = DIRECTION ( 'NONE',  ( 0.000000000000000000, 0.000000000000000000, 1.000000000000000000 ) ) ;
#18774 = CARTESIAN_POINT ( 'NONE',  ( -10.01549611932659722, 210.2015048109875011, 77.64886208192143613 ) ) ;
#18775 = CARTESIAN_POINT ( 'NONE',  ( 53.17499999726881299, 145.8408176439707802, -12.60653300113719588 ) ) ;
#18776 = CARTESIAN_POINT ( 'NONE',  ( 3.044812012440130555, 197.4746971517856764, 23.60113791807857098 ) ) ;
#18777 = CARTESIAN_POINT ( 'NONE',  ( 33.78867513459482552, 155.0000000000000000, 15.00000000000001243 ) ) ;
#18778 = CARTESIAN_POINT ( 'NONE',  ( 75.89999999999999147, 141.2096805137202580, 4.480746418436733158 ) ) ;
#18779 = CARTESIAN_POINT ( 'NONE',  ( 105.0134430565187387, 155.0000000000000000, -31.00000000000000000 ) ) ;
#18780 = DIRECTION ( 'NONE',  ( 1.000000000000000000, 0.000000000000000000, 0.000000000000000000 ) ) ;
#18781 = CARTESIAN_POINT ( 'NONE',  ( -3.135527875058821579, 197.5041725223112223, 83.90113791807857524 ) ) ;
#18782 = DIRECTION ( 'NONE',  ( 1.000000000000000000, 0.000000000000000000, 0.000000000000000000 ) ) ;
#18783 = CARTESIAN_POINT ( 'NONE',  ( 37.17499999726881299, 145.8408176439707802, -12.60653300113719588 ) ) ;
#18784 = CARTESIAN_POINT ( 'NONE',  ( 3.662846001189864698, 218.4274158808046593, 99.39886208192146455 ) ) ;
#18785 = APPLICATION_CONTEXT ( 'automotive_design' ) ;
#18786 = CARTESIAN_POINT ( 'NONE',  ( 77.82499999726880446, 168.2552932293087906, 9.630534252274372875 ) ) ;
#18787 = VERTEX_POINT ( 'NONE', #31258 ) ;
#18788 = CARTESIAN_POINT ( 'NONE',  ( 127.5000000000000000, 155.0000000000000000, 98.00000000000002842 ) ) ;
#18789 = CARTESIAN_POINT ( 'NONE',  ( 43.39999999453763024, 141.2096805137202580, 4.480746418436733158 ) ) ;
#18790 = FACE_OUTER_BOUND ( 'NONE', #21141, .T. ) ;
#18791 = CARTESIAN_POINT ( 'NONE',  ( -0.6169862416623524970, -8.783631307150855605, -7.913704048099795330 ) ) ;
#18792 = ORIENTED_EDGE ( 'NONE', *, *, #27006, .T. ) ;
#18793 = CARTESIAN_POINT ( 'NONE',  ( -10.01549611932659545, 210.2015048109875011, 92.64886208192143613 ) ) ;
#18794 = CARTESIAN_POINT ( 'NONE',  ( -9.680171189290716072, 199.9079932115567146, 29.19886208192143684 ) ) ;
#18795 = FACE_OUTER_BOUND ( 'NONE', #6699, .T. ) ;
#18796 = CARTESIAN_POINT ( 'NONE',  ( 8.062137200540920645, 201.0835637161417822, 50.30113791807857382 ) ) ;
#18797 = VERTEX_POINT ( 'NONE', #575 ) ;
#18798 = CARTESIAN_POINT ( 'NONE',  ( 4.984841277089891776, 200.2242689037093726, 7.448862081921436840 ) ) ;
#18799 = DIRECTION ( 'NONE',  ( -1.000000000000000000, -0.000000000000000000, -0.000000000000000000 ) ) ;
#18800 = EDGE_LOOP ( 'NONE', ( #8418, #20004, #2973, #15456 ) ) ;
#18801 = CARTESIAN_POINT ( 'NONE',  ( -2.426778023690076225, 199.3768101843759553, 85.89886208192143613 ) ) ;
#18802 = CARTESIAN_POINT ( 'NONE',  ( 6.444103211791042618, 202.2591342207267644, 29.30113791807857027 ) ) ;
#18803 = CARTESIAN_POINT ( 'NONE',  ( 127.5000000000000000, 155.0000000000000000, -6.938893903907228378E-15 ) ) ;
#18804 = ORIENTED_EDGE ( 'NONE', *, *, #21851, .F. ) ;
#18805 = CARTESIAN_POINT ( 'NONE',  ( 90.49452189536829394, 155.0000000000000000, -32.10452846326766974 ) ) ;
#18806 = CARTESIAN_POINT ( 'NONE',  ( 37.17499999726881299, 145.8408176439707802, -12.60653300113719588 ) ) ;
#18807 = CARTESIAN_POINT ( 'NONE',  ( 77.50000000000000000, 155.0000000000000000, -6.938893903907228378E-15 ) ) ;
#18808 = CARTESIAN_POINT ( 'NONE',  ( 2.517493886308900919, 214.5937144450984420, 100.4011379180785895 ) ) ;
#18809 = DIRECTION ( 'NONE',  ( 0.9999999999999998890, 0.000000000000000000, 0.000000000000000000 ) ) ;
#18810 = CARTESIAN_POINT ( 'NONE',  ( 56.70000000000000284, 163.5228861582408797, -11.73074641843674470 ) ) ;
#18811 = CARTESIAN_POINT ( 'NONE',  ( 4.903702542908435547, 213.8346818373419751, 69.54886208192141339 ) ) ;
#18812 = FACE_OUTER_BOUND ( 'NONE', #1194, .T. ) ;
#18813 = CARTESIAN_POINT ( 'NONE',  ( 56.32499999726881157, 145.8408176439707802, 12.60653300113718345 ) ) ;
#18815 = ORIENTED_EDGE ( 'NONE', *, *, #14682, .T. ) ;
#18814 = CARTESIAN_POINT ( 'NONE',  ( -10.01549611932653860, 203.7984951890123000, 12.35113791807856387 ) ) ;
#18816 = CARTESIAN_POINT ( 'NONE',  ( 58.50000000000001421, -88.00000000000000000, -20.00000000000000000 ) ) ;
#18817 = CARTESIAN_POINT ( 'NONE',  ( 61.72499999726881015, 169.8198683612136222, 4.815267126137181997 ) ) ;
#18818 = CARTESIAN_POINT ( 'NONE',  ( 74.27499999726880731, 160.0630714827496206, 15.58253174999999402 ) ) ;
#18819 = CARTESIAN_POINT ( 'NONE',  ( 7.456977232089302632, 217.1783343296989131, 76.55113791807858092 ) ) ;
#18820 = CARTESIAN_POINT ( 'NONE',  ( 15.61000000000001364, 0.000000000000000000, 2.000000000000000888 ) ) ;
#18821 = CARTESIAN_POINT ( 'NONE',  ( 9.984503880673473830, 203.7031108863295401, 98.15113791807858945 ) ) ;
#18822 = FACE_OUTER_BOUND ( 'NONE', #20107, .T. ) ;
#18823 = AXIS2_PLACEMENT_3D ( 'NONE', #4881, #20044, #28046 ) ;
#18824 = EDGE_LOOP ( 'NONE', ( #13434, #283, #17330, #27582 ) ) ;
#18825 = CARTESIAN_POINT ( 'NONE',  ( 12.00000000000000711, 207.0476921513415220, 63.99886208192143044 ) ) ;
#18826 = CARTESIAN_POINT ( 'NONE',  ( 3.044812012439969795, 216.5253028482143520, 66.39886208192143613 ) ) ;
#18827 = CARTESIAN_POINT ( 'NONE',  ( -11.89830997168683702, 232.6342992855866783, 103.4854814124441447 ) ) ;
#18828 = CARTESIAN_POINT ( 'NONE',  ( 127.5000000000000000, 81.56696077377658582, -76.47359838532473475 ) ) ;
#18829 = CARTESIAN_POINT ( 'NONE',  ( 10.01549611932653860, 210.2015048109876716, 22.85113791807856742 ) ) ;
#18830 = CARTESIAN_POINT ( 'NONE',  ( -6.139770520408224463, 198.4640165459539389, 83.04886208192144181 ) ) ;
#18831 = EDGE_CURVE ( 'NONE', #5170, #10719, #3129, .T. ) ;
#18832 = EDGE_LOOP ( 'NONE', ( #11591, #26990, #8889, #7411 ) ) ;
#18833 = CARTESIAN_POINT ( 'NONE',  ( 6.837824896291514243, -3.947820044545437224, -6.564402953523717166 ) ) ;
#18834 = ORIENTED_EDGE ( 'NONE', *, *, #25804, .T. ) ;
#18835 = DIRECTION ( 'NONE',  ( 1.000000000000000000, -0.000000000000000000, -0.000000000000000000 ) ) ;
#18836 = CARTESIAN_POINT ( 'NONE',  ( -0.05014649552828365914, 215.4116977939061144, 57.24886208192145887 ) ) ;
#18837 = ORIENTED_EDGE ( 'NONE', *, *, #28058, .T. ) ;
#18838 = CARTESIAN_POINT ( 'NONE',  ( 77.12499999726881583, 155.0000000000000000, -15.58253175000000823 ) ) ;
#18839 = ORIENTED_EDGE ( 'NONE', *, *, #1445, .T. ) ;
#18840 = CARTESIAN_POINT ( 'NONE',  ( 89.50000000000002842, 155.0000000000000000, 32.00000000000002842 ) ) ;
#18841 = B_SPLINE_CURVE_WITH_KNOTS ( 'NONE', 3,
 ( #16834, #29623, #32165, #6454, #31672, #8341 ),
 .UNSPECIFIED., .F., .F.,
 ( 4, 2, 4 ),
 ( 0.000000000000000000, 0.0004189869898914152461, 0.0008379739797828304922 ),
 .UNSPECIFIED. ) ;
#18842 = UNCERTAINTY_MEASURE_WITH_UNIT (LENGTH_MEASURE( 1.000000000000000082E-05 ), #10239, 'distance_accuracy_value', 'NONE');
#18843 = CARTESIAN_POINT ( 'NONE',  ( 71.02499999726882152, 149.9369285172503510, -15.58253175000000823 ) ) ;
#18844 = CARTESIAN_POINT ( 'NONE',  ( 0.05014649552807626948, 215.4116977939061144, 73.25113791807858377 ) ) ;
#18845 = CIRCLE ( 'NONE', #29717, 6.999999999999950262 ) ;
#18846 = DIRECTION ( 'NONE',  ( 1.000000000000000000, 0.000000000000000000, 0.000000000000000000 ) ) ;
#18847 = CIRCLE ( 'NONE', #8514, 32.10452846326764131 ) ;
#18848 = CARTESIAN_POINT ( 'NONE',  ( 8.000000000000008882, 207.0476921513415220, 48.99886208192144466 ) ) ;
#18849 = CARTESIAN_POINT ( 'NONE',  ( 3.044812012440130555, 197.4746971517856764, 77.60113791807857808 ) ) ;
#18850 = CARTESIAN_POINT ( 'NONE',  ( -10.00000000000000711, 207.0476921513413515, 69.50113791807856956 ) ) ;
#18851 = CIRCLE ( 'NONE', #25375, 2.150000000000004352 ) ;
#18852 = FACE_OUTER_BOUND ( 'NONE', #15464, .T. ) ;
#18853 = CARTESIAN_POINT ( 'NONE',  ( -8.015496119326531499, 204.4483345814780364, 21.35113791807856742 ) ) ;
#18854 = CARTESIAN_POINT ( 'NONE',  ( 0.5984201754795568373, 8.314755988442765755, -0.7022220667781353676 ) ) ;
#18855 = DIRECTION ( 'NONE',  ( 1.000000000000000000, -0.000000000000000000, -0.000000000000000000 ) ) ;
#18856 = CARTESIAN_POINT ( 'NONE',  ( 46.42499999726881299, 141.7447067706911810, 9.630534252274376428 ) ) ;
#18857 = CARTESIAN_POINT ( 'NONE',  ( 3.753561863808689836, 218.3979405102790565, 49.40113791807856813 ) ) ;
#18858 = CARTESIAN_POINT ( 'NONE',  ( 7.922798488042200660, -4.627419312545550056, -8.057411459260041653 ) ) ;
#18859 = CARTESIAN_POINT ( 'NONE',  ( -0.05014649552810635652, 196.4853777576173002, 92.75113791807858377 ) ) ;
#18860 = CARTESIAN_POINT ( 'NONE',  ( -3.044812012440131443, 216.5253028482142952, 70.10113791807857808 ) ) ;
#18861 = CARTESIAN_POINT ( 'NONE',  ( 7.456977232089471386, 196.8216656703012006, 31.44886208192143684 ) ) ;
#18862 = CARTESIAN_POINT ( 'NONE',  ( -3.044812012439970683, 197.4746971517856196, 34.89886208192143613 ) ) ;
#18863 = CARTESIAN_POINT ( 'NONE',  ( 82.09999999453762598, 159.7113355953771077, -14.50000000000000888 ) ) ;
#18864 = CARTESIAN_POINT ( 'NONE',  ( 9.680171189290831535, 199.9079932115568852, 74.30113791807858092 ) ) ;
#18865 = CARTESIAN_POINT ( 'NONE',  ( -8.000000000000008882, 207.0476921513413515, 90.50113791807858377 ) ) ;
#18866 = CARTESIAN_POINT ( 'NONE',  ( 10.00000000000000711, 207.0476921513415220, 45.99886208192143755 ) ) ;
#18867 = EDGE_CURVE ( 'NONE', #26329, #26980, #32288, .T. ) ;
#18868 = CONICAL_SURFACE ( 'NONE', #4179, 12.00000000000001066, 0.1047197551196464710 ) ;
#18869 = FACE_BOUND ( 'NONE', #19387, .T. ) ;
#18870 = VERTEX_POINT ( 'NONE', #15410 ) ;
#18871 = CARTESIAN_POINT ( 'NONE',  ( 3.662846001189864698, 218.4274158808046593, 66.39886208192143613 ) ) ;
#18872 = AXIS2_PLACEMENT_3D ( 'NONE', #22491, #4608, #32535 ) ;
#18873 = ORIENTED_EDGE ( 'NONE', *, *, #29067, .F. ) ;
#18874 = CARTESIAN_POINT ( 'NONE',  ( 4.984841277089891776, 200.2242689037093726, 34.44886208192144039 ) ) ;
#18875 = ADVANCED_FACE ( 'NONE', ( #28858 ), #18635, .F. ) ;
#18876 = VERTEX_POINT ( 'NONE', #10319 ) ;
#18877 = AXIS2_PLACEMENT_3D ( 'NONE', #27009, #29737, #24630 ) ;
#18878 = CARTESIAN_POINT ( 'NONE',  ( 77.57499999726881867, 164.1591823560292198, -12.60653300113719766 ) ) ;
#18879 = CARTESIAN_POINT ( 'NONE',  ( 53.41132485994281609, 142.2402378747194405, -9.270509831248439525 ) ) ;
#18880 = EDGE_CURVE ( 'NONE', #33504, #14265, #6167, .T. ) ;
#18881 = CARTESIAN_POINT ( 'NONE',  ( 115.4999999999999858, 127.5651812191323557, -102.3881375866411645 ) ) ;
#18882 = CARTESIAN_POINT ( 'NONE',  ( 6.500168698208129925, 211.6636982574063381, 52.70113791807857240 ) ) ;
#18883 = CARTESIAN_POINT ( 'NONE',  ( 3.499999999999993339, -2.020725942163723143, -2.587392608830344720 ) ) ;
#18884 = CARTESIAN_POINT ( 'NONE',  ( -6.139770520408224463, 198.4640165459539389, 35.04886208192144181 ) ) ;
#18885 = CARTESIAN_POINT ( 'NONE',  ( 69.17499999726881299, 145.8408176439707802, -12.60653300113719588 ) ) ;
#18886 = ORIENTED_EDGE ( 'NONE', *, *, #24347, .T. ) ;
#18887 = DIRECTION ( 'NONE',  ( 1.000000000000000000, 0.000000000000000000, 0.000000000000000000 ) ) ;
#18888 = CARTESIAN_POINT ( 'NONE',  ( -6.444103211790928043, 202.2591342207265939, 20.19886208192143684 ) ) ;
#18889 = VECTOR ( 'NONE', #20450, 1000.000000000000114 ) ;
#18890 = CARTESIAN_POINT ( 'NONE',  ( -10.00000000000000711, 207.0476921513413515, 51.50113791807857666 ) ) ;
#18891 = EDGE_CURVE ( 'NONE', #2299, #576, #16071, .T. ) ;
#18892 = CARTESIAN_POINT ( 'NONE',  ( 10.01549611932653860, 210.2015048109876716, 34.85113791807856387 ) ) ;
#18893 = CARTESIAN_POINT ( 'NONE',  ( 84.97499999726882436, 140.1801316387863778, -4.815267126137194431 ) ) ;
#18894 = APPLICATION_PROTOCOL_DEFINITION ( 'draft international standard', 'automotive_design', 1998, #2018 ) ;
#18895 = VECTOR ( 'NONE', #19992, 1000.000000000000227 ) ;
#18896 = CARTESIAN_POINT ( 'NONE',  ( 6.444103211790928043, 211.7408657792734061, 93.69886208192144750 ) ) ;
#18897 = CARTESIAN_POINT ( 'NONE',  ( 36.92499999726880588, 145.8408176439707802, -12.60653300113719588 ) ) ;
#18898 = CARTESIAN_POINT ( 'NONE',  ( 81.28867513459482552, 170.7719333635740497, -7.904646289410545231E-15 ) ) ;
#18899 = DIRECTION ( 'NONE',  ( 1.000000000000000000, 0.000000000000000000, 0.000000000000000000 ) ) ;
#18900 = CARTESIAN_POINT ( 'NONE',  ( -12.00000000000000711, 207.0476921513413515, 15.50113791807856600 ) ) ;
#18901 = CARTESIAN_POINT ( 'NONE',  ( 4.599534470797546959, -6.460478697736932396, -7.590212325761396706 ) ) ;
#18902 = CARTESIAN_POINT ( 'NONE',  ( 59.77499999726881441, 169.8198683612136222, -4.815267126137197984 ) ) ;
#18903 = ADVANCED_FACE ( 'NONE', ( #18475, #26461 ), #25807, .T. ) ;
#18904 = CARTESIAN_POINT ( 'NONE',  ( 6.139770520408368348, 198.4640165459539674, 68.45113791807858661 ) ) ;
#18905 = CARTESIAN_POINT ( 'NONE',  ( 10.01549611932653860, 210.2015048109876716, 37.85113791807856387 ) ) ;
#18906 = CIRCLE ( 'NONE', #28714, 2.149999999999979483 ) ;
#18907 = CARTESIAN_POINT ( 'NONE',  ( -7.500000000000000000, -3.988190556646204588, -0.8526458641284329065 ) ) ;
#18908 = DIRECTION ( 'NONE',  ( 1.000000000000000000, 0.000000000000000000, 0.000000000000000000 ) ) ;
#18909 = CARTESIAN_POINT ( 'NONE',  ( 6.139770520408223575, 215.5359834540460611, 6.548862081921434708 ) ) ;
#18910 = CARTESIAN_POINT ( 'NONE',  ( 58.49999999453762456, 170.2462022514548323, -7.872454543227099337E-15 ) ) ;
#18911 = VERTEX_POINT ( 'NONE', #31092 ) ;
#18912 = CARTESIAN_POINT ( 'NONE',  ( 11.98450388067348271, 203.0532714938637753, 44.15113791807856813 ) ) ;
#18913 = CARTESIAN_POINT ( 'NONE',  ( 77.21132485994282035, 139.2280666364260071, -4.041636747397287284E-15 ) ) ;
#18914 = CARTESIAN_POINT ( 'NONE',  ( -10.00000000000000711, 206.9523078486584495, 23.49886208192143755 ) ) ;
#18915 = CARTESIAN_POINT ( 'NONE',  ( 59.21132485994281325, 139.2280666364260071, -4.041636747397287284E-15 ) ) ;
#18916 = ORIENTED_EDGE ( 'NONE', *, *, #17671, .T. ) ;
#18917 = CARTESIAN_POINT ( 'NONE',  ( -3.135527875058821579, 197.5041725223112223, 77.90113791807857524 ) ) ;
#18918 = AXIS2_PLACEMENT_3D ( 'NONE', #19888, #11725, #32333 ) ;
#18919 = ORIENTED_EDGE ( 'NONE', *, *, #13689, .F. ) ;
#18920 = AXIS2_PLACEMENT_3D ( 'NONE', #27585, #4603, #19923 ) ;
#18921 = DIRECTION ( 'NONE',  ( 1.000000000000000000, 0.000000000000000000, 0.000000000000000000 ) ) ;
#18922 = VECTOR ( 'NONE', #32123, 1000.000000000000000 ) ;
#18923 = CARTESIAN_POINT ( 'NONE',  ( 0.2813450144774466422, -7.667988119308859041, -6.122077150241856280 ) ) ;
#18924 = ORIENTED_EDGE ( 'NONE', *, *, #30201, .T. ) ;
#18925 = CARTESIAN_POINT ( 'NONE',  ( -8.000000000000008882, 207.0476921513413515, 24.50113791807856600 ) ) ;
#18926 = ADVANCED_FACE ( 'NONE', ( #7751 ), #18139, .T. ) ;
#18927 = CARTESIAN_POINT ( 'NONE',  ( -60.91988776943159678, 194.9950600780878460, 0.6490123436103525378 ) ) ;
#18928 = CARTESIAN_POINT ( 'NONE',  ( -10.00000000000000711, 206.9523078486584495, 2.498862081921433997 ) ) ;
#18929 = CARTESIAN_POINT ( 'NONE',  ( 47.17499999726881299, 145.8408176439707802, -12.60653300113719588 ) ) ;
#18931 = EDGE_LOOP ( 'NONE', ( #29514, #8003, #19170, #10677 ) ) ;
#18930 = VECTOR ( 'NONE', #25065, 1000.000000000000000 ) ;
#18932 = CARTESIAN_POINT ( 'NONE',  ( 60.22499999726881725, 149.9369285172503510, 15.58253174999999580 ) ) ;
#18933 = CARTESIAN_POINT ( 'NONE',  ( -125.0000000000000000, 25.00000000000000000, 35.00000000000000000 ) ) ;
#18934 = DIRECTION ( 'NONE',  ( 1.000000000000000000, -0.000000000000000000, -0.000000000000000000 ) ) ;
#18935 = CYLINDRICAL_SURFACE ( 'NONE', #17344, 32.00000000000001421 ) ;
#18936 = CARTESIAN_POINT ( 'NONE',  ( 6.139770520408223575, 215.5359834540460611, 90.54886208192144181 ) ) ;
#18937 = CARTESIAN_POINT ( 'NONE',  ( 54.77499999726881441, 140.1801316387863778, 4.815267126137185549 ) ) ;
#18938 = CARTESIAN_POINT ( 'NONE',  ( -10.01549611932653860, 203.7984951890123284, 21.35113791807855677 ) ) ;
#18939 = CARTESIAN_POINT ( 'NONE',  ( 119.7500000000000000, 3.125910954823619074E-14, -35.00000000000000000 ) ) ;
#18940 = ADVANCED_FACE ( 'NONE', ( #10970 ), #29569, .F. ) ;
#18941 = CARTESIAN_POINT ( 'NONE',  ( 12.01549611932659367, 203.1486557965466773, 82.14886208192143613 ) ) ;
#18942 = CARTESIAN_POINT ( 'NONE',  ( 72.50000000000001421, 155.0000000000000000, -14.50000000000000711 ) ) ;
#18943 = LINE ( 'NONE', #19278, #14900 ) ;
#18944 = CARTESIAN_POINT ( 'NONE',  ( -5.357619327558936585E-16, 7.505553499465137612, -6.064240316920400886 ) ) ;
#18945 = CARTESIAN_POINT ( 'NONE',  ( 10.00000000000000711, 206.9523078486586201, 98.00113791807856956 ) ) ;
#18946 = AXIS2_PLACEMENT_3D ( 'NONE', #28699, #18479, #29368 ) ;
#18947 = CARTESIAN_POINT ( 'NONE',  ( 0.000000000000000000, 0.000000000000000000, -2.629527361626598836 ) ) ;
#18948 = CARTESIAN_POINT ( 'NONE',  ( 37.27499999726880020, 149.9369285172503510, -15.58253175000000823 ) ) ;
#18949 = EDGE_CURVE ( 'NONE', #22604, #25621, #18265, .T. ) ;
#18950 = CARTESIAN_POINT ( 'NONE',  ( 3.135527875058820690, 216.4958274776887492, 40.40113791807857524 ) ) ;
#18951 = CIRCLE ( 'NONE', #3716, 7.499999999999992895 ) ;
#18952 = CARTESIAN_POINT ( 'NONE',  ( 74.32499999726881867, 145.8408176439707802, 12.60653300113718345 ) ) ;
#18953 = ORIENTED_EDGE ( 'NONE', *, *, #24172, .T. ) ;
#18954 = CARTESIAN_POINT ( 'NONE',  ( 117.5000000000000000, 52.61186241335891367, 27.43481878086798176 ) ) ;
#18955 = CARTESIAN_POINT ( 'NONE',  ( 44.09999999453762598, 159.7113355953771077, -14.50000000000000888 ) ) ;
#18956 = CARTESIAN_POINT ( 'NONE',  ( 3.753561863808689836, 218.3979405102790565, 22.40113791807856813 ) ) ;
#18957 = CYLINDRICAL_SURFACE ( 'NONE', #8317, 24.99999999999999289 ) ;
#18958 = VECTOR ( 'NONE', #20928, 1000.000000000000000 ) ;
#18959 = CARTESIAN_POINT ( 'NONE',  ( 6.250000000000000000, -5.051814855409237026, -7.198902722707430257 ) ) ;
#18960 = VERTEX_POINT ( 'NONE', #21021 ) ;
#18961 = CARTESIAN_POINT ( 'NONE',  ( -10.00000000000000711, 206.9523078486584495, 98.49886208192143044 ) ) ;
#18962 = CARTESIAN_POINT ( 'NONE',  ( 7.456977232089471386, 196.8216656703012006, 37.44886208192143329 ) ) ;
#18963 = CARTESIAN_POINT ( 'NONE',  ( -9.996365641501871124, 207.8097375604742467, 102.5363179372327096 ) ) ;
#18964 = CARTESIAN_POINT ( 'NONE',  ( -9.984503880673473830, 210.2968891136704315, 48.65113791807858235 ) ) ;
#18965 = ORIENTED_EDGE ( 'NONE', *, *, #17100, .F. ) ;
#18966 = CARTESIAN_POINT ( 'NONE',  ( 0.05014649552828262524, 198.5883022060938572, 13.74886208192143577 ) ) ;
#18967 = CARTESIAN_POINT ( 'NONE',  ( 51.61132485994281893, 150.1262045565065364, -15.00000000000012434 ) ) ;
#18968 = ORIENTED_EDGE ( 'NONE', *, *, #15157, .F. ) ;
#18969 = CARTESIAN_POINT ( 'NONE',  ( 4.903702542908435547, 213.8346818373419751, 99.54886208192144181 ) ) ;
#18970 = VECTOR ( 'NONE', #29087, 999.9999999999998863 ) ;
#18971 = EDGE_CURVE ( 'NONE', #7638, #18870, #14349, .T. ) ;
#18972 = AXIS2_PLACEMENT_3D ( 'NONE', #23788, #24277, #29404 ) ;
#18973 = CARTESIAN_POINT ( 'NONE',  ( 2.517493886308900919, 214.5937144450984420, 37.40113791807856813 ) ) ;
#18974 = DIRECTION ( 'NONE',  ( 1.000000000000000000, 0.000000000000000000, 0.000000000000000000 ) ) ;
#18975 = ORIENTED_EDGE ( 'NONE', *, *, #27929, .F. ) ;
#18976 = CARTESIAN_POINT ( 'NONE',  ( 1.013163106016871096, 8.075304045852551127, -7.231838333420561149 ) ) ;
#18977 = CIRCLE ( 'NONE', #10819, 0.7733184030943203169 ) ;
#18979 = EDGE_CURVE ( 'NONE', #31209, #32913, #8906, .T. ) ;
#18978 = CARTESIAN_POINT ( 'NONE',  ( -6.139770520408224463, 198.4640165459539389, 56.04886208192142050 ) ) ;
#18981 = CARTESIAN_POINT ( 'NONE',  ( 87.82499999726881867, 168.2552932293087906, 9.630534252274372875 ) ) ;
#18980 = PRODUCT_DEFINITION ( 'UNKNOWN', '', #11028, #29865 ) ;
#18982 = CARTESIAN_POINT ( 'NONE',  ( 8.015496119326531499, 209.5516654185219636, 100.8511379180785781 ) ) ;
#18983 = EDGE_CURVE ( 'NONE', #7152, #8990, #17867, .T. ) ;
#18984 = AXIS2_PLACEMENT_3D ( 'NONE', #33418, #30187, #2244 ) ;
#18985 = DIRECTION ( 'NONE',  ( 6.123233995736766036E-17, 0.000000000000000000, 1.000000000000000000 ) ) ;
#18986 = CARTESIAN_POINT ( 'NONE',  ( 53.50000000000000711, 155.0000000000000000, 14.49999999999999467 ) ) ;
#18987 = CARTESIAN_POINT ( 'NONE',  ( 2.426778023690075337, 214.6231898156240447, 72.39886208192143613 ) ) ;
#18988 = CARTESIAN_POINT ( 'NONE',  ( 77.08867513459483689, 167.7597621252805880, -9.270509831248443078 ) ) ;
#18989 = CARTESIAN_POINT ( 'NONE',  ( 56.22499999726881015, 149.9369285172503510, 15.58253174999999580 ) ) ;
#18990 = CARTESIAN_POINT ( 'NONE',  ( -10.01549611932653860, 203.7984951890123000, 6.351137918078565647 ) ) ;
#18991 = DIRECTION ( 'NONE',  ( -1.000000000000000000, -0.000000000000000000, -0.000000000000000000 ) ) ;
#18992 = CARTESIAN_POINT ( 'NONE',  ( 63.32499999726881867, 164.1591823560292198, -12.60653300113719766 ) ) ;
#18993 = CARTESIAN_POINT ( 'NONE',  ( 73.67499999726878457, 168.2552932293087906, -9.630534252274385310 ) ) ;
#18994 = CARTESIAN_POINT ( 'NONE',  ( -7.375838497908182134, 217.2372850707499765, 72.95113791807857240 ) ) ;
#18995 = AXIS2_PLACEMENT_3D ( 'NONE', #26156, #23605, #23100 ) ;
#18996 = CARTESIAN_POINT ( 'NONE',  ( 8.062137200540920645, 201.0835637161417822, 95.30113791807858092 ) ) ;
#18997 = CARTESIAN_POINT ( 'NONE',  ( 2.000000000000000000, 0.000000000000000000, 1.535500000000000087 ) ) ;
#18998 = ORIENTED_EDGE ( 'NONE', *, *, #30971, .T. ) ;
#18999 = CARTESIAN_POINT ( 'NONE',  ( 3.662846001189864698, 218.4274158808046593, 102.3988620819214361 ) ) ;
#19000 = CARTESIAN_POINT ( 'NONE',  ( -12.01549611932659722, 210.8513442034533227, 59.64886208192143613 ) ) ;
#19001 = CARTESIAN_POINT ( 'NONE',  ( 3.135527875058981895, 197.5041725223112792, 64.59886208192143897 ) ) ;
#19002 = CARTESIAN_POINT ( 'NONE',  ( 7.375838497908012492, 217.2372850707501186, 3.548862081921434264 ) ) ;
#19003 = FACE_OUTER_BOUND ( 'NONE', #12941, .T. ) ;
#19004 = CARTESIAN_POINT ( 'NONE',  ( 10.00000000000000711, 206.9523078486586201, 20.00113791807856600 ) ) ;
#19005 = CARTESIAN_POINT ( 'NONE',  ( -0.05014649552828403384, 217.5146222423826714, 90.24886208192141623 ) ) ;
#19006 = ORIENTED_EDGE ( 'NONE', *, *, #8945, .F. ) ;
#19007 = DIRECTION ( 'NONE',  ( -0.9891821073486152249, -0.1466927349985428231, 0.000000000000000000 ) ) ;
#19008 = EDGE_LOOP ( 'NONE', ( #17089, #11381, #29433, #21022 ) ) ;
#19009 =( NAMED_UNIT ( * ) SI_UNIT ( $, .STERADIAN. ) SOLID_ANGLE_UNIT ( ) );
#19010 =( BOUNDED_CURVE ( )  B_SPLINE_CURVE ( 2, ( #8766, #23938, #29552, #6550, #14390, #27329, #16933, #19497, #3993, #24782, #1437 ),
 .UNSPECIFIED., .F., .T. ) 
 B_SPLINE_CURVE_WITH_KNOTS ( ( 3, 2, 2, 2, 2, 3 ),
 ( 0.6071428571428568732, 0.6107142857142854320, 0.6142857142857139907, 0.6178571428571425495, 0.6214285714285711082, 0.6249999999999996669 ),
 .UNSPECIFIED. ) 
 CURVE ( )  GEOMETRIC_REPRESENTATION_ITEM ( )  RATIONAL_B_SPLINE_CURVE ( ( 1.000000000000003109, 0.9510565162951504226, 1.000000000000000000, 0.9510565162951534202, 1.000000000000000000, 0.9510565162951534202, 1.000000000000000000, 0.9510565162951534202, 1.000000000000000000, 0.9510565162951579721, 0.9999999999999954481 ) ) 
 REPRESENTATION_ITEM ( '' )  );
#19011 = CARTESIAN_POINT ( 'NONE',  ( -6.444103211790928043, 202.2591342207265939, 62.19886208192144750 ) ) ;
#19012 = VERTEX_POINT ( 'NONE', #22188 ) ;
#19013 = CARTESIAN_POINT ( 'NONE',  ( 79.32499999726881867, 164.1591823560292198, -12.60653300113719766 ) ) ;
#19014 = VERTEX_POINT ( 'NONE', #6009 ) ;
#19015 = CARTESIAN_POINT ( 'NONE',  ( 27.50000000000001776, -15.87713240271472870, -2.456200930618646971 ) ) ;
#19016 = AXIS2_PLACEMENT_3D ( 'NONE', #17741, #25912, #20294 ) ;
#19017 = CARTESIAN_POINT ( 'NONE',  ( 69.62499999726883004, 171.3844434931184253, -7.942151717890132712E-15 ) ) ;
#19018 = CARTESIAN_POINT ( 'NONE',  ( 7.984503880673485376, 204.3529502787953902, 68.15113791807856103 ) ) ;
#19019 = CARTESIAN_POINT ( 'NONE',  ( 13.75000000000002487, 23.81569860407205397, 0.000000000000000000 ) ) ;
#19020 = SURFACE_SIDE_STYLE ('',( #6574 ) ) ;
#19021 = CARTESIAN_POINT ( 'NONE',  ( 36.50000000000000711, 155.0000000000000000, -14.50000000000000711 ) ) ;
#19022 = CARTESIAN_POINT ( 'NONE',  ( -6.444103211790928043, 202.2591342207265939, 44.19886208192144750 ) ) ;
#19023 = CARTESIAN_POINT ( 'NONE',  ( -6.220909254589537696, 198.5229672870051161, 81.05113791807856671 ) ) ;
#19024 = CARTESIAN_POINT ( 'NONE',  ( -9.984503880673473830, 210.2968891136704315, 69.65113791807854682 ) ) ;
#19025 = CARTESIAN_POINT ( 'NONE',  ( -10.00000000000000178, 205.7704093527941893, 108.2846756197957490 ) ) ;
#19026 = CARTESIAN_POINT ( 'NONE',  ( 4.903702542908601636, 200.1653181626581102, 20.45113791807856529 ) ) ;
#19027 = DIRECTION ( 'NONE',  ( 1.000000000000000000, 0.000000000000000000, 0.000000000000000000 ) ) ;
#19028 = CARTESIAN_POINT ( 'NONE',  ( 3.500000000000004885, 2.020725942163676070, -2.899999999999999911 ) ) ;
#19029 = CARTESIAN_POINT ( 'NONE',  ( 47.62499999726880162, 171.3844434931184253, -7.942151717890134290E-15 ) ) ;
#19030 = CARTESIAN_POINT ( 'NONE',  ( 3.662846001190051659, 195.5725841191953691, 47.60113791807857808 ) ) ;
#19031 = CARTESIAN_POINT ( 'NONE',  ( -1.472725187932624030E-14, 206.9977241638431167, -6.000000000000014211 ) ) ;
#19032 = CARTESIAN_POINT ( 'NONE',  ( -3.044812012440131443, 216.5253028482142952, 97.10113791807857808 ) ) ;
#19033 = CARTESIAN_POINT ( 'NONE',  ( 3.044812012440130555, 197.4746971517856764, 71.60113791807857808 ) ) ;
#19034 = CARTESIAN_POINT ( 'NONE',  ( 3.753561863808876797, 195.6020594897209719, 34.59886208192143187 ) ) ;
#19035 = CARTESIAN_POINT ( 'NONE',  ( -6.220909254589682469, 215.4770327129947134, 35.94886208192142618 ) ) ;
#19036 = CARTESIAN_POINT ( 'NONE',  ( 88.39999999453762314, 168.7903194862797420, -4.480746418436745593 ) ) ;
#19037 = CARTESIAN_POINT ( 'NONE',  ( -7.456977232089304408, 196.8216656703010301, 78.05113791807858092 ) ) ;
#19038 = CARTESIAN_POINT ( 'NONE',  ( 8.015496119326531499, 209.5516654185219636, 94.85113791807856387 ) ) ;
#19039 = CARTESIAN_POINT ( 'NONE',  ( 3.135527875058981895, 197.5041725223112792, 46.59886208192143187 ) ) ;
#19040 = CARTESIAN_POINT ( 'NONE',  ( 49.28867513459483263, 170.7719333635740497, -7.904646289410545231E-15 ) ) ;
#19041 = ORIENTED_EDGE ( 'NONE', *, *, #4823, .F. ) ;
#19042 = CARTESIAN_POINT ( 'NONE',  ( -7.375838497908014268, 196.7627149292498530, 59.04886208192144181 ) ) ;
#19043 = EDGE_LOOP ( 'NONE', ( #27475, #7157, #23194, #26923, #18815, #11711, #33385 ) ) ;
#19044 = CARTESIAN_POINT ( 'NONE',  ( -4.903702542908436435, 200.1653181626580249, 32.04886208192144181 ) ) ;
#19045 = B_SPLINE_CURVE_WITH_KNOTS ( 'NONE', 3,
 ( #29673, #22005, #11282, #3270, #8395, #14168 ),
 .UNSPECIFIED., .F., .F.,
 ( 4, 2, 4 ),
 ( 0.003981881017442818506, 0.005970145066490139402, 0.007958409115537461165 ),
 .UNSPECIFIED. ) ;
#19046 = ORIENTED_EDGE ( 'NONE', *, *, #9988, .T. ) ;
#19047 = CARTESIAN_POINT ( 'NONE',  ( 76.27499999726879309, 160.0630714827496206, 15.58253174999999224 ) ) ;
#19048 = DIRECTION ( 'NONE',  ( 0.000000000000000000, 0.000000000000000000, 1.000000000000000000 ) ) ;
#19049 = DIRECTION ( 'NONE',  ( -1.000000000000000000, -0.000000000000000000, 0.000000000000000000 ) ) ;
#19050 = CARTESIAN_POINT ( 'NONE',  ( -4.903702542908602524, 213.8346818373418898, 48.95113791807857240 ) ) ;
#19051 = DIRECTION ( 'NONE',  ( -1.000000000000000000, 0.000000000000000000, 0.000000000000000000 ) ) ;
#19052 = CARTESIAN_POINT ( 'NONE',  ( -6.139770520408224463, 198.4640165459539389, 32.04886208192143471 ) ) ;
#19053 = CARTESIAN_POINT ( 'NONE',  ( 67.77499999726880731, 169.8198683612136222, -4.815267126137197984 ) ) ;
#19054 = ORIENTED_EDGE ( 'NONE', *, *, #20368, .F. ) ;
#19055 = CARTESIAN_POINT ( 'NONE',  ( 36.01132485994281041, 167.7597621252805880, -9.270509831248443078 ) ) ;
#19056 = DIRECTION ( 'NONE',  ( 0.000000000000000000, -1.222984857324291014E-15, -1.000000000000000000 ) ) ;
#19057 = DIRECTION ( 'NONE',  ( 1.000000000000000000, 0.000000000000000000, 0.000000000000000000 ) ) ;
#19058 = CARTESIAN_POINT ( 'NONE',  ( -6.444103211790928043, 202.2591342207265939, 17.19886208192143684 ) ) ;
#19059 = CARTESIAN_POINT ( 'NONE',  ( -10.00000000000000711, 207.0476921513413515, 54.50113791807857666 ) ) ;
#19060 = CARTESIAN_POINT ( 'NONE',  ( 83.28867513459483973, 170.7719333635740497, -7.904646289410545231E-15 ) ) ;
#19061 = PRODUCT_DEFINITION_SHAPE ( 'NONE', 'NONE',  #33700 ) ;
#19062 = ADVANCED_FACE ( 'NONE', ( #11639 ), #9245, .T. ) ;
#19063 = CARTESIAN_POINT ( 'NONE',  ( 9.984503880673470277, 203.7031108863295401, 41.15113791807855392 ) ) ;
#19064 = CARTESIAN_POINT ( 'NONE',  ( 84.87499999726881583, 138.6155565068815463, -3.929120461958505118E-15 ) ) ;
#19065 = CARTESIAN_POINT ( 'NONE',  ( -6.444103211790928043, 202.2591342207265939, 104.1988620819214475 ) ) ;
#19066 = CARTESIAN_POINT ( 'NONE',  ( 37.12499999726881583, 155.0000000000000000, -15.58253175000000823 ) ) ;
#19067 = CARTESIAN_POINT ( 'NONE',  ( 54.30000000000001137, -88.00000000000000000, -30.00000000000000000 ) ) ;
#19068 = FACE_OUTER_BOUND ( 'NONE', #33355, .T. ) ;
#19069 = CARTESIAN_POINT ( 'NONE',  ( -12.00000000000000711, 207.0476921513413515, 21.50113791807856956 ) ) ;
#19070 = CARTESIAN_POINT ( 'NONE',  ( -2.133938722758560669, -6.273523403446323421, -0.09463688534107154993 ) ) ;
#19071 = CARTESIAN_POINT ( 'NONE',  ( 64.77499999726882152, 140.1801316387863778, 4.815267126137185549 ) ) ;
#19072 = CARTESIAN_POINT ( 'NONE',  ( 8.062137200540920645, 201.0835637161417822, 65.30113791807858092 ) ) ;
#19073 = CARTESIAN_POINT ( 'NONE',  ( 6.139770520408367460, 198.4640165459539389, 35.45113791807857240 ) ) ;
#19074 = CARTESIAN_POINT ( 'NONE',  ( 64.50000000000000000, -73.00000000000000000, -30.00000000000000000 ) ) ;
#19075 = CARTESIAN_POINT ( 'NONE',  ( -7.500000000000000000, 3.608439182435158710, -7.298562697733104621 ) ) ;
#19076 = CARTESIAN_POINT ( 'NONE',  ( 12.01549611932659367, 203.1486557965466773, 4.148862081921434353 ) ) ;
#19077 = CARTESIAN_POINT ( 'NONE',  ( 3.044812012439969795, 216.5253028482143520, 6.398862081921435241 ) ) ;
#19078 = VECTOR ( 'NONE', #29447, 1000.000000000000000 ) ;
#19079 = CARTESIAN_POINT ( 'NONE',  ( 64.89999999453763735, 159.7113355953771077, 14.49999999999999289 ) ) ;
#19080 = ORIENTED_EDGE ( 'NONE', *, *, #7911, .T. ) ;
#19081 = CARTESIAN_POINT ( 'NONE',  ( 12.01549611932652972, 210.8513442034534933, 43.85113791807856387 ) ) ;
#19082 = CARTESIAN_POINT ( 'NONE',  ( 8.000000000000008882, 206.9523078486586485, 74.00113791807856956 ) ) ;
#19083 = DIRECTION ( 'NONE',  ( 1.000000000000000000, 0.000000000000000000, 0.000000000000000000 ) ) ;
#19084 = CARTESIAN_POINT ( 'NONE',  ( 8.062137200540822946, 212.9164362838583315, 24.69886208192143684 ) ) ;
#19085 = CARTESIAN_POINT ( 'NONE',  ( 71.68867513459484542, 159.8737954434933215, 15.00000000000024336 ) ) ;
#19086 = ORIENTED_EDGE ( 'NONE', *, *, #33029, .T. ) ;
#19087 = CARTESIAN_POINT ( 'NONE',  ( -3.044812012440131443, 216.5253028482142952, 85.10113791807857808 ) ) ;
#19088 = VERTEX_POINT ( 'NONE', #24580 ) ;
#19089 = CYLINDRICAL_SURFACE ( 'NONE', #14566, 2.149999999999974598 ) ;
#19090 = CARTESIAN_POINT ( 'NONE',  ( 2.385244779468109755E-15, 4.041451884327391220, -2.587392608830344720 ) ) ;
#19091 = ORIENTED_EDGE ( 'NONE', *, *, #24061, .T. ) ;
#19092 = CARTESIAN_POINT ( 'NONE',  ( -8.000000000000008882, 207.0476921513413515, 18.50113791807856956 ) ) ;
#19093 = EDGE_CURVE ( 'NONE', #6936, #33266, #21733, .T. ) ;
#19094 = CARTESIAN_POINT ( 'NONE',  ( -59.75243488385262225, 194.9412087183787037, 2.169815710172075196 ) ) ;
#19095 = CARTESIAN_POINT ( 'NONE',  ( 8.062137200540822946, 212.9164362838583315, 6.698862081921435063 ) ) ;
#19096 = CARTESIAN_POINT ( 'NONE',  ( 48.37499999726880873, 155.0000000000000000, 15.58253174999999402 ) ) ;
#19097 = ORIENTED_EDGE ( 'NONE', *, *, #11474, .T. ) ;
#19098 = CARTESIAN_POINT ( 'NONE',  ( 59.12499999726881583, 155.0000000000000000, -15.58253175000000823 ) ) ;
#19099 = LINE ( 'NONE', #8537, #4468 ) ;
#19100 = DIRECTION ( 'NONE',  ( 0.000000000000000000, 0.000000000000000000, 1.000000000000000000 ) ) ;
#19101 = AXIS2_PLACEMENT_3D ( 'NONE', #18529, #3018, #26359 ) ;
#19102 = CARTESIAN_POINT ( 'NONE',  ( 0.000000000000000000, 0.000000000000000000, 0.000000000000000000 ) ) ;
#19103 = CARTESIAN_POINT ( 'NONE',  ( -3.044812012439970683, 197.4746971517856196, 88.89886208192143613 ) ) ;
#19104 = CARTESIAN_POINT ( 'NONE',  ( 62.27499999726880020, 160.0630714827496206, 15.58253174999999402 ) ) ;
#19105 = CARTESIAN_POINT ( 'NONE',  ( -6.220909254589537696, 198.5229672870051161, 27.05113791807856671 ) ) ;
#19106 = CARTESIAN_POINT ( 'NONE',  ( 47.28867513459482552, 170.7719333635740497, -7.904646289410545231E-15 ) ) ;
#19107 = ADVANCED_FACE ( 'NONE', ( #8741 ), #22023, .T. ) ;
#19108 = CARTESIAN_POINT ( 'NONE',  ( 7.375838497908012492, 217.2372850707501186, 81.54886208192144181 ) ) ;
#19109 = CARTESIAN_POINT ( 'NONE',  ( 71.20000000000000284, 167.3344367211045096, 8.961492836873468093 ) ) ;
#19110 = CARTESIAN_POINT ( 'NONE',  ( 2.428571428571428381, 0.000000000000000000, 9.480888224575629408 ) ) ;
#19111 = CARTESIAN_POINT ( 'NONE',  ( -8.118202686958039038, 201.1607312380087080, 96.20113791807857240 ) ) ;
#19112 = CARTESIAN_POINT ( 'NONE',  ( -60.00000000000000000, -7.347880794884118356E-15, -35.00000000000000000 ) ) ;
#19113 = CARTESIAN_POINT ( 'NONE',  ( 45.47499999726881015, 160.0630714827496206, -15.58253175000000823 ) ) ;
#19114 = CARTESIAN_POINT ( 'NONE',  ( -8.118202686958039038, 201.1607312380087080, 36.20113791807857240 ) ) ;
#19115 = CARTESIAN_POINT ( 'NONE',  ( 75.52499999726880731, 169.8198683612136222, -4.815267126137197984 ) ) ;
#19116 = EDGE_CURVE ( 'NONE', #33071, #10396, #20869, .T. ) ;
#19117 = ORIENTED_EDGE ( 'NONE', *, *, #7727, .T. ) ;
#19118 = CARTESIAN_POINT ( 'NONE',  ( 47.71132485994280614, 155.0000000000000000, -15.00000000000002487 ) ) ;
#19119 = CARTESIAN_POINT ( 'NONE',  ( 38.69999999453762030, 167.3344367211045096, 8.961492836873468093 ) ) ;
#19120 = CARTESIAN_POINT ( 'NONE',  ( -7.456977232089304408, 196.8216656703010301, 21.05113791807857027 ) ) ;
#19121 = CARTESIAN_POINT ( 'NONE',  ( 40.11132485994280472, 169.2658477444273331, -4.635254915624224203 ) ) ;
#19122 = LINE ( 'NONE', #2500, #28655 ) ;
#19123 = VERTEX_POINT ( 'NONE', #32405 ) ;
#19124 = CIRCLE ( 'NONE', #7166, 2.149999999999974598 ) ;
#19125 = CARTESIAN_POINT ( 'NONE',  ( 9.736236675708031640, 199.9851607334238963, 31.29886208192143826 ) ) ;
#19126 = DIRECTION ( 'NONE',  ( -1.000000000000000000, 0.000000000000000000, -0.000000000000000000 ) ) ;
#19127 = CARTESIAN_POINT ( 'NONE',  ( 10.01549611932653860, 210.2015048109876716, 52.85113791807854966 ) ) ;
#19128 = ORIENTED_EDGE ( 'NONE', *, *, #29372, .T. ) ;
#19129 = EDGE_CURVE ( 'NONE', #32368, #12301, #28014, .T. ) ;
#19130 = CARTESIAN_POINT ( 'NONE',  ( -6.500168698208244500, 211.6636982574061676, 11.79886208192143648 ) ) ;
#19131 = CARTESIAN_POINT ( 'NONE',  ( 79.58867513459483689, 163.8167787843871110, 12.13525491562421621 ) ) ;
#19132 = EDGE_LOOP ( 'NONE', ( #14689, #15052, #6450, #12595 ) ) ;
#19133 = CARTESIAN_POINT ( 'NONE',  ( 6.444103211790928043, 211.7408657792734061, 99.69886208192144750 ) ) ;
#19134 = CARTESIAN_POINT ( 'NONE',  ( -8.015496119326531499, 204.4483345814780364, 36.35113791807857098 ) ) ;
#19135 = DIRECTION ( 'NONE',  ( -1.000000000000000000, -0.000000000000000000, -0.000000000000000000 ) ) ;
#19136 = ORIENTED_EDGE ( 'NONE', *, *, #19519, .T. ) ;
#19137 = CARTESIAN_POINT ( 'NONE',  ( 40.02499999726881441, 160.0630714827496206, 15.58253174999999402 ) ) ;
#19138 = CARTESIAN_POINT ( 'NONE',  ( 8.062137200540822946, 212.9164362838583315, 60.69886208192143329 ) ) ;
#19139 = CARTESIAN_POINT ( 'NONE',  ( 39.07499999726881157, 141.7447067706911810, -9.630534252274385310 ) ) ;
#19140 = CYLINDRICAL_SURFACE ( 'NONE', #14359, 2.149999999999985256 ) ;
#19141 = CARTESIAN_POINT ( 'NONE',  ( 6.444103211791042618, 202.2591342207267644, 98.30113791807858092 ) ) ;
#19142 = CARTESIAN_POINT ( 'NONE',  ( 55.70000000000000284, 146.4771138417591203, 11.73074641843673227 ) ) ;
#19143 = CARTESIAN_POINT ( 'NONE',  ( -0.05014649552828365914, 215.4116977939061144, 72.24886208192143044 ) ) ;
#19144 = CARTESIAN_POINT ( 'NONE',  ( 77.48867513459484258, 167.7597621252805880, 9.270509831248428867 ) ) ;
#19145 =( BOUNDED_CURVE ( )  B_SPLINE_CURVE ( 2, ( #6486, #16865, #17032, #1534, #30321, #27257, #32700, #9366, #3912, #11755, #19760 ),
 .UNSPECIFIED., .F., .F. ) 
 B_SPLINE_CURVE_WITH_KNOTS ( ( 3, 2, 2, 2, 2, 3 ),
 ( 0.8035714285714284921, 0.8071428571428571619, 0.8107142857142857206, 0.8142857142857142794, 0.8178571428571428381, 0.8214285714285713969 ),
 .UNSPECIFIED. ) 
 CURVE ( )  GEOMETRIC_REPRESENTATION_ITEM ( )  RATIONAL_B_SPLINE_CURVE ( ( 1.000000000000000000, 0.9510565162951534202, 1.000000000000000000, 0.9510565162951534202, 1.000000000000000000, 0.9510565162951534202, 1.000000000000000000, 0.9510565162951534202, 1.000000000000000000, 0.9510565162951534202, 1.000000000000000000 ) ) 
 REPRESENTATION_ITEM ( '' )  );
#19146 = CARTESIAN_POINT ( 'NONE',  ( 55.32499999726881157, 164.1591823560292198, -12.60653300113719766 ) ) ;
#19147 = CARTESIAN_POINT ( 'NONE',  ( 3.044812012440130555, 197.4746971517856764, 14.60113791807856565 ) ) ;
#19148 = CARTESIAN_POINT ( 'NONE',  ( -6.500000000000000888, 1.416734669062281959, -5.722373386996368438 ) ) ;
#19149 = AXIS2_PLACEMENT_3D ( 'NONE', #21569, #13736, #8305 ) ;
#19150 = CARTESIAN_POINT ( 'NONE',  ( 67.12499999726881583, 155.0000000000000000, -15.58253175000000823 ) ) ;
#19151 = CARTESIAN_POINT ( 'NONE',  ( 74.57499999726881867, 145.8408176439707802, 12.60653300113718345 ) ) ;
#19152 = CARTESIAN_POINT ( 'NONE',  ( 9.680171189290831535, 199.9079932115568852, 77.30113791807858092 ) ) ;
#19153 = EDGE_CURVE ( 'NONE', #30423, #5223, #33291, .T. ) ;
#19154 = EDGE_CURVE ( 'NONE', #15698, #25971, #31731, .T. ) ;
#19155 = CARTESIAN_POINT ( 'NONE',  ( -8.062137200540920645, 212.9164362838581894, 99.80113791807858092 ) ) ;
#19156 = CARTESIAN_POINT ( 'NONE',  ( 84.08867513459485110, 142.2402378747194405, 9.270509831248432420 ) ) ;
#19157 = ORIENTED_EDGE ( 'NONE', *, *, #9485, .T. ) ;
#19158 = CARTESIAN_POINT ( 'NONE',  ( 10.00000000000000711, 207.0476921513415220, 3.998862081921434442 ) ) ;
#19159 = CARTESIAN_POINT ( 'NONE',  ( -3.753561863808878130, 218.3979405102790281, 66.09886208192142476 ) ) ;
#19160 = CARTESIAN_POINT ( 'NONE',  ( 6.139770520408223575, 215.5359834540460611, 63.54886208192144181 ) ) ;
#19161 = CARTESIAN_POINT ( 'NONE',  ( -12.00000000000000711, 207.0476921513413515, 102.5011379180785696 ) ) ;
#19162 = CARTESIAN_POINT ( 'NONE',  ( 82.71132485994282035, 155.0000000000000000, 15.00000000000001243 ) ) ;
#19163 = CARTESIAN_POINT ( 'NONE',  ( 8.118202686958039038, 212.8392687619912635, 19.70113791807856884 ) ) ;
#19164 = PRODUCT_RELATED_PRODUCT_CATEGORY ( 'part', '', ( #1257 ) ) ;
#19165 = ADVANCED_FACE ( 'NONE', ( #22352 ), #10104, .F. ) ;
#19166 = CARTESIAN_POINT ( 'NONE',  ( 3.135527875058981895, 197.5041725223112792, 91.59886208192143897 ) ) ;
#19167 = ORIENTED_EDGE ( 'NONE', *, *, #28298, .F. ) ;
#19168 = AXIS2_PLACEMENT_3D ( 'NONE', #7006, #25060, #1714 ) ;
#19169 = CARTESIAN_POINT ( 'NONE',  ( 62.81132485994281467, 150.1262045565064227, 15.00000000000001599 ) ) ;
#19170 = ORIENTED_EDGE ( 'NONE', *, *, #25408, .F. ) ;
#19171 = CYLINDRICAL_SURFACE ( 'NONE', #28175, 40.00000000000000711 ) ;
#19172 = CARTESIAN_POINT ( 'NONE',  ( -6.500168698208244500, 211.6636982574061676, 68.79886208192144181 ) ) ;
#19173 = EDGE_CURVE ( 'NONE', #13672, #22445, #27936, .T. ) ;
#19174 = ORIENTED_EDGE ( 'NONE', *, *, #3252, .T. ) ;
#19175 = CARTESIAN_POINT ( 'NONE',  ( 85.22499999726882436, 160.0630714827496206, -15.58253175000000823 ) ) ;
#19176 = VERTEX_POINT ( 'NONE', #25419 ) ;
#19177 = CYLINDRICAL_SURFACE ( 'NONE', #18877, 1.650000000000000133 ) ;
#19178 = AXIS2_PLACEMENT_3D ( 'NONE', #17472, #4529, #1974 ) ;
#19179 = AXIS2_PLACEMENT_3D ( 'NONE', #17283, #14895, #16938 ) ;
#19180 = CARTESIAN_POINT ( 'NONE',  ( 69.72499999726881015, 169.8198683612136222, 4.815267126137181997 ) ) ;
#19181 = CARTESIAN_POINT ( 'NONE',  ( 7.984503880673485376, 204.3529502787953902, 71.15113791807857524 ) ) ;
#19182 = DIRECTION ( 'NONE',  ( 0.000000000000000000, 0.9988620819214349966, -0.04769215134146094492 ) ) ;
#19183 = DIRECTION ( 'NONE',  ( -0.000000000000000000, 0.000000000000000000, -1.000000000000000000 ) ) ;
#19184 = FILL_AREA_STYLE ('',( #19687 ) ) ;
#19185 = CARTESIAN_POINT ( 'NONE',  ( 37.40000000000000568, 159.7113355953771077, 14.49999999999999289 ) ) ;
#19186 = CARTESIAN_POINT ( 'NONE',  ( -8.000000000000008882, 206.9523078486584780, 41.49886208192143755 ) ) ;
#19187 = CARTESIAN_POINT ( 'NONE',  ( -3.135527875058821579, 197.5041725223112223, 89.90113791807857524 ) ) ;
#19188 = CARTESIAN_POINT ( 'NONE',  ( 0.05014649552810505201, 217.5146222423826714, 64.25113791807856956 ) ) ;
#19189 = AXIS2_PLACEMENT_3D ( 'NONE', #20915, #33523, #23468 ) ;
#19190 = DIRECTION ( 'NONE',  ( -0.000000000000000000, -0.000000000000000000, 1.000000000000000000 ) ) ;
#19191 = CARTESIAN_POINT ( 'NONE',  ( 8.015496119326531499, 209.5516654185219636, 25.85113791807856742 ) ) ;
#19192 = CARTESIAN_POINT ( 'NONE',  ( 130.1133565525086624, -1.374176392886194975, 35.00001200000001234 ) ) ;
#19193 = CARTESIAN_POINT ( 'NONE',  ( 0.04050535873994059316, 7.919512791578233291, -6.573129608219092646 ) ) ;
#19194 = CARTESIAN_POINT ( 'NONE',  ( 45.32499999726881157, 164.1591823560292198, -12.60653300113719766 ) ) ;
#19195 = CARTESIAN_POINT ( 'NONE',  ( 9.736236675707914401, 214.0148392665762458, 49.70113791807856529 ) ) ;
#19196 = CARTESIAN_POINT ( 'NONE',  ( 7.922811941611899833, 4.628808333142401032, -8.057670691780701944 ) ) ;
#19197 = CARTESIAN_POINT ( 'NONE',  ( 8.062137200540920645, 201.0835637161417822, 98.30113791807858092 ) ) ;
#19198 = CARTESIAN_POINT ( 'NONE',  ( -9.984503880673475606, 210.2968891136704315, 72.65113791807857524 ) ) ;
#19199 = CARTESIAN_POINT ( 'NONE',  ( -3.753561863808878130, 218.3979405102790281, 36.09886208192143187 ) ) ;
#19200 = CARTESIAN_POINT ( 'NONE',  ( 3.135527875058981895, 197.5041725223112792, 40.59886208192143187 ) ) ;
#19201 = CARTESIAN_POINT ( 'NONE',  ( 85.19999999453763451, 146.4771138417591203, 11.73074641843673227 ) ) ;
#19202 = VECTOR ( 'NONE', #17619, 1000.000000000000000 ) ;
#19203 = CARTESIAN_POINT ( 'NONE',  ( 7.375838497908181246, 196.7627149292499666, 74.45113791807855819 ) ) ;
#19204 = CARTESIAN_POINT ( 'NONE',  ( 2.517493886308900919, 214.5937144450984420, 100.4011379180785895 ) ) ;
#19205 = AXIS2_PLACEMENT_3D ( 'NONE', #15899, #30920, #28688 ) ;
#19206 = CARTESIAN_POINT ( 'NONE',  ( 10.00000000000000711, 207.0476921513415220, 63.99886208192143044 ) ) ;
#19207 = VECTOR ( 'NONE', #5230, 1000.000000000000000 ) ;
#19208 = EDGE_LOOP ( 'NONE', ( #3296, #17074, #19091, #18305 ) ) ;
#19209 = CARTESIAN_POINT ( 'NONE',  ( -3.662846001189865142, 195.5725841191952838, 61.89886208192143613 ) ) ;
#19210 = EDGE_LOOP ( 'NONE', ( #22817, #21266, #25593, #6643 ) ) ;
#19211 = CARTESIAN_POINT ( 'NONE',  ( 72.97499999726881015, 140.1801316387863778, -4.815267126137194431 ) ) ;
#19212 = CARTESIAN_POINT ( 'NONE',  ( 8.015496119326595448, 204.4483345814782638, 43.14886208192144323 ) ) ;
#19213 = ORIENTED_EDGE ( 'NONE', *, *, #24927, .F. ) ;
#19214 = CARTESIAN_POINT ( 'NONE',  ( 77.67499999726879878, 168.2552932293087906, -9.630534252274387086 ) ) ;
#19215 = CARTESIAN_POINT ( 'NONE',  ( -6.500000000000000000, 3.752776749732564809, -0.7999999999999969358 ) ) ;
#19216 = VECTOR ( 'NONE', #31100, 1000.000000000000000 ) ;
#19217 = DIRECTION ( 'NONE',  ( 0.000000000000000000, 0.7071067811865506814, 0.7071067811865442421 ) ) ;
#19218 = CARTESIAN_POINT ( 'NONE',  ( 2.426778023690261410, 199.3768101843759837, 47.60113791807857808 ) ) ;
#19219 = SURFACE_SIDE_STYLE ('',( #24324 ) ) ;
#19220 =( REPRESENTATION_RELATIONSHIP ('NONE','NONE', #25663, #1289 ) REPRESENTATION_RELATIONSHIP_WITH_TRANSFORMATION ( #25349 )SHAPE_REPRESENTATION_RELATIONSHIP( ) );
#19221 = CARTESIAN_POINT ( 'NONE',  ( -0.05014649552828403384, 217.5146222423826714, 36.24886208192143755 ) ) ;
#19222 = CARTESIAN_POINT ( 'NONE',  ( 68.87499999726881583, 138.6155565068815747, -3.929120461958505118E-15 ) ) ;
#19223 = ORIENTED_EDGE ( 'NONE', *, *, #7683, .T. ) ;
#19224 = CARTESIAN_POINT ( 'NONE',  ( 62.28867513459482552, 139.2280666364260071, -4.041636747397287284E-15 ) ) ;
#19225 = AXIS2_PLACEMENT_3D ( 'NONE', #31473, #29076, #625 ) ;
#19226 = LINE ( 'NONE', #29622, #23220 ) ;
#19227 = CARTESIAN_POINT ( 'NONE',  ( 0.000000000000000000, 8.878689293818310074E-16, -6.500000000000000888 ) ) ;
#19228 = CARTESIAN_POINT ( 'NONE',  ( -2.426778023690076225, 199.3768101843759553, 10.89886208192143613 ) ) ;
#19229 = VECTOR ( 'NONE', #23417, 1000.000000000000000 ) ;
#19230 = CARTESIAN_POINT ( 'NONE',  ( 0.05014649552810505201, 217.5146222423826714, 55.25113791807858377 ) ) ;
#19231 = CARTESIAN_POINT ( 'NONE',  ( -3.135527875058821579, 197.5041725223112223, 38.90113791807857524 ) ) ;
#19232 = CARTESIAN_POINT ( 'NONE',  ( 81.57499999726880446, 164.1591823560292198, -12.60653300113719766 ) ) ;
#19233 = AXIS2_PLACEMENT_3D ( 'NONE', #25583, #10433, #2248 ) ;
#19234 = ITEM_DEFINED_TRANSFORMATION ( 'NONE', 'NONE', #12656,  #2404 ) ;
#19235 = CARTESIAN_POINT ( 'NONE',  ( 8.015496119326595448, 204.4483345814782638, 100.1488620819214646 ) ) ;
#19236 = CARTESIAN_POINT ( 'NONE',  ( 42.02499999726880731, 160.0630714827496206, 15.58253174999999402 ) ) ;
#19237 = SURFACE_SIDE_STYLE ('',( #8835 ) ) ;
#19238 = CARTESIAN_POINT ( 'NONE',  ( 2.000000000000000000, 1.690103923579303787E-15, 1.535499999999999865 ) ) ;
#19239 = CARTESIAN_POINT ( 'NONE',  ( -3.753561863808691168, 195.6020594897209435, 20.90113791807856813 ) ) ;
#19240 = CARTESIAN_POINT ( 'NONE',  ( -52.50000000000002132, 155.0000000000000000, 40.00000000000001421 ) ) ;
#19241 = CARTESIAN_POINT ( 'NONE',  ( -10.01549611932653860, 203.7984951890123284, 69.35113791807857808 ) ) ;
#19242 = CARTESIAN_POINT ( 'NONE',  ( 0.05014649552810506589, 217.5146222423826714, 43.25113791807858377 ) ) ;
#19243 = FACE_OUTER_BOUND ( 'NONE', #30841, .T. ) ;
#19244 = CYLINDRICAL_SURFACE ( 'NONE', #29915, 2.500000000000000000 ) ;
#19245 = CARTESIAN_POINT ( 'NONE',  ( -12.01549611932659722, 210.8513442034533227, 2.648862081921433909 ) ) ;
#19246 = CARTESIAN_POINT ( 'NONE',  ( -3.044812012439970683, 197.4746971517856196, 7.898862081921434353 ) ) ;
#19247 = CARTESIAN_POINT ( 'NONE',  ( 64.79999999453762882, 163.5228861582408797, 11.73074641843673049 ) ) ;
#19248 = ORIENTED_EDGE ( 'NONE', *, *, #24979, .T. ) ;
#19249 = CARTESIAN_POINT ( 'NONE',  ( 9.680171189290831535, 199.9079932115568852, 50.30113791807857382 ) ) ;
#19250 = CARTESIAN_POINT ( 'NONE',  ( 4.903702542908601636, 200.1653181626581102, 68.45113791807857240 ) ) ;
#19251 = DIRECTION ( 'NONE',  ( -1.000000000000000000, -1.804112415015879378E-16, 0.000000000000000000 ) ) ;
#19252 = CARTESIAN_POINT ( 'NONE',  ( 3.044812012439969795, 216.5253028482143520, 30.39886208192143613 ) ) ;
#19253 = CARTESIAN_POINT ( 'NONE',  ( 32.50000000000000000, 155.0000000000000000, -15.00000000000002487 ) ) ;
#19254 = ORIENTED_EDGE ( 'NONE', *, *, #31577, .F. ) ;
#19255 = CARTESIAN_POINT ( 'NONE',  ( 10.00000000000000711, 206.9523078486586201, 80.00113791807856956 ) ) ;
#19256 = VECTOR ( 'NONE', #6087, 1000.000000000000000 ) ;
#19257 = ORIENTED_EDGE ( 'NONE', *, *, #4252, .F. ) ;
#19258 = EDGE_CURVE ( 'NONE', #13595, #1453, #18150, .T. ) ;
#19259 = CARTESIAN_POINT ( 'NONE',  ( 125.0000000000000000, 3.061616997868383121E-14, -35.00000000000000000 ) ) ;
#19260 = CARTESIAN_POINT ( 'NONE',  ( -5.589124336235484769, -4.278671059406953248, -6.219623095964403880 ) ) ;
#19261 = EDGE_LOOP ( 'NONE', ( #18501, #19844, #24226, #13482 ) ) ;
#19262 = CARTESIAN_POINT ( 'NONE',  ( -4.903702542908602524, 213.8346818373418898, 24.95113791807856884 ) ) ;
#19263 = CARTESIAN_POINT ( 'NONE',  ( 32.50000000000000000, 155.0000000000000000, 15.00000000000001243 ) ) ;
#19264 = CARTESIAN_POINT ( 'NONE',  ( 8.062137200540822946, 212.9164362838583315, 3.698862081921434619 ) ) ;
#19265 = CARTESIAN_POINT ( 'NONE',  ( 51.57499999726881157, 164.1591823560292198, -12.60653300113719766 ) ) ;
#19266 = ORIENTED_EDGE ( 'NONE', *, *, #5380, .F. ) ;
#19267 = CARTESIAN_POINT ( 'NONE',  ( 58.92499999726881299, 145.8408176439707802, -12.60653300113719588 ) ) ;
#19268 = DIRECTION ( 'NONE',  ( -1.000000000000000000, 0.000000000000000000, 0.000000000000000000 ) ) ;
#19269 = DIRECTION ( 'NONE',  ( 0.000000000000000000, 0.000000000000000000, 1.000000000000000000 ) ) ;
#19270 = DIRECTION ( 'NONE',  ( 1.000000000000000000, 0.000000000000000000, 0.000000000000000000 ) ) ;
#19271 = CARTESIAN_POINT ( 'NONE',  ( -3.044812012439970683, 197.4746971517856196, 91.89886208192143613 ) ) ;
#19272 = CARTESIAN_POINT ( 'NONE',  ( 57.57499999726881157, 164.1591823560292198, -12.60653300113719766 ) ) ;
#19273 = CARTESIAN_POINT ( 'NONE',  ( -10.00000000000000711, 207.0476921513413515, 18.50113791807856956 ) ) ;
#19274 = CARTESIAN_POINT ( 'NONE',  ( 115.4999999999999858, 182.4348187808683690, 102.3881375866409513 ) ) ;
#19275 = CARTESIAN_POINT ( 'NONE',  ( -7.456977232089471386, 217.1783343296987709, 80.94886208192143329 ) ) ;
#19276 = AXIS2_PLACEMENT_3D ( 'NONE', #19399, #13087, #7314 ) ;
#19277 = CARTESIAN_POINT ( 'NONE',  ( 75.30000000000001137, 163.5228861582408797, 11.73074641843673049 ) ) ;
#19278 = CARTESIAN_POINT ( 'NONE',  ( 2.000000000000000000, 1.773042676681340968, -2.276824562219559311E-15 ) ) ;
#19279 = CARTESIAN_POINT ( 'NONE',  ( 0.000000000000000000, 0.000000000000000000, 0.000000000000000000 ) ) ;
#19280 = CARTESIAN_POINT ( 'NONE',  ( 10.01549611932653860, 210.2015048109876716, 94.85113791807857808 ) ) ;
#19281 = DIRECTION ( 'NONE',  ( 0.000000000000000000, -0.7071067811865411334, 0.7071067811865540120 ) ) ;
#19282 = CARTESIAN_POINT ( 'NONE',  ( 42.07499999726881157, 168.2552932293087906, 9.630534252274372875 ) ) ;
#19283 = CARTESIAN_POINT ( 'NONE',  ( 8.118202686958039038, 212.8392687619912635, 34.70113791807857240 ) ) ;
#19284 = CARTESIAN_POINT ( 'NONE',  ( 75.92499999726881299, 164.1591823560292198, 12.60653300113718167 ) ) ;
#19285 = ORIENTED_EDGE ( 'NONE', *, *, #16895, .F. ) ;
#19286 = LINE ( 'NONE', #9233, #13042 ) ;
#19287 = CARTESIAN_POINT ( 'NONE',  ( 45.79999999453762882, 146.4771138417591203, -11.73074641843674470 ) ) ;
#19288 = CARTESIAN_POINT ( 'NONE',  ( -11.98450388067348804, 210.9467285061362247, 15.65113791807856636 ) ) ;
#19289 = EDGE_CURVE ( 'NONE', #3486, #24793, #17608, .T. ) ;
#19290 = CARTESIAN_POINT ( 'NONE',  ( 92.50248874961125978, 155.0000000000000000, 13.00000000000001066 ) ) ;
#19291 = CARTESIAN_POINT ( 'NONE',  ( -1.060314165522979968, -8.048081368954337123, -7.659344964963557878 ) ) ;
#19292 = ORIENTED_EDGE ( 'NONE', *, *, #14742, .T. ) ;
#19293 = CARTESIAN_POINT ( 'NONE',  ( 3.662846001189864698, 218.4274158808046593, 45.39886208192143613 ) ) ;
#19294 = DIRECTION ( 'NONE',  ( 0.000000000000000000, -1.000000000000000000, 0.000000000000000000 ) ) ;
#19295 = CARTESIAN_POINT ( 'NONE',  ( -10.01549611932653860, 203.7984951890123284, 48.35113791807855677 ) ) ;
#19296 = ORIENTED_EDGE ( 'NONE', *, *, #30827, .T. ) ;
#19297 = CARTESIAN_POINT ( 'NONE',  ( -7.984503880673422316, 204.3529502787951628, 17.34886208192143187 ) ) ;
#19298 = EDGE_CURVE ( 'NONE', #734, #13463, #11751, .T. ) ;
#19299 = PRODUCT_DEFINITION_CONTEXT ( 'detailed design', #22914, 'design' ) ;
#19300 = CARTESIAN_POINT ( 'NONE',  ( -25.25629716696160543, -17.17253483735098030, -16.29170001372755650 ) ) ;
#19301 = VERTEX_POINT ( 'NONE', #11968 ) ;
#19302 = CARTESIAN_POINT ( 'NONE',  ( 2.426778023690075337, 214.6231898156240447, 102.3988620819214361 ) ) ;
#19303 = DIRECTION ( 'NONE',  ( 1.000000000000000000, 0.000000000000000000, 0.000000000000000000 ) ) ;
#19304 = CARTESIAN_POINT ( 'NONE',  ( -2.517493886308901807, 199.4062855549015012, 41.90113791807856813 ) ) ;
#19305 = DIRECTION ( 'NONE',  ( 1.000000000000000000, 0.000000000000000000, 0.000000000000000000 ) ) ;
#19306 = EDGE_LOOP ( 'NONE', ( #17752, #6905, #10099, #28886 ) ) ;
#19307 = CARTESIAN_POINT ( 'NONE',  ( 36.62499999726881583, 138.6155565068815463, -3.929120461958505118E-15 ) ) ;
#19308 = EDGE_CURVE ( 'NONE', #317, #11207, #25252, .T. ) ;
#19309 = CARTESIAN_POINT ( 'NONE',  ( 8.062137200540822946, 212.9164362838583315, 63.69886208192143329 ) ) ;
#19310 = CARTESIAN_POINT ( 'NONE',  ( 42.17499999726881299, 164.1591823560292198, 12.60653300113718167 ) ) ;
#19311 = DIRECTION ( 'NONE',  ( -1.000000000000000000, -0.000000000000000000, -0.000000000000000000 ) ) ;
#19312 = CARTESIAN_POINT ( 'NONE',  ( -7.984503880673488041, 209.6470497212046098, 93.65113791807857524 ) ) ;
#19313 = CARTESIAN_POINT ( 'NONE',  ( 51.79999999999999005, 142.6655632788954620, 8.961492836873471646 ) ) ;
#19314 = LINE ( 'NONE', #10697, #1150 ) ;
#19315 = CARTESIAN_POINT ( 'NONE',  ( 2.517493886309087436, 199.4062855549015865, 76.59886208192142476 ) ) ;
#19316 = DIRECTION ( 'NONE',  ( 1.000000000000000000, -0.000000000000000000, -0.000000000000000000 ) ) ;
#19317 = CARTESIAN_POINT ( 'NONE',  ( 3.499999999999999556, 0.000000000000000000, -2.899999999999999911 ) ) ;
#19318 = EDGE_CURVE ( 'NONE', #33225, #31608, #30715, .T. ) ;
#19319 = CARTESIAN_POINT ( 'NONE',  ( 58.72499999726881015, 140.1801316387863778, -4.815267126137194431 ) ) ;
#19321 = EDGE_LOOP ( 'NONE', ( #17285, #12727, #26740, #3409 ) ) ;
#19320 = CARTESIAN_POINT ( 'NONE',  ( 10.00000000000000711, 206.9523078486586201, 23.00113791807856600 ) ) ;
#19322 = CARTESIAN_POINT ( 'NONE',  ( -6.838249472399978046, -3.995156693690920413, -6.573189567101943354 ) ) ;
#19323 = CARTESIAN_POINT ( 'NONE',  ( 81.87499999726880162, 171.3844434931184253, -7.942151717890132712E-15 ) ) ;
#19324 = CARTESIAN_POINT ( 'NONE',  ( 11.98450388067348271, 203.0532714938637753, 74.15113791807857524 ) ) ;
#19325 = EDGE_CURVE ( 'NONE', #14133, #1695, #2257, .T. ) ;
#19326 = CARTESIAN_POINT ( 'NONE',  ( -3.044812012440131443, 216.5253028482142952, 94.10113791807857808 ) ) ;
#19327 = DIRECTION ( 'NONE',  ( -0.000000000000000000, 1.478898702612462246E-15, 1.000000000000000000 ) ) ;
#19328 = EDGE_LOOP ( 'NONE', ( #32625, #14986, #1688 ) ) ;
#19329 = CARTESIAN_POINT ( 'NONE',  ( 12.00000000000000711, 207.0476921513415220, 102.9988620819214304 ) ) ;
#19330 = CARTESIAN_POINT ( 'NONE',  ( -11.98450388067341876, 203.0532714938636047, 59.34886208192144608 ) ) ;
#19331 = CARTESIAN_POINT ( 'NONE',  ( 9.984503880673420539, 210.2968891136705736, 72.84886208192143897 ) ) ;
#19332 = CARTESIAN_POINT ( 'NONE',  ( 12.01549611932659367, 203.1486557965466773, 7.148862081921435241 ) ) ;
#19333 = CARTESIAN_POINT ( 'NONE',  ( 108.0159016311981759, 155.0000000000000000, 12.10452846326767684 ) ) ;
#19334 = CARTESIAN_POINT ( 'NONE',  ( 0.05014649552810505201, 217.5146222423826714, 22.25113791807856956 ) ) ;
#19335 = CARTESIAN_POINT ( 'NONE',  ( -10.01549611932659722, 210.2015048109875011, 89.64886208192143613 ) ) ;
#19336 = VERTEX_POINT ( 'NONE', #4124 ) ;
#19337 = ORIENTED_EDGE ( 'NONE', *, *, #33256, .F. ) ;
#19338 = CARTESIAN_POINT ( 'NONE',  ( -1.472725187932624030E-14, 206.9977241638431167, -6.000000000000014211 ) ) ;
#19339 = CARTESIAN_POINT ( 'NONE',  ( -8.015496119326597224, 209.5516654185217362, 74.64886208192143613 ) ) ;
#19340 = ORIENTED_EDGE ( 'NONE', *, *, #33487, .F. ) ;
#19341 = PRODUCT_DEFINITION_SHAPE ( 'NONE', 'NONE',  #33723 ) ;
#19342 = CARTESIAN_POINT ( 'NONE',  ( 82.72499999726881015, 140.1801316387863778, -4.815267126137194431 ) ) ;
#19344 = VERTEX_POINT ( 'NONE', #22868 ) ;
#19343 = B_SPLINE_CURVE_WITH_KNOTS ( 'NONE', 3,
 ( #6751, #27525, #24983, #1634, #20542, #17993, #25312, #12706 ),
 .UNSPECIFIED., .F., .F.,
 ( 4, 2, 2, 4 ),
 ( 0.04438889715320012974, 0.04840678451617883016, 0.05242467187915753057, 0.06046044660511493835 ),
 .UNSPECIFIED. ) ;
#19345 = CARTESIAN_POINT ( 'NONE',  ( 78.92499999726881299, 145.8408176439707802, -12.60653300113719588 ) ) ;
#19346 =( BOUNDED_CURVE ( )  B_SPLINE_CURVE ( 2, ( #2762, #13140, #7189, #23025, #32027, #13628, #28814, #26918, #10599, #21135, #3241 ),
 .UNSPECIFIED., .F., .T. ) 
 B_SPLINE_CURVE_WITH_KNOTS ( ( 3, 2, 2, 2, 2, 3 ),
 ( 0.8928571428571427937, 0.8964285714285712414, 0.8999999999999998002, 0.9035714285714282479, 0.9071428571428569176, 0.9107142857142853654 ),
 .UNSPECIFIED. ) 
 CURVE ( )  GEOMETRIC_REPRESENTATION_ITEM ( )  RATIONAL_B_SPLINE_CURVE ( ( 1.000000000000000000, 0.9510565162951534202, 1.000000000000000000, 0.9510565162951534202, 1.000000000000000000, 0.9510565162951534202, 1.000000000000000000, 0.9510565162951534202, 1.000000000000000000, 0.9510565162951579721, 0.9999999999999954481 ) ) 
 REPRESENTATION_ITEM ( '' )  );
#19347 = CARTESIAN_POINT ( 'NONE',  ( -8.015496119326531499, 204.4483345814780364, 72.35113791807857808 ) ) ;
#19348 = EDGE_CURVE ( 'NONE', #15698, #2881, #21949, .T. ) ;
#19349 = DIRECTION ( 'NONE',  ( -1.000000000000000000, 0.000000000000000000, 0.000000000000000000 ) ) ;
#19350 = EDGE_CURVE ( 'NONE', #27043, #23387, #27468, .T. ) ;
#19351 = CARTESIAN_POINT ( 'NONE',  ( 38.10000000000000142, 141.2096805137202580, -4.480746418436742040 ) ) ;
#19352 = CARTESIAN_POINT ( 'NONE',  ( 2.517493886309087436, 199.4062855549015865, 40.59886208192143897 ) ) ;
#19353 = CARTESIAN_POINT ( 'NONE',  ( -9.984503880673473830, 210.2968891136704315, 87.65113791807854682 ) ) ;
#19354 = EDGE_CURVE ( 'NONE', #23763, #29401, #30674, .T. ) ;
#19355 = CARTESIAN_POINT ( 'NONE',  ( 6.220909254589536808, 215.4770327129947702, 70.55113791807856671 ) ) ;
#19356 = FACE_BOUND ( 'NONE', #16855, .T. ) ;
#19357 = CARTESIAN_POINT ( 'NONE',  ( -105.0000000000000142, 2.449293598294705330E-15, -20.00000000000000000 ) ) ;
#19358 = CARTESIAN_POINT ( 'NONE',  ( 34.50000000000000000, -72.99999999999998579, -30.00000000000000000 ) ) ;
#19359 = CARTESIAN_POINT ( 'NONE',  ( 52.42499999726880588, 141.7447067706911810, 9.630534252274376428 ) ) ;
#19360 = CARTESIAN_POINT ( 'NONE',  ( -3.753561863808691168, 195.6020594897209435, 47.90113791807857524 ) ) ;
#19361 = DIRECTION ( 'NONE',  ( 0.000000000000000000, 0.000000000000000000, -1.000000000000000000 ) ) ;
#19362 = EDGE_CURVE ( 'NONE', #11329, #6902, #1817, .T. ) ;
#19363 = CARTESIAN_POINT ( 'NONE',  ( 10.00000000000000711, 206.9523078486586201, 98.00113791807856956 ) ) ;
#19364 = CARTESIAN_POINT ( 'NONE',  ( 10.00000000000000711, 206.9523078486586201, 68.00113791807856956 ) ) ;
#19365 = CARTESIAN_POINT ( 'NONE',  ( 3.753561863808876797, 195.6020594897209719, 28.59886208192143897 ) ) ;
#19366 = CARTESIAN_POINT ( 'NONE',  ( 3.044812012439969795, 216.5253028482143520, 42.39886208192143613 ) ) ;
#19367 = CARTESIAN_POINT ( 'NONE',  ( 87.29999999453764303, 142.6655632788954620, 8.961492836873471646 ) ) ;
#19368 = CARTESIAN_POINT ( 'NONE',  ( -12.00000000000000711, 207.0476921513413515, 78.50113791807856956 ) ) ;
#19369 = CARTESIAN_POINT ( 'NONE',  ( -8.015496119326531499, 204.4483345814780364, 96.35113791807857808 ) ) ;
#19370 = CARTESIAN_POINT ( 'NONE',  ( -0.05014649552828403384, 217.5146222423826714, 60.24886208192142334 ) ) ;
#19371 = CARTESIAN_POINT ( 'NONE',  ( 77.50000000000000000, 155.0000000000000000, -6.938893903907228378E-15 ) ) ;
#19372 = ORIENTED_EDGE ( 'NONE', *, *, #1625, .T. ) ;
#19373 = CARTESIAN_POINT ( 'NONE',  ( 0.05014649552828288198, 194.3824533091408000, 64.74886208192143044 ) ) ;
#19374 = ORIENTED_EDGE ( 'NONE', *, *, #7292, .F. ) ;
#19375 = CARTESIAN_POINT ( 'NONE',  ( 74.17499999726881299, 164.1591823560292198, 12.60653300113718167 ) ) ;
#19376 = CARTESIAN_POINT ( 'NONE',  ( 7.984503880673422316, 209.6470497212048372, 39.84886208192144608 ) ) ;
#19377 = ORIENTED_EDGE ( 'NONE', *, *, #28462, .F. ) ;
#19378 = VECTOR ( 'NONE', #32398, 1000.000000000000114 ) ;
#19379 = CARTESIAN_POINT ( 'NONE',  ( 85.97499999726882436, 169.8198683612136222, 4.815267126137181997 ) ) ;
#19380 = CARTESIAN_POINT ( 'NONE',  ( -2.346298152288376571, 2.686816014504558758, -2.900000000000002576 ) ) ;
#19381 = LINE ( 'NONE', #498, #5109 ) ;
#19382 = CARTESIAN_POINT ( 'NONE',  ( -7.984503880673488041, 209.6470497212046098, 51.65113791807857524 ) ) ;
#19383 = DIRECTION ( 'NONE',  ( 0.000000000000000000, 1.224646799147353207E-16, 1.000000000000000000 ) ) ;
#19384 = EDGE_CURVE ( 'NONE', #22574, #29479, #19765, .T. ) ;
#19385 = CARTESIAN_POINT ( 'NONE',  ( -9.984503880673420539, 203.7031108863293980, 35.34886208192142476 ) ) ;
#19386 = CARTESIAN_POINT ( 'NONE',  ( 71.37499999726881583, 155.0000000000000000, -15.58253175000000823 ) ) ;
#19387 = EDGE_LOOP ( 'NONE', ( #7026, #20769 ) ) ;
#19388 = AXIS2_PLACEMENT_3D ( 'NONE', #14956, #27555, #17507 ) ;
#19389 = LINE ( 'NONE', #29955, #23281 ) ;
#19390 = DIRECTION ( 'NONE',  ( -0.000000000000000000, -0.000000000000000000, 1.000000000000000000 ) ) ;
#19391 = DIRECTION ( 'NONE',  ( 0.000000000000000000, 0.000000000000000000, 1.000000000000000000 ) ) ;
#19392 = CARTESIAN_POINT ( 'NONE',  ( -8.000000000000008882, 206.9523078486584780, 14.49886208192143577 ) ) ;
#19393 = CARTESIAN_POINT ( 'NONE',  ( -8.118202686958039038, 201.1607312380087080, 60.20113791807857240 ) ) ;
#19394 = CARTESIAN_POINT ( 'NONE',  ( 6.139770520408368348, 198.4640165459539674, 38.45113791807855819 ) ) ;
#19395 = CARTESIAN_POINT ( 'NONE',  ( 66.88867513459483405, 159.8737954434938615, -14.99999999999984190 ) ) ;
#19396 = ITEM_DEFINED_TRANSFORMATION ( 'NONE', 'NONE', #6094,  #2404 ) ;
#19397 = CARTESIAN_POINT ( 'NONE',  ( -4.984841277089726574, 200.2242689037092305, 0.05113791807856601229 ) ) ;
#19398 = CARTESIAN_POINT ( 'NONE',  ( 42.42499999726881299, 141.7447067706911810, 9.630534252274376428 ) ) ;
#19399 = CARTESIAN_POINT ( 'NONE',  ( 0.000000000000000000, 0.000000000000000000, 0.000000000000000000 ) ) ;
#19400 = CARTESIAN_POINT ( 'NONE',  ( 33.92499999726881299, 164.1591823560292198, 12.60653300113718167 ) ) ;
#19401 = CARTESIAN_POINT ( 'NONE',  ( -11.98450388067348804, 210.9467285061362247, 18.65113791807856458 ) ) ;
#19402 = CARTESIAN_POINT ( 'NONE',  ( 82.58867513459483689, 146.1832212156128890, -12.13525491562423042 ) ) ;
#19403 = CARTESIAN_POINT ( 'NONE',  ( -8.062137200540920645, 212.9164362838581894, 69.80113791807856671 ) ) ;
#19404 = CARTESIAN_POINT ( 'NONE',  ( 6.139770520408367460, 198.4640165459539389, 44.45113791807856529 ) ) ;
#19405 = CIRCLE ( 'NONE', #29206, 2.149999999999994138 ) ;
#19406 = LINE ( 'NONE', #22634, #32831 ) ;
#19407 = DIRECTION ( 'NONE',  ( 1.000000000000000000, 0.000000000000000000, 0.000000000000000000 ) ) ;
#19408 = CARTESIAN_POINT ( 'NONE',  ( 11.98450388067341876, 210.9467285061363953, 6.848862081921435419 ) ) ;
#19409 = CARTESIAN_POINT ( 'NONE',  ( 3.135527875058981895, 197.5041725223112792, 7.598862081921435419 ) ) ;
#19410 = CARTESIAN_POINT ( 'NONE',  ( 69.29999999453764303, 142.6655632788954620, 8.961492836873471646 ) ) ;
#19411 = ORIENTED_EDGE ( 'NONE', *, *, #28019, .F. ) ;
#19412 = CARTESIAN_POINT ( 'NONE',  ( -12.01549611932652972, 203.1486557965464499, 48.35113791807857098 ) ) ;
#19413 = CARTESIAN_POINT ( 'NONE',  ( 4.903702542908601636, 200.1653181626581102, 65.45113791807858661 ) ) ;
#19414 = CARTESIAN_POINT ( 'NONE',  ( 6.220909254589681581, 198.5229672870052582, 31.44886208192142263 ) ) ;
#19415 = CARTESIAN_POINT ( 'NONE',  ( 60.63708498984762940, 120.3589838486224437, 20.00000000000000000 ) ) ;
#19416 = TOROIDAL_SURFACE ( 'NONE', #17793, 2.466666666666999408, 1.033333333332998372 ) ;
#19417 = ORIENTED_EDGE ( 'NONE', *, *, #1423, .F. ) ;
#19418 = CARTESIAN_POINT ( 'NONE',  ( 0.05014649552810505201, 217.5146222423826714, 94.25113791807855534 ) ) ;
#19419 = ORIENTED_EDGE ( 'NONE', *, *, #1655, .F. ) ;
#19420 = CARTESIAN_POINT ( 'NONE',  ( 57.88867513459482694, 150.1262045565065364, 15.00000000000011191 ) ) ;
#19421 = CARTESIAN_POINT ( 'NONE',  ( 4.000000000000000000, 0.000000000000000000, 0.000000000000000000 ) ) ;
#19422 = EDGE_LOOP ( 'NONE', ( #30397, #19599, #13886 ) ) ;
#19423 = CARTESIAN_POINT ( 'NONE',  ( -8.015496119326531499, 204.4483345814780364, 18.35113791807856387 ) ) ;
#19424 = CIRCLE ( 'NONE', #30303, 3.309499999999999886 ) ;
#19425 = CARTESIAN_POINT ( 'NONE',  ( 32.50000000000000000, 155.0000000000000000, -6.938893903907228378E-15 ) ) ;
#19426 = VECTOR ( 'NONE', #648, 1000.000000000000114 ) ;
#19427 = CARTESIAN_POINT ( 'NONE',  ( 6.139770520408223575, 215.5359834540460611, 6.548862081921434708 ) ) ;
#19428 = CARTESIAN_POINT ( 'NONE',  ( 48.97499999726881725, 140.1801316387863778, -4.815267126137194431 ) ) ;
#19429 = ORIENTED_EDGE ( 'NONE', *, *, #26473, .F. ) ;
#19430 = CARTESIAN_POINT ( 'NONE',  ( 55.22499999726880304, 160.0630714827496206, -15.58253175000000823 ) ) ;
#19431 = CARTESIAN_POINT ( 'NONE',  ( -2.426778023690262742, 214.6231898156240163, 49.10113791807857808 ) ) ;
#19432 = DIRECTION ( 'NONE',  ( -0.000000000000000000, -0.000000000000000000, 1.000000000000000000 ) ) ;
#19433 = CARTESIAN_POINT ( 'NONE',  ( 4.764707147349631625E-14, -103.0000000000000284, 30.00000000000000000 ) ) ;
#19434 = CARTESIAN_POINT ( 'NONE',  ( 0.05014649552828275708, 196.4853777576173002, 88.74886208192140202 ) ) ;
#19435 = CARTESIAN_POINT ( 'NONE',  ( 57.17499999726881299, 145.8408176439707802, -12.60653300113719588 ) ) ;
#19436 = CARTESIAN_POINT ( 'NONE',  ( -3.044812012440131443, 216.5253028482142952, 37.10113791807857098 ) ) ;
#19437 = CARTESIAN_POINT ( 'NONE',  ( 0.000000000000000000, 0.000000000000000000, -2.899999999999999911 ) ) ;
#19438 = CARTESIAN_POINT ( 'NONE',  ( 7.375838497908012492, 217.2372850707501186, 75.54886208192142760 ) ) ;
#19439 = CIRCLE ( 'NONE', #6944, 32.00000000000002842 ) ;
#19440 = CARTESIAN_POINT ( 'NONE',  ( 82.90000000000000568, 168.7903194862797420, -4.480746418436745593 ) ) ;
#19441 = CARTESIAN_POINT ( 'NONE',  ( 39.78867513459481842, 155.0000000000000000, 15.00000000000001243 ) ) ;
#19442 = DIRECTION ( 'NONE',  ( 0.000000000000000000, 0.000000000000000000, -1.000000000000000000 ) ) ;
#19443 = CARTESIAN_POINT ( 'NONE',  ( 9.984503880673470277, 203.7031108863295401, 92.15113791807856103 ) ) ;
#19444 = DIRECTION ( 'NONE',  ( -1.000000000000000000, 0.000000000000000000, 0.000000000000000000 ) ) ;
#19445 = CARTESIAN_POINT ( 'NONE',  ( 44.87499999726880873, 138.6155565068815463, -3.929120461958505118E-15 ) ) ;
#19446 = CARTESIAN_POINT ( 'NONE',  ( -10.00000000000000711, 207.0476921513413515, 33.50113791807856956 ) ) ;
#19447 = EDGE_CURVE ( 'NONE', #8252, #26926, #5085, .T. ) ;
#19448 = CARTESIAN_POINT ( 'NONE',  ( 84.92499999726882720, 145.8408176439707802, -12.60653300113719588 ) ) ;
#19449 = ORIENTED_EDGE ( 'NONE', *, *, #25391, .T. ) ;
#19450 = CARTESIAN_POINT ( 'NONE',  ( -7.922281120364393914, 4.573931137438271399, -8.047472243342930653 ) ) ;
#19451 = CARTESIAN_POINT ( 'NONE',  ( 117.5000000000000000, 102.0000000000001990, 89.64869280115064498 ) ) ;
#19453 = ADVANCED_FACE ( 'NONE', ( #12303 ), #14879, .T. ) ;
#19452 = CARTESIAN_POINT ( 'NONE',  ( 49.39999999453763024, 141.2096805137202580, 4.480746418436733158 ) ) ;
#19454 = CARTESIAN_POINT ( 'NONE',  ( 7.375838497908181246, 196.7627149292499666, 23.45113791807856884 ) ) ;
#19455 = AXIS2_PLACEMENT_3D ( 'NONE', #9850, #12742, #17680 ) ;
#19456 = CARTESIAN_POINT ( 'NONE',  ( 5.541103744621880989E-15, 31.75426480542943608, -18.00000000000000000 ) ) ;
#19457 =( GEOMETRIC_REPRESENTATION_CONTEXT ( 3 ) GLOBAL_UNCERTAINTY_ASSIGNED_CONTEXT ( ( #7966 ) ) GLOBAL_UNIT_ASSIGNED_CONTEXT ( ( #24310, #21757, #15274 ) ) REPRESENTATION_CONTEXT ( 'NONE', 'WORKASPACE' ) );
#19458 = DIRECTION ( 'NONE',  ( 0.000000000000000000, 1.000000000000000000, -1.295896757998781572E-15 ) ) ;
#19459 = ORIENTED_EDGE ( 'NONE', *, *, #11754, .F. ) ;
#19460 = STYLED_ITEM ( 'NONE', ( #28907 ), #1232 ) ;
#19461 = CARTESIAN_POINT ( 'NONE',  ( 12.00000000000000711, 207.0476921513415220, 39.99886208192143755 ) ) ;
#19462 = DIRECTION ( 'NONE',  ( 1.000000000000000000, -0.000000000000000000, -0.000000000000000000 ) ) ;
#19463 = CARTESIAN_POINT ( 'NONE',  ( -0.05014649552810635652, 196.4853777576173002, 50.75113791807856956 ) ) ;
#19464 = CARTESIAN_POINT ( 'NONE',  ( -0.05014649552828365914, 215.4116977939061144, 9.248862081921435774 ) ) ;
#19465 = CIRCLE ( 'NONE', #4781, 4.200000000000001954 ) ;
#19466 = CARTESIAN_POINT ( 'NONE',  ( -27.50000000000000000, -15.87713240271474824, -15.54379906938135214 ) ) ;
#19467 = VERTEX_POINT ( 'NONE', #7198 ) ;
#19468 = CARTESIAN_POINT ( 'NONE',  ( 4.903702542908435547, 213.8346818373419751, 102.5488620819214560 ) ) ;
#19469 = CARTESIAN_POINT ( 'NONE',  ( 97.20416941062678973, 155.0000000000000000, 0.000000000000000000 ) ) ;
#19470 = CARTESIAN_POINT ( 'NONE',  ( -4.984841277089726574, 200.2242689037092305, 45.05113791807857382 ) ) ;
#19471 = CARTESIAN_POINT ( 'NONE',  ( 0.000000000000000000, 0.000000000000000000, -1.400415076419418092 ) ) ;
#19472 = ORIENTED_EDGE ( 'NONE', *, *, #28341, .F. ) ;
#19473 = CARTESIAN_POINT ( 'NONE',  ( 36.02499999726881441, 160.0630714827496206, 15.58253174999999402 ) ) ;
#19474 = CARTESIAN_POINT ( 'NONE',  ( -10.00000000000000178, 206.7692714347156198, 108.3323677711372000 ) ) ;
#19475 = EDGE_CURVE ( 'NONE', #24793, #3486, #206, .T. ) ;
#19476 = CIRCLE ( 'NONE', #4250, 4.200000000000001954 ) ;
#19477 = CARTESIAN_POINT ( 'NONE',  ( -3.044812012439970683, 197.4746971517856196, 64.89886208192145034 ) ) ;
#19478 = CARTESIAN_POINT ( 'NONE',  ( 43.77499999726881441, 169.8198683612136222, -4.815267126137197984 ) ) ;
#19479 = DIRECTION ( 'NONE',  ( 0.000000000000000000, 0.000000000000000000, -1.000000000000000000 ) ) ;
#19480 = CARTESIAN_POINT ( 'NONE',  ( -0.05014649552807731031, 198.5883022060938572, 95.75113791807856956 ) ) ;
#19481 = PRODUCT_DEFINITION_SHAPE ( 'NONE', 'NONE',  #6235 ) ;
#19482 = CIRCLE ( 'NONE', #27622, 30.00000000000000000 ) ;
#19483 = CARTESIAN_POINT ( 'NONE',  ( 63.20000000000000995, 167.3344367211045096, 8.961492836873468093 ) ) ;
#19484 = CARTESIAN_POINT ( 'NONE',  ( 76.78867513459483973, 155.0000000000000000, -15.00000000000002487 ) ) ;
#19485 = CARTESIAN_POINT ( 'NONE',  ( -6.500168698208244500, 211.6636982574061676, 83.79886208192144181 ) ) ;
#19486 = CARTESIAN_POINT ( 'NONE',  ( -1.126429428730189031, 7.232124035235028892, -6.344710093416086494 ) ) ;
#19487 = LINE ( 'NONE', #9091, #1973 ) ;
#19488 = EDGE_CURVE ( 'NONE', #8582, #16783, #2420, .T. ) ;
#19489 = CARTESIAN_POINT ( 'NONE',  ( 60.02499999726880020, 160.0630714827496206, 15.58253174999999402 ) ) ;
#19491 = ORIENTED_EDGE ( 'NONE', *, *, #1465, .T. ) ;
#19490 = CARTESIAN_POINT ( 'NONE',  ( 3.044812012440130555, 197.4746971517856764, 23.60113791807857098 ) ) ;
#19492 = DIRECTION ( 'NONE',  ( 1.000000000000000000, 0.000000000000000000, 0.000000000000000000 ) ) ;
#19493 = CARTESIAN_POINT ( 'NONE',  ( 83.27499999726880731, 149.9369285172503510, -15.58253175000000823 ) ) ;
#19494 = CARTESIAN_POINT ( 'NONE',  ( 12.00000000000000711, 206.9523078486586485, 89.00113791807858377 ) ) ;
#19495 = EDGE_CURVE ( 'NONE', #30928, #31779, #26423, .T. ) ;
#19496 = CARTESIAN_POINT ( 'NONE',  ( 55.78867513459481842, 155.0000000000000000, 15.00000000000001243 ) ) ;
#19497 = CARTESIAN_POINT ( 'NONE',  ( 53.08867513459482979, 167.7597621252805880, -9.270509831248443078 ) ) ;
#19498 = EDGE_CURVE ( 'NONE', #24269, #10286, #23731, .T. ) ;
#19499 = ORIENTED_EDGE ( 'NONE', *, *, #23497, .F. ) ;
#19500 = CARTESIAN_POINT ( 'NONE',  ( -9.736236675708031640, 214.0148392665760753, 68.79886208192144181 ) ) ;
#19501 = CARTESIAN_POINT ( 'NONE',  ( -3.135527875058982783, 216.4958274776886924, 75.09886208192143897 ) ) ;
#19502 = CARTESIAN_POINT ( 'NONE',  ( -3.753561863808878130, 218.3979405102790281, 12.09886208192143364 ) ) ;
#19503 = CARTESIAN_POINT ( 'NONE',  ( -9.000000000000001776, 206.7692714347155629, 108.3323677711371857 ) ) ;
#19504 = CIRCLE ( 'NONE', #2668, 0.9999999999999947820 ) ;
#19505 = CARTESIAN_POINT ( 'NONE',  ( 6.139770520408368348, 198.4640165459539674, 20.45113791807855819 ) ) ;
#19506 = CARTESIAN_POINT ( 'NONE',  ( 3.135527875058981895, 197.5041725223112792, 85.59886208192143897 ) ) ;
#19507 = AXIS2_PLACEMENT_3D ( 'NONE', #2177, #2691, #5229 ) ;
#19508 = ORIENTED_EDGE ( 'NONE', *, *, #23480, .F. ) ;
#19509 = CIRCLE ( 'NONE', #1033, 3.500000000000000000 ) ;
#19510 = DIRECTION ( 'NONE',  ( 0.000000000000000000, 0.000000000000000000, -1.000000000000000000 ) ) ;
#19511 = ORIENTED_EDGE ( 'NONE', *, *, #23883, .T. ) ;
#19512 = DIRECTION ( 'NONE',  ( -1.000000000000000000, -0.000000000000000000, -0.000000000000000000 ) ) ;
#19513 = CARTESIAN_POINT ( 'NONE',  ( 8.000000000000008882, 207.0476921513415220, 66.99886208192144466 ) ) ;
#19514 = VERTEX_POINT ( 'NONE', #7882 ) ;
#19515 = AXIS2_PLACEMENT_3D ( 'NONE', #9741, #27788, #25404 ) ;
#19516 = CARTESIAN_POINT ( 'NONE',  ( 82.82499999726881867, 141.7447067706911810, -9.630534252274387086 ) ) ;
#19517 = ORIENTED_EDGE ( 'NONE', *, *, #5641, .T. ) ;
#19518 = FACE_OUTER_BOUND ( 'NONE', #16867, .T. ) ;
#19519 = EDGE_CURVE ( 'NONE', #5796, #7152, #455, .T. ) ;
#19520 = CARTESIAN_POINT ( 'NONE',  ( 78.32499999726881867, 145.8408176439707802, 12.60653300113718345 ) ) ;
#19521 = DIRECTION ( 'NONE',  ( 1.000000000000000000, 0.000000000000000000, 0.000000000000000000 ) ) ;
#19522 = CARTESIAN_POINT ( 'NONE',  ( -2.517493886308901807, 199.4062855549015012, 68.90113791807856103 ) ) ;
#19523 = DIRECTION ( 'NONE',  ( 0.000000000000000000, 0.000000000000000000, 1.000000000000000000 ) ) ;
#19524 =( NAMED_UNIT ( * ) PLANE_ANGLE_UNIT ( ) SI_UNIT ( $, .RADIAN. ) );
#19525 = CARTESIAN_POINT ( 'NONE',  ( 35.89999999999999858, 141.2096805137202580, 4.480746418436733158 ) ) ;
#19526 = CARTESIAN_POINT ( 'NONE',  ( 8.015496119326595448, 204.4483345814782638, 55.14886208192145034 ) ) ;
#19527 = AXIS2_PLACEMENT_3D ( 'NONE', #18816, #925, #429 ) ;
#19528 = CARTESIAN_POINT ( 'NONE',  ( -6.220909254589537696, 198.5229672870051161, 75.05113791807858092 ) ) ;
#19529 = EDGE_CURVE ( 'NONE', #2045, #21331, #11628, .T. ) ;
#19530 = VECTOR ( 'NONE', #4094, 1000.000000000000227 ) ;
#19531 = DIRECTION ( 'NONE',  ( 0.000000000000000000, 0.000000000000000000, 1.000000000000000000 ) ) ;
#19532 = CARTESIAN_POINT ( 'NONE',  ( 73.71132485994280614, 155.0000000000000000, -15.00000000000002487 ) ) ;
#19533 = DIRECTION ( 'NONE',  ( 1.000000000000000000, 0.000000000000000000, 0.000000000000000000 ) ) ;
#19534 = CARTESIAN_POINT ( 'NONE',  ( 53.52499999726881441, 169.8198683612136222, -4.815267126137197984 ) ) ;
#19535 = CARTESIAN_POINT ( 'NONE',  ( 3.662846001190051659, 195.5725841191953691, 53.60113791807856387 ) ) ;
#19536 = DIRECTION ( 'NONE',  ( 1.000000000000000000, -0.000000000000000000, -0.000000000000000000 ) ) ;
#19537 = CARTESIAN_POINT ( 'NONE',  ( -7.456977232089304408, 196.8216656703010301, 0.05113791807856556820 ) ) ;
#19538 = CARTESIAN_POINT ( 'NONE',  ( -8.118202686958039038, 201.1607312380087080, 78.20113791807857240 ) ) ;
#19539 = ADVANCED_FACE ( 'NONE', ( #23541 ), #29035, .T. ) ;
#19540 = CARTESIAN_POINT ( 'NONE',  ( 3.662846001189864698, 218.4274158808046593, 36.39886208192143613 ) ) ;
#19541 = CARTESIAN_POINT ( 'NONE',  ( -10.00000000000000711, 206.9523078486584495, 50.49886208192143044 ) ) ;
#19542 = CARTESIAN_POINT ( 'NONE',  ( 86.89999999453760893, 159.7113355953771077, 14.49999999999999289 ) ) ;
#19543 = CARTESIAN_POINT ( 'NONE',  ( -12.01549611932652972, 203.1486557965464499, 90.35113791807857808 ) ) ;
#19544 = CARTESIAN_POINT ( 'NONE',  ( 6.500168698208129925, 211.6636982574063381, 100.7011379180785866 ) ) ;
#19545 = CARTESIAN_POINT ( 'NONE',  ( -3.044812012439970683, 197.4746971517856196, 55.89886208192143613 ) ) ;
#19546 = VERTEX_POINT ( 'NONE', #30885 ) ;
#19547 = CARTESIAN_POINT ( 'NONE',  ( -12.01549611932659722, 210.8513442034533227, 62.64886208192143613 ) ) ;
#19548 = EDGE_LOOP ( 'NONE', ( #5136, #5965 ) ) ;
#19549 = CARTESIAN_POINT ( 'NONE',  ( 71.67499999726881299, 168.2552932293087906, -9.630534252274385310 ) ) ;
#19550 = CARTESIAN_POINT ( 'NONE',  ( 4.903702542908435547, 213.8346818373419751, 39.54886208192143471 ) ) ;
#19551 = CIRCLE ( 'NONE', #28272, 32.00000000000000000 ) ;
#19552 = ORIENTED_EDGE ( 'NONE', *, *, #16196, .T. ) ;
#19553 = ADVANCED_FACE ( 'NONE', ( #2601 ), #4008, .T. ) ;
#19554 = CARTESIAN_POINT ( 'NONE',  ( 83.37499999726881583, 155.0000000000000000, -15.58253175000000823 ) ) ;
#19555 = CYLINDRICAL_SURFACE ( 'NONE', #9708, 13.00000000000001776 ) ;
#19556 = DIRECTION ( 'NONE',  ( -0.000000000000000000, -0.000000000000000000, 1.000000000000000000 ) ) ;
#19557 = CARTESIAN_POINT ( 'NONE',  ( -8.015496119326531499, 204.4483345814780364, 57.35113791807857098 ) ) ;
#19558 = EDGE_CURVE ( 'NONE', #26344, #25247, #23059, .T. ) ;
#19559 = CARTESIAN_POINT ( 'NONE',  ( 54.75000000000000000, 7.990820364436479461E-15, 35.00000000000000000 ) ) ;
#19560 = CARTESIAN_POINT ( 'NONE',  ( -6.220909254589682469, 215.4770327129946850, 41.94886208192144039 ) ) ;
#19561 = CARTESIAN_POINT ( 'NONE',  ( 72.17499999726881299, 164.1591823560292198, 12.60653300113718167 ) ) ;
#19562 = ORIENTED_EDGE ( 'NONE', *, *, #27047, .T. ) ;
#19563 = CARTESIAN_POINT ( 'NONE',  ( -52.50000000000002132, 0.000000000000000000, -20.00000000000000000 ) ) ;
#19564 = LINE ( 'NONE', #4054, #19953 ) ;
#19565 = DIRECTION ( 'NONE',  ( -0.000000000000000000, -0.000000000000000000, 1.000000000000000000 ) ) ;
#19566 = CARTESIAN_POINT ( 'NONE',  ( -6.500168698208244500, 211.6636982574061676, 17.79886208192143471 ) ) ;
#19567 = CARTESIAN_POINT ( 'NONE',  ( 0.05014649552810505201, 217.5146222423826714, 64.25113791807856956 ) ) ;
#19568 = CARTESIAN_POINT ( 'NONE',  ( -6.220909254589537696, 198.5229672870051161, 48.05113791807858092 ) ) ;
#19569 = DIRECTION ( 'NONE',  ( 0.000000000000000000, 0.000000000000000000, 1.000000000000000000 ) ) ;
#19570 = CARTESIAN_POINT ( 'NONE',  ( 0.05014649552810505201, 217.5146222423826714, 22.25113791807856956 ) ) ;
#19571 = CARTESIAN_POINT ( 'NONE',  ( -6.500168698208244500, 211.6636982574061676, 98.79886208192142760 ) ) ;
#19572 = CARTESIAN_POINT ( 'NONE',  ( 45.92499999726881299, 164.1591823560292198, 12.60653300113718167 ) ) ;
#19573 = CARTESIAN_POINT ( 'NONE',  ( -4.366061277241453098, 4.984806845751379889, -0.09463688534106590167 ) ) ;
#19574 = DIRECTION ( 'NONE',  ( 0.000000000000000000, 0.000000000000000000, -1.000000000000000000 ) ) ;
#19575 = CARTESIAN_POINT ( 'NONE',  ( -3.753561863808691168, 195.6020594897209435, 23.90113791807857169 ) ) ;
#19576 = AXIS2_PLACEMENT_3D ( 'NONE', #10510, #26328, #17698 ) ;
#19577 = LINE ( 'NONE', #33200, #6997 ) ;
#19578 = CARTESIAN_POINT ( 'NONE',  ( -0.05014649552810635652, 196.4853777576173002, 74.75113791807858377 ) ) ;
#19579 = CARTESIAN_POINT ( 'NONE',  ( -8.062137200540920645, 212.9164362838581894, 42.80113791807857382 ) ) ;
#19580 = CARTESIAN_POINT ( 'NONE',  ( 76.58867513459483689, 146.1832212156128890, -12.13525491562423042 ) ) ;
#19581 = FACE_OUTER_BOUND ( 'NONE', #5512, .T. ) ;
#19582 = CARTESIAN_POINT ( 'NONE',  ( -7.456977232089471386, 217.1783343296987709, 5.948862081921435063 ) ) ;
#19583 = CARTESIAN_POINT ( 'NONE',  ( -0.05014649552828402690, 217.5146222423826714, 15.24886208192143400 ) ) ;
#19584 = CARTESIAN_POINT ( 'NONE',  ( 67.59999999453764019, 141.2096805137202580, -4.480746418436742040 ) ) ;
#19585 = ORIENTED_EDGE ( 'NONE', *, *, #367, .F. ) ;
#19586 = CARTESIAN_POINT ( 'NONE',  ( 12.00000000000000711, 206.9523078486586485, 53.00113791807857666 ) ) ;
#19587 = CARTESIAN_POINT ( 'NONE',  ( 7.984503880673485376, 204.3529502787953902, 71.15113791807857524 ) ) ;
#19588 = ADVANCED_FACE ( 'NONE', ( #5478 ), #15866, .F. ) ;
#19589 = CARTESIAN_POINT ( 'NONE',  ( -9.984503880673420539, 203.7031108863293980, 32.34886208192143187 ) ) ;
#19590 = ADVANCED_FACE ( 'NONE', ( #23381 ), #8211, .T. ) ;
#19591 = ORIENTED_EDGE ( 'NONE', *, *, #18891, .F. ) ;
#19592 = SHAPE_REPRESENTATION ( 'air chamber shell rear', ( #2404 ), #33431 ) ;
#19593 = CARTESIAN_POINT ( 'NONE',  ( 8.118202686958039038, 212.8392687619912635, 88.70113791807857240 ) ) ;
#19594 = EDGE_CURVE ( 'NONE', #25466, #26702, #29319, .T. ) ;
#19595 = ORIENTED_EDGE ( 'NONE', *, *, #1435, .T. ) ;
#19596 = ADVANCED_FACE ( 'NONE', ( #29478 ), #24708, .F. ) ;
#19597 = DIRECTION ( 'NONE',  ( -1.000000000000000000, 0.000000000000000000, 0.000000000000000000 ) ) ;
#19598 = CARTESIAN_POINT ( 'NONE',  ( 2.832728918602883006, 6.234773369952725020, -6.171481112545252223 ) ) ;
#19599 = ORIENTED_EDGE ( 'NONE', *, *, #13973, .F. ) ;
#19600 = CARTESIAN_POINT ( 'NONE',  ( -0.05014649552807731031, 198.5883022060938572, 20.75113791807856600 ) ) ;
#19601 = CARTESIAN_POINT ( 'NONE',  ( 102.4138169258850581, 155.0000000000000000, 32.10452846326769816 ) ) ;
#19602 = CARTESIAN_POINT ( 'NONE',  ( -3.135527875058982783, 216.4958274776886924, 3.098862081921434974 ) ) ;
#19603 = CARTESIAN_POINT ( 'NONE',  ( 51.87499999726880873, 171.3844434931184253, -7.942151717890134290E-15 ) ) ;
#19604 = EDGE_LOOP ( 'NONE', ( #7918, #7451, #19174, #19128 ) ) ;
#19605 = CARTESIAN_POINT ( 'NONE',  ( 6.444103211791042618, 202.2591342207267644, 53.30113791807858092 ) ) ;
#19606 = DIRECTION ( 'NONE',  ( -0.000000000000000000, -0.000000000000000000, 1.000000000000000000 ) ) ;
#19607 = CARTESIAN_POINT ( 'NONE',  ( 0.000000000000000000, 0.000000000000000000, -8.000000000000000000 ) ) ;
#19608 = CARTESIAN_POINT ( 'NONE',  ( 8.118202686958138514, 201.1607312380088501, 91.29886208192144181 ) ) ;
#19609 = CARTESIAN_POINT ( 'NONE',  ( 60.97499999726881015, 140.1801316387863778, -4.815267126137194431 ) ) ;
#19610 = CARTESIAN_POINT ( 'NONE',  ( -0.05014649552810635652, 196.4853777576173002, 29.75113791807856956 ) ) ;
#19611 = FACE_OUTER_BOUND ( 'NONE', #11959, .T. ) ;
#19612 = CARTESIAN_POINT ( 'NONE',  ( 6.139770520408368348, 198.4640165459539674, 14.45113791807856352 ) ) ;
#19613 = CARTESIAN_POINT ( 'NONE',  ( 132.3999999999999773, 261.0000000000000000, 0.000000000000000000 ) ) ;
#19614 = AXIS2_PLACEMENT_3D ( 'NONE', #16157, #27897, #22618 ) ;
#19615 = CARTESIAN_POINT ( 'NONE',  ( 78.79999999999999716, 167.3344367211045096, -8.961492836873482304 ) ) ;
#19616 = CARTESIAN_POINT ( 'NONE',  ( -56.25402757683428234, 194.9848779240976171, -1.110136720165091129 ) ) ;
#19617 = CARTESIAN_POINT ( 'NONE',  ( 100.3117322205716420, 155.0000000000000000, 0.000000000000000000 ) ) ;
#19618 = CARTESIAN_POINT ( 'NONE',  ( -3.135527875058821579, 197.5041725223112223, 95.90113791807858945 ) ) ;
#19619 = DIRECTION ( 'NONE',  ( 0.000000000000000000, 0.000000000000000000, 1.000000000000000000 ) ) ;
#19620 = CARTESIAN_POINT ( 'NONE',  ( 45.17499999726881299, 145.8408176439707802, -12.60653300113719588 ) ) ;
#19621 = CARTESIAN_POINT ( 'NONE',  ( 6.139770520408368348, 198.4640165459539674, 38.45113791807855819 ) ) ;
#19622 = CARTESIAN_POINT ( 'NONE',  ( 81.42499999726882720, 168.2552932293087906, -9.630534252274385310 ) ) ;
#19623 = DIRECTION ( 'NONE',  ( -0.7071067811865331398, 8.659560562355110352E-17, -0.7071067811865620056 ) ) ;
#19624 = DIRECTION ( 'NONE',  ( 0.000000000000000000, 0.000000000000000000, 1.000000000000000000 ) ) ;
#19625 = CARTESIAN_POINT ( 'NONE',  ( 47.99999999453762456, 155.0000000000000000, -14.50000000000000711 ) ) ;
#19626 = VERTEX_POINT ( 'NONE', #6132 ) ;
#19627 = CARTESIAN_POINT ( 'NONE',  ( 12.01549611932652972, 210.8513442034534933, 22.85113791807856742 ) ) ;
#19628 = CARTESIAN_POINT ( 'NONE',  ( 61.01132485994282462, 142.2402378747194405, 9.270509831248432420 ) ) ;
#19629 = DIRECTION ( 'NONE',  ( 0.000000000000000000, 0.000000000000000000, -1.000000000000000000 ) ) ;
#19630 = ORIENTED_EDGE ( 'NONE', *, *, #9517, .T. ) ;
#19631 = CARTESIAN_POINT ( 'NONE',  ( -7.375838497908014268, 196.7627149292498530, 44.04886208192143471 ) ) ;
#19632 = CARTESIAN_POINT ( 'NONE',  ( -8.118202686958039038, 201.1607312380087080, 3.201137918078566180 ) ) ;
#19633 = CARTESIAN_POINT ( 'NONE',  ( 9.984503880673470277, 203.7031108863295401, 62.15113791807856813 ) ) ;
#19634 = CARTESIAN_POINT ( 'NONE',  ( 4.984841277089891776, 200.2242689037093726, 13.44886208192143684 ) ) ;
#19635 = CIRCLE ( 'NONE', #24521, 7.500000000000015099 ) ;
#19636 = UNCERTAINTY_MEASURE_WITH_UNIT (LENGTH_MEASURE( 1.000000000000000082E-05 ), #22758, 'distance_accuracy_value', 'NONE');
#19637 = CARTESIAN_POINT ( 'NONE',  ( 79.08867513459483689, 167.7597621252805880, -9.270509831248443078 ) ) ;
#19638 = AXIS2_PLACEMENT_3D ( 'NONE', #27392, #29958, #20235 ) ;
#19639 = ORIENTED_EDGE ( 'NONE', *, *, #20177, .F. ) ;
#19640 = CARTESIAN_POINT ( 'NONE',  ( 8.015496119326595448, 204.4483345814782638, 97.14886208192146455 ) ) ;
#19641 = B_SPLINE_CURVE_WITH_KNOTS ( 'NONE', 3,
 ( #27572, #1020, #24523, #4072, #3740, #32184 ),
 .UNSPECIFIED., .F., .F.,
 ( 4, 2, 4 ),
 ( 2.380727408984196306E-07, 0.008032766472079773054, 0.01606529487141864984 ),
 .UNSPECIFIED. ) ;
#19642 = LINE ( 'NONE', #32580, #25188 ) ;
#19643 = CARTESIAN_POINT ( 'NONE',  ( -8.000000000000008882, 207.0476921513413515, 36.50113791807857666 ) ) ;
#19644 = CARTESIAN_POINT ( 'NONE',  ( 34.07499999726880446, 168.2552932293087906, 9.630534252274372875 ) ) ;
#19645 = ORIENTED_EDGE ( 'NONE', *, *, #31660, .T. ) ;
#19646 = CARTESIAN_POINT ( 'NONE',  ( 38.02499999726881441, 160.0630714827496206, 15.58253174999999402 ) ) ;
#19647 = CARTESIAN_POINT ( 'NONE',  ( 39.58867513459482268, 163.8167787843871110, 12.13525491562421621 ) ) ;
#19648 = CARTESIAN_POINT ( 'NONE',  ( 8.062137200540920645, 201.0835637161417822, -0.6988620819214342861 ) ) ;
#19649 = CARTESIAN_POINT ( 'NONE',  ( -0.05014649552828403384, 217.5146222423826714, 66.24886208192143044 ) ) ;
#19650 = CARTESIAN_POINT ( 'NONE',  ( 37.97499999726881015, 169.8198683612136222, 4.815267126137181997 ) ) ;
#19651 = DIRECTION ( 'NONE',  ( -1.000000000000000000, -0.000000000000000000, -0.000000000000000000 ) ) ;
#19652 = CARTESIAN_POINT ( 'NONE',  ( -6.220909254589537696, 198.5229672870051161, 3.051137918078564937 ) ) ;
#19653 = CARTESIAN_POINT ( 'NONE',  ( 59.70000000000000284, 146.4771138417591203, 11.73074641843673227 ) ) ;
#19654 = CARTESIAN_POINT ( 'NONE',  ( -31.74999999999995737, 0.000000000000000000, 0.000000000000000000 ) ) ;
#19655 = CARTESIAN_POINT ( 'NONE',  ( 6.444103211790928043, 211.7408657792734061, 78.69886208192143329 ) ) ;
#19656 = DIRECTION ( 'NONE',  ( 1.000000000000000000, -0.000000000000000000, -0.000000000000000000 ) ) ;
#19657 = DIRECTION ( 'NONE',  ( 0.000000000000000000, -0.04769215134144040580, 0.9988620819214356628 ) ) ;
#19658 = CARTESIAN_POINT ( 'NONE',  ( 65.72499999726881015, 169.8198683612136222, 4.815267126137181997 ) ) ;
#19660 = ORIENTED_EDGE ( 'NONE', *, *, #25199, .F. ) ;
#19659 = CARTESIAN_POINT ( 'NONE',  ( -9.984503880673475606, 210.2968891136704315, 24.65113791807856458 ) ) ;
#19661 = LINE ( 'NONE', #30051, #26595 ) ;
#19662 = CIRCLE ( 'NONE', #29453, 32.10452846326766974 ) ;
#19663 = CARTESIAN_POINT ( 'NONE',  ( 86.07499999726880446, 168.2552932293087906, 9.630534252274372875 ) ) ;
#19664 = CARTESIAN_POINT ( 'NONE',  ( 11.98450388067348271, 203.0532714938637753, 89.15113791807856103 ) ) ;
#19665 = CARTESIAN_POINT ( 'NONE',  ( 42.78867513459481842, 155.0000000000000000, -15.00000000000002487 ) ) ;
#19666 = ORIENTED_EDGE ( 'NONE', *, *, #5524, .F. ) ;
#19667 = CARTESIAN_POINT ( 'NONE',  ( -3.753561863808878130, 218.3979405102790281, 69.09886208192143897 ) ) ;
#19668 = CARTESIAN_POINT ( 'NONE',  ( -6.220909254589682469, 215.4770327129947134, 74.94886208192143329 ) ) ;
#19669 = CARTESIAN_POINT ( 'NONE',  ( 9.736236675708031640, 199.9851607334238963, 16.29886208192143471 ) ) ;
#19670 = DIRECTION ( 'NONE',  ( 0.000000000000000000, 0.000000000000000000, -1.000000000000000000 ) ) ;
#19671 = CARTESIAN_POINT ( 'NONE',  ( 3.135527875058820690, 216.4958274776887492, 34.40113791807856813 ) ) ;
#19672 = CARTESIAN_POINT ( 'NONE',  ( -56.00000000000002132, 209.9999999999999716, 0.000000000000000000 ) ) ;
#19673 = CARTESIAN_POINT ( 'NONE',  ( -6.139770520408224463, 198.4640165459539389, 89.04886208192139918 ) ) ;
#19674 = CARTESIAN_POINT ( 'NONE',  ( 63.11132485994280472, 140.7341522555726669, 4.635254915624211769 ) ) ;
#19675 = EDGE_LOOP ( 'NONE', ( #28022, #33257, #8050, #30633 ) ) ;
#19676 = CARTESIAN_POINT ( 'NONE',  ( -9.945352646237287431, 205.9548993908332193, 104.4520571433695579 ) ) ;
#19677 = CARTESIAN_POINT ( 'NONE',  ( -6.444103211790928043, 202.2591342207265939, 74.19886208192143329 ) ) ;
#19678 = ORIENTED_EDGE ( 'NONE', *, *, #12425, .T. ) ;
#19679 = ADVANCED_FACE ( 'NONE', ( #3913 ), #27425, .T. ) ;
#19680 = CARTESIAN_POINT ( 'NONE',  ( 86.72499999726882436, 140.1801316387863778, -4.815267126137194431 ) ) ;
#19681 = VERTEX_POINT ( 'NONE', #24202 ) ;
#19682 = CARTESIAN_POINT ( 'NONE',  ( 68.88867513459483405, 159.8737954434937478, -14.99999999999993072 ) ) ;
#19683 = CARTESIAN_POINT ( 'NONE',  ( 73.52499999726882152, 169.8198683612136222, -4.815267126137197984 ) ) ;
#19684 = CARTESIAN_POINT ( 'NONE',  ( 13.75000000000000888, -23.81569860407206463, -18.00000000000000000 ) ) ;
#19685 = CARTESIAN_POINT ( 'NONE',  ( 8.000000000000008882, 206.9523078486586485, 74.00113791807856956 ) ) ;
#19686 = CARTESIAN_POINT ( 'NONE',  ( 75.58867513459482268, 163.8167787843871110, 12.13525491562421621 ) ) ;
#19688 = CIRCLE ( 'NONE', #17499, 17.00000000000000711 ) ;
#19687 = FILL_AREA_STYLE_COLOUR ( '', #23047 ) ;
#19689 = CARTESIAN_POINT ( 'NONE',  ( 44.40000000000000568, 150.2886644046228639, -14.50000000000000888 ) ) ;
#19690 = CARTESIAN_POINT ( 'NONE',  ( 4.903702542908435547, 213.8346818373419751, 51.54886208192144181 ) ) ;
#19691 = DIRECTION ( 'NONE',  ( -1.000000000000000000, -0.000000000000000000, -0.000000000000000000 ) ) ;
#19692 = CARTESIAN_POINT ( 'NONE',  ( 32.50000000000000000, 155.0000000000000000, 15.00000000000001243 ) ) ;
#19693 = LINE ( 'NONE', #24809, #25131 ) ;
#19694 = CARTESIAN_POINT ( 'NONE',  ( 49.92499999726881299, 164.1591823560292198, 12.60653300113718167 ) ) ;
#19695 = CARTESIAN_POINT ( 'NONE',  ( 65.87499999726880162, 171.3844434931184253, -7.942151717890132712E-15 ) ) ;
#19696 = CARTESIAN_POINT ( 'NONE',  ( 7.456977232089302632, 217.1783343296989131, 58.55113791807858092 ) ) ;
#19697 = FACE_OUTER_BOUND ( 'NONE', #20898, .T. ) ;
#19698 = CARTESIAN_POINT ( 'NONE',  ( -0.05014649552807705357, 194.3824533091408000, 2.751137918078565114 ) ) ;
#19699 = CARTESIAN_POINT ( 'NONE',  ( 10.00000000000000711, 206.9523078486586201, 74.00113791807858377 ) ) ;
#19700 = CARTESIAN_POINT ( 'NONE',  ( 9.736236675708031640, 199.9851607334238963, 40.29886208192143471 ) ) ;
#19701 =( GEOMETRIC_REPRESENTATION_CONTEXT ( 3 ) GLOBAL_UNCERTAINTY_ASSIGNED_CONTEXT ( ( #6692 ) ) GLOBAL_UNIT_ASSIGNED_CONTEXT ( ( #18688, #5893, #21237 ) ) REPRESENTATION_CONTEXT ( 'NONE', 'WORKASPACE' ) );
#19702 = CARTESIAN_POINT ( 'NONE',  ( 3.135527875058981895, 197.5041725223112792, 49.59886208192143897 ) ) ;
#19703 = CARTESIAN_POINT ( 'NONE',  ( 87.49999999453764588, 139.7537977485451393, -4.138211985947621020E-15 ) ) ;
#19704 = CARTESIAN_POINT ( 'NONE',  ( 12.00000000000000711, 206.9523078486586485, 86.00113791807856956 ) ) ;
#19705 = CARTESIAN_POINT ( 'NONE',  ( -6.500168698208129925, 202.3363017425936050, 96.20113791807858661 ) ) ;
#19706 = CARTESIAN_POINT ( 'NONE',  ( 9.984503880673420539, 210.2968891136705167, 60.84886208192142476 ) ) ;
#19707 = ORIENTED_EDGE ( 'NONE', *, *, #33460, .T. ) ;
#19708 = CARTESIAN_POINT ( 'NONE',  ( -9.736236675708031640, 214.0148392665760753, 68.79886208192144181 ) ) ;
#19709 = AXIS2_PLACEMENT_3D ( 'NONE', #30084, #19691, #32636 ) ;
#19710 = ORIENTED_EDGE ( 'NONE', *, *, #28744, .T. ) ;
#19711 = CARTESIAN_POINT ( 'NONE',  ( 69.17499999726881299, 145.8408176439707802, -12.60653300113719588 ) ) ;
#19712 = CARTESIAN_POINT ( 'NONE',  ( 8.000000000000008882, 207.0476921513415220, 39.99886208192145176 ) ) ;
#19713 = CIRCLE ( 'NONE', #5038, 27.99999999999999645 ) ;
#19714 = ORIENTED_EDGE ( 'NONE', *, *, #6868, .F. ) ;
#19715 = ADVANCED_FACE ( 'NONE', ( #8699 ), #3583, .F. ) ;
#19716 = CARTESIAN_POINT ( 'NONE',  ( 84.77499999726880731, 140.1801316387863778, 4.815267126137185549 ) ) ;
#19717 = FACE_BOUND ( 'NONE', #17279, .T. ) ;
#19718 = CARTESIAN_POINT ( 'NONE',  ( 1.517883041479706208E-15, 4.041451884327390331, -0.3126073911696551910 ) ) ;
#19719 = CARTESIAN_POINT ( 'NONE',  ( 4.984841277089725686, 213.7757310962907411, 61.55113791807858092 ) ) ;
#19720 = DIRECTION ( 'NONE',  ( 0.5000000000000005551, -0.8660254037844383745, 0.000000000000000000 ) ) ;
#19721 = CARTESIAN_POINT ( 'NONE',  ( 6.139770520408223575, 215.5359834540460611, 39.54886208192143471 ) ) ;
#19722 = ORIENTED_EDGE ( 'NONE', *, *, #27084, .F. ) ;
#19723 = DIRECTION ( 'NONE',  ( 1.000000000000000000, 0.000000000000000000, 0.000000000000000000 ) ) ;
#19724 = EDGE_CURVE ( 'NONE', #25792, #31511, #16866, .T. ) ;
#19725 = PRODUCT_DEFINITION_FORMATION_WITH_SPECIFIED_SOURCE ( 'ANY', '', #33103, .NOT_KNOWN. ) ;
#19726 =( LENGTH_UNIT ( ) NAMED_UNIT ( * ) SI_UNIT ( .MILLI., .METRE. ) );
#19727 = DIRECTION ( 'NONE',  ( 0.000000000000000000, 0.000000000000000000, -1.000000000000000000 ) ) ;
#19728 = CARTESIAN_POINT ( 'NONE',  ( 85.81132485994280046, 159.8737954434936057, -15.00000000000002665 ) ) ;
#19729 = CARTESIAN_POINT ( 'NONE',  ( 4.984841277089891776, 200.2242689037093726, 22.44886208192143329 ) ) ;
#19730 = CARTESIAN_POINT ( 'NONE',  ( -9.984503880673473830, 210.2968891136704315, 63.65113791807857524 ) ) ;
#19731 = CARTESIAN_POINT ( 'NONE',  ( 6.139770520408368348, 198.4640165459539674, 44.45113791807855819 ) ) ;
#19732 = CARTESIAN_POINT ( 'NONE',  ( 67.68867513459483121, 159.8737954434934352, 15.00000000000015277 ) ) ;
#19733 = CONTEXT_DEPENDENT_SHAPE_REPRESENTATION ( #1808, #3555 ) ;
#19734 = CARTESIAN_POINT ( 'NONE',  ( 10.01549611932653860, 210.2015048109876716, 19.85113791807856387 ) ) ;
#19735 = CARTESIAN_POINT ( 'NONE',  ( 7.984503880673485376, 204.3529502787953902, 5.151137918078566358 ) ) ;
#19736 = AXIS2_PLACEMENT_3D ( 'NONE', #21012, #33292, #7912 ) ;
#19737 = CARTESIAN_POINT ( 'NONE',  ( 43.92499999726881299, 164.1591823560292198, 12.60653300113718167 ) ) ;
#19738 = CARTESIAN_POINT ( 'NONE',  ( -52.50000000000002132, -95.00000000000000000, 20.00000000000001776 ) ) ;
#19739 = CARTESIAN_POINT ( 'NONE',  ( 87.50000000000001421, 157.3337595323334028, -15.27490146385892267 ) ) ;
#19740 = CARTESIAN_POINT ( 'NONE',  ( 9.680171189290831535, 199.9079932115568852, 26.30113791807856316 ) ) ;
#19741 = DIRECTION ( 'NONE',  ( -0.000000000000000000, -0.000000000000000000, 1.000000000000000000 ) ) ;
#19742 = EDGE_CURVE ( 'NONE', #23586, #21522, #33422, .T. ) ;
#19743 = CARTESIAN_POINT ( 'NONE',  ( 8.118202686958039038, 212.8392687619912635, 73.70113791807857240 ) ) ;
#19744 = CARTESIAN_POINT ( 'NONE',  ( -0.05014649552810635652, 196.4853777576173002, 44.75113791807856956 ) ) ;
#19745 = CARTESIAN_POINT ( 'NONE',  ( -64.96121601855533356, 1.809269760319424769, -19.53878398144470907 ) ) ;
#19746 = CARTESIAN_POINT ( 'NONE',  ( 0.000000000000000000, 0.000000000000000000, -20.00000000000000000 ) ) ;
#19747 = CARTESIAN_POINT ( 'NONE',  ( 7.375838497908012492, 217.2372850707501186, 12.54886208192143826 ) ) ;
#19748 = CARTESIAN_POINT ( 'NONE',  ( 9.984503880673420539, 210.2968891136705736, 15.84886208192143719 ) ) ;
#19749 = CARTESIAN_POINT ( 'NONE',  ( 68.39999999453763735, 168.7903194862797420, -4.480746418436745593 ) ) ;
#19750 = ORIENTED_EDGE ( 'NONE', *, *, #17637, .F. ) ;
#19751 = CARTESIAN_POINT ( 'NONE',  ( -7.456977232089304408, 196.8216656703010301, 60.05113791807858092 ) ) ;
#19752 = CARTESIAN_POINT ( 'NONE',  ( 6.500168698208129925, 211.6636982574063381, 64.70113791807857240 ) ) ;
#19753 = EDGE_CURVE ( 'NONE', #19681, #9541, #14144, .T. ) ;
#19754 = CARTESIAN_POINT ( 'NONE',  ( 3.135527875058981895, 197.5041725223112792, 34.59886208192143897 ) ) ;
#19755 = CARTESIAN_POINT ( 'NONE',  ( 45.21132485994280614, 139.2280666364260071, -4.041636747397287284E-15 ) ) ;
#19756 = EDGE_LOOP ( 'NONE', ( #11762, #9973 ) ) ;
#19757 = AXIS2_PLACEMENT_3D ( 'NONE', #5294, #30698, #15686 ) ;
#19758 = CARTESIAN_POINT ( 'NONE',  ( -9.984503880673473830, 210.2968891136704315, 90.65113791807854682 ) ) ;
#19759 = ORIENTED_EDGE ( 'NONE', *, *, #18867, .T. ) ;
#19760 = CARTESIAN_POINT ( 'NONE',  ( 41.78867513459481842, 155.0000000000000000, 15.00000000000001243 ) ) ;
#19761 = DIRECTION ( 'NONE',  ( -1.000000000000000000, 0.000000000000000000, 0.000000000000000000 ) ) ;
#19762 = VERTEX_POINT ( 'NONE', #16193 ) ;
#19763 = AXIS2_PLACEMENT_3D ( 'NONE', #13571, #23961, #29242 ) ;
#19764 = CARTESIAN_POINT ( 'NONE',  ( 0.05014649552807626948, 215.4116977939061144, 37.25113791807857666 ) ) ;
#19765 = CIRCLE ( 'NONE', #27394, 5.000000000000000888 ) ;
#19766 = DIRECTION ( 'NONE',  ( 1.224646799147353207E-16, 1.000000000000000000, 0.000000000000000000 ) ) ;
#19767 = CARTESIAN_POINT ( 'NONE',  ( -8.118202686958138514, 212.8392687619910930, 11.79886208192143471 ) ) ;
#19768 = CIRCLE ( 'NONE', #17584, 7.500000000000015099 ) ;
#19769 = CARTESIAN_POINT ( 'NONE',  ( 59.67499999726880588, 168.2552932293087906, -9.630534252274387086 ) ) ;
#19770 = ORIENTED_EDGE ( 'NONE', *, *, #3784, .T. ) ;
#19771 = CARTESIAN_POINT ( 'NONE',  ( -0.05014649552807731031, 198.5883022060938572, 53.75113791807857666 ) ) ;
#19772 = FACE_OUTER_BOUND ( 'NONE', #16145, .T. ) ;
#19773 = CARTESIAN_POINT ( 'NONE',  ( 0.000000000000000000, -1.759474945355381958, 3.047500000000001208 ) ) ;
#19774 = CARTESIAN_POINT ( 'NONE',  ( 10.01549611932659545, 203.7984951890123853, 103.1488620819214077 ) ) ;
#19775 = CARTESIAN_POINT ( 'NONE',  ( 57.97499999726881015, 169.8198683612136222, 4.815267126137181997 ) ) ;
#19776 = CARTESIAN_POINT ( 'NONE',  ( 3.044812012440130555, 197.4746971517856764, 35.60113791807857098 ) ) ;
#19777 = CARTESIAN_POINT ( 'NONE',  ( 125.0000000000000000, 3.061616997868383121E-14, 35.00200000000000244 ) ) ;
#19778 = EDGE_CURVE ( 'NONE', #22743, #13301, #4030, .T. ) ;
#19779 = ADVANCED_FACE ( 'NONE', ( #21643 ), #8903, .F. ) ;
#19780 = CARTESIAN_POINT ( 'NONE',  ( 0.05014649552810505201, 217.5146222423826714, 13.25113791807856778 ) ) ;
#19781 = DIRECTION ( 'NONE',  ( 0.9237280213470682178, 0.3830490080632377725, 1.131240564625405124E-16 ) ) ;
#19782 = CARTESIAN_POINT ( 'NONE',  ( 77.40000000000000568, 159.7113355953771077, 14.49999999999999289 ) ) ;
#19783 = FILL_AREA_STYLE ('',( #22333 ) ) ;
#19784 = CARTESIAN_POINT ( 'NONE',  ( -68.50000000000000000, 215.0000000000000000, -2.500000000000000000 ) ) ;
#19785 = CARTESIAN_POINT ( 'NONE',  ( -10.01549611932653860, 203.7984951890123284, 102.3511379180785781 ) ) ;
#19786 = CARTESIAN_POINT ( 'NONE',  ( 27.50000000000000355, 0.000000000000000000, -18.00000000000000000 ) ) ;
#19787 = CARTESIAN_POINT ( 'NONE',  ( 43.87499999726880162, 171.3844434931184253, -7.942151717890132712E-15 ) ) ;
#19788 = PRODUCT_RELATED_PRODUCT_CATEGORY ( 'part', '', ( #9707 ) ) ;
#19789 = EDGE_CURVE ( 'NONE', #23693, #4173, #23169, .T. ) ;
#19790 = CARTESIAN_POINT ( 'NONE',  ( -10.01549611932653860, 203.7984951890123284, 42.35113791807855677 ) ) ;
#19791 = CARTESIAN_POINT ( 'NONE',  ( 86.42499999726881299, 141.7447067706911810, 9.630534252274376428 ) ) ;
#19792 = CARTESIAN_POINT ( 'NONE',  ( 34.50000000000000000, -103.0000000000000142, 30.00000000000000000 ) ) ;
#19793 = CYLINDRICAL_SURFACE ( 'NONE', #23865, 40.00000000000000711 ) ;
#19794 = VECTOR ( 'NONE', #30692, 1000.000000000000000 ) ;
#19795 = CARTESIAN_POINT ( 'NONE',  ( 49.69999999453763451, 142.6655632788954620, -8.961492836873480528 ) ) ;
#19796 = ORIENTED_EDGE ( 'NONE', *, *, #23975, .F. ) ;
#19797 = CARTESIAN_POINT ( 'NONE',  ( 0.05014649552807549926, 219.6175466908591716, 31.25113791807856956 ) ) ;
#19798 = AXIS2_PLACEMENT_3D ( 'NONE', #25208, #4085, #20266 ) ;
#19799 = EDGE_CURVE ( 'NONE', #29530, #25373, #32198, .T. ) ;
#19800 = DIRECTION ( 'NONE',  ( 1.000000000000000000, 0.000000000000000000, 0.000000000000000000 ) ) ;
#19801 = DIRECTION ( 'NONE',  ( 0.000000000000000000, 0.000000000000000000, -1.000000000000000000 ) ) ;
#19802 = ORIENTED_EDGE ( 'NONE', *, *, #21939, .T. ) ;
#19803 = CARTESIAN_POINT ( 'NONE',  ( 7.375838497908012492, 217.2372850707501186, 42.54886208192143471 ) ) ;
#19804 = DIRECTION ( 'NONE',  ( 0.000000000000000000, 0.000000000000000000, 1.000000000000000000 ) ) ;
#19805 = CARTESIAN_POINT ( 'NONE',  ( -8.118202686958039038, 201.1607312380087080, 63.20113791807857240 ) ) ;
#19806 = CARTESIAN_POINT ( 'NONE',  ( -2.517493886309087880, 214.5937144450984135, 27.09886208192143897 ) ) ;
#19807 = CARTESIAN_POINT ( 'NONE',  ( 117.5000000000000142, 155.0000000000000000, -6.938893903907228378E-15 ) ) ;
#19808 = ORIENTED_EDGE ( 'NONE', *, *, #9591, .T. ) ;
#19809 = CARTESIAN_POINT ( 'NONE',  ( 4.984841277089725686, 213.7757310962907411, 1.551137918078566047 ) ) ;
#19810 = DIRECTION ( 'NONE',  ( 0.000000000000000000, 0.000000000000000000, -1.000000000000000000 ) ) ;
#19811 = CARTESIAN_POINT ( 'NONE',  ( 0.05014649552828288198, 194.3824533091408000, 85.74886208192143044 ) ) ;
#19812 = PLANE ( 'NONE',  #13519 ) ;
#19813 = ORIENTED_EDGE ( 'NONE', *, *, #2461, .F. ) ;
#19814 = CARTESIAN_POINT ( 'NONE',  ( 38.32499999726881157, 145.8408176439707802, 12.60653300113718345 ) ) ;
#19815 = CARTESIAN_POINT ( 'NONE',  ( -3.379472811782915531E-16, -7.505553499465146494, -6.177805531628540514 ) ) ;
#19816 = CIRCLE ( 'NONE', #11648, 5.249999999999997335 ) ;
#19817 = CARTESIAN_POINT ( 'NONE',  ( -6.220909254589682469, 215.4770327129946850, 59.94886208192141908 ) ) ;
#19818 = CARTESIAN_POINT ( 'NONE',  ( 41.97499999726881015, 169.8198683612136222, 4.815267126137181997 ) ) ;
#19819 = PLANE ( 'NONE',  #25523 ) ;
#19820 = CARTESIAN_POINT ( 'NONE',  ( 8.118202686958039038, 212.8392687619912635, 4.701137918078565292 ) ) ;
#19821 = CARTESIAN_POINT ( 'NONE',  ( -22.99387487948482089, -18.47874495404631290, -1.090893241169168748 ) ) ;
#19822 = CARTESIAN_POINT ( 'NONE',  ( 59.59999999999999432, 150.2886644046228639, 14.49999999999999645 ) ) ;
#19823 = CARTESIAN_POINT ( 'NONE',  ( -2.047034997319599814, -2.859595677584358953, -1.683223872783745003E-14 ) ) ;
#19824 = CARTESIAN_POINT ( 'NONE',  ( -7.984503880673422316, 204.3529502787951628, 83.34886208192143897 ) ) ;
#19825 = CARTESIAN_POINT ( 'NONE',  ( -0.9763930676156993282, 8.096533237421580154, -7.213065638943424673 ) ) ;
#19826 = DIRECTION ( 'NONE',  ( -1.000000000000000000, -0.000000000000000000, -0.000000000000000000 ) ) ;
#19827 = CARTESIAN_POINT ( 'NONE',  ( 3.753561863808876797, 195.6020594897209719, 82.59886208192143897 ) ) ;
#19828 = CARTESIAN_POINT ( 'NONE',  ( 65.02499999726882152, 149.9369285172503510, -15.58253175000000823 ) ) ;
#19830 = ORIENTED_EDGE ( 'NONE', *, *, #14588, .F. ) ;
#19829 = CARTESIAN_POINT ( 'NONE',  ( -10.01549611932653860, 203.7984951890123000, 18.35113791807856742 ) ) ;
#19831 = DIRECTION ( 'NONE',  ( -1.000000000000000000, -0.000000000000000000, -0.000000000000000000 ) ) ;
#19832 = CARTESIAN_POINT ( 'NONE',  ( 80.77499999726880731, 140.1801316387863778, 4.815267126137185549 ) ) ;
#19833 = CARTESIAN_POINT ( 'NONE',  ( -9.736236675707914401, 199.9851607334237542, 87.20113791807858661 ) ) ;
#19834 = CARTESIAN_POINT ( 'NONE',  ( 87.50000000000001421, 155.0000000000000000, -6.938893903907228378E-15 ) ) ;
#19835 = EDGE_LOOP ( 'NONE', ( #2099, #31175, #4837, #21392 ) ) ;
#19836 = CARTESIAN_POINT ( 'NONE',  ( 9.736236675708031640, 199.9851607334238963, 67.29886208192144181 ) ) ;
#19837 = CARTESIAN_POINT ( 'NONE',  ( 6.220909254589680693, 198.5229672870052582, 76.44886208192143329 ) ) ;
#19838 = CARTESIAN_POINT ( 'NONE',  ( -7.375838497908014268, 196.7627149292498530, 11.04886208192143648 ) ) ;
#19839 = DIRECTION ( 'NONE',  ( -1.000000000000000000, 0.000000000000000000, 0.000000000000000000 ) ) ;
#19840 = CARTESIAN_POINT ( 'NONE',  ( -3.135527875058821579, 197.5041725223112223, 29.90113791807856813 ) ) ;
#19841 = CARTESIAN_POINT ( 'NONE',  ( 65.98867513459482836, 146.1832212156128890, 12.13525491562421976 ) ) ;
#19842 = CARTESIAN_POINT ( 'NONE',  ( -6.220909254589682469, 215.4770327129946850, 95.94886208192143329 ) ) ;
#19843 = CARTESIAN_POINT ( 'NONE',  ( 5.589124336233334489, 4.278671059407959554, -6.219623095966918314 ) ) ;
#19844 = ORIENTED_EDGE ( 'NONE', *, *, #9402, .T. ) ;
#19845 = CARTESIAN_POINT ( 'NONE',  ( -1.153701847711675610, -3.375361811986517413, -1.643114763111695053E-14 ) ) ;
#19846 = CARTESIAN_POINT ( 'NONE',  ( 0.05014649552828262524, 198.5883022060938572, 70.74886208192144466 ) ) ;
#19847 = ORIENTED_EDGE ( 'NONE', *, *, #29742, .F. ) ;
#19848 = CARTESIAN_POINT ( 'NONE',  ( 82.02499999726879309, 160.0630714827496206, 15.58253174999999224 ) ) ;
#19849 = VERTEX_POINT ( 'NONE', #26750 ) ;
#19850 = CYLINDRICAL_SURFACE ( 'NONE', #21595, 13.00000000000002487 ) ;
#19851 = CARTESIAN_POINT ( 'NONE',  ( 75.52499999726880731, 169.8198683612136222, -4.815267126137197984 ) ) ;
#19852 = FACE_OUTER_BOUND ( 'NONE', #5070, .T. ) ;
#19853 = CARTESIAN_POINT ( 'NONE',  ( -4.903702542908602524, 213.8346818373418898, 78.95113791807858661 ) ) ;
#19854 = CYLINDRICAL_SURFACE ( 'NONE', #33079, 4.200000000000001954 ) ;
#19855 = CARTESIAN_POINT ( 'NONE',  ( 39.30000000000000426, 163.5228861582408797, 11.73074641843673049 ) ) ;
#19856 = CARTESIAN_POINT ( 'NONE',  ( -4.984841277089891776, 213.7757310962905990, 56.94886208192144039 ) ) ;
#19857 = FACE_BOUND ( 'NONE', #25383, .T. ) ;
#19858 = CARTESIAN_POINT ( 'NONE',  ( -7.922281120364393914, 4.573931137438271399, -8.047472243342930653 ) ) ;
#19859 = CARTESIAN_POINT ( 'NONE',  ( 0.000000000000000000, 0.000000000000000000, 0.000000000000000000 ) ) ;
#19860 = CARTESIAN_POINT ( 'NONE',  ( 53.72499999726881015, 169.8198683612136222, 4.815267126137181997 ) ) ;
#19861 = CARTESIAN_POINT ( 'NONE',  ( 66.87499999726880162, 138.6155565068815463, -3.929120461958505118E-15 ) ) ;
#19862 = CARTESIAN_POINT ( 'NONE',  ( -12.01549611932652972, 203.1486557965464499, 60.35113791807857098 ) ) ;
#19863 = DIRECTION ( 'NONE',  ( 0.000000000000000000, 0.000000000000000000, -1.000000000000000000 ) ) ;
#19864 = CARTESIAN_POINT ( 'NONE',  ( 6.139770520408368348, 198.4640165459539674, 101.4511379180785866 ) ) ;
#19865 = EDGE_CURVE ( 'NONE', #27878, #15105, #10567, .T. ) ;
#19867 = CARTESIAN_POINT ( 'NONE',  ( 8.062137200540920645, 201.0835637161417822, 74.30113791807858092 ) ) ;
#19866 =( REPRESENTATION_RELATIONSHIP ('NONE','NONE', #25663, #30243 ) REPRESENTATION_RELATIONSHIP_WITH_TRANSFORMATION ( #17004 )SHAPE_REPRESENTATION_RELATIONSHIP( ) );
#19868 = CARTESIAN_POINT ( 'NONE',  ( -12.01549611932659722, 210.8513442034533227, 38.64886208192143613 ) ) ;
#19869 = CARTESIAN_POINT ( 'NONE',  ( -3.044812012439970683, 197.4746971517856196, 49.89886208192143613 ) ) ;
#19870 = CARTESIAN_POINT ( 'NONE',  ( 16.00000000000000000, 2.210487472460973191E-16, -1.610000000000000098 ) ) ;
#19871 = CARTESIAN_POINT ( 'NONE',  ( 11.98450388067348271, 203.0532714938637753, 83.15113791807856103 ) ) ;
#19872 = DIRECTION ( 'NONE',  ( 0.000000000000000000, 0.000000000000000000, 1.000000000000000000 ) ) ;
#19873 = CARTESIAN_POINT ( 'NONE',  ( 6.139770520408368348, 198.4640165459539674, 2.451137918078566180 ) ) ;
#19874 = CARTESIAN_POINT ( 'NONE',  ( 10.01549611932659545, 203.7984951890123853, 58.14886208192142192 ) ) ;
#19875 = CARTESIAN_POINT ( 'NONE',  ( 0.6508621380849231031, 8.763657152406445050, -7.907633014911220393 ) ) ;
#19876 = ORIENTED_EDGE ( 'NONE', *, *, #14291, .T. ) ;
#19877 = CARTESIAN_POINT ( 'NONE',  ( -7.375838497908014268, 196.7627149292498530, 74.04886208192142760 ) ) ;
#19878 = EDGE_LOOP ( 'NONE', ( #25850, #16659, #10320, #16562 ) ) ;
#19879 = CARTESIAN_POINT ( 'NONE',  ( 72.37499999726881583, 155.0000000000000000, 15.58253174999999402 ) ) ;
#19880 = CARTESIAN_POINT ( 'NONE',  ( 0.05014649552828262524, 198.5883022060938572, 40.74886208192143755 ) ) ;
#19881 = ORIENTED_EDGE ( 'NONE', *, *, #17951, .F. ) ;
#19882 = CARTESIAN_POINT ( 'NONE',  ( 82.67499999726881299, 141.7447067706911810, 9.630534252274376428 ) ) ;
#19883 = FACE_BOUND ( 'NONE', #25969, .T. ) ;
#19884 = DIRECTION ( 'NONE',  ( -1.000000000000000000, 0.000000000000000000, -0.000000000000000000 ) ) ;
#19885 = DIRECTION ( 'NONE',  ( -1.000000000000000000, 0.000000000000000000, -0.000000000000000000 ) ) ;
#19886 = CARTESIAN_POINT ( 'NONE',  ( 8.062137200540822946, 212.9164362838583315, 39.69886208192143329 ) ) ;
#19887 = VERTEX_POINT ( 'NONE', #9535 ) ;
#19888 = CARTESIAN_POINT ( 'NONE',  ( -14.99999999999998934, -1.734723475976807094E-15, -10.00000000000000000 ) ) ;
#19889 = CARTESIAN_POINT ( 'NONE',  ( 5.619193549421182432, -4.261310591078213861, -5.875704392892080463 ) ) ;
#19890 = ADVANCED_FACE ( 'NONE', ( #25046 ), #7307, .T. ) ;
#19891 = DIRECTION ( 'NONE',  ( 0.9396926207859143121, 1.150791560227857665E-16, -0.3420201433256525592 ) ) ;
#19892 = CARTESIAN_POINT ( 'NONE',  ( 4.984841277089891776, 200.2242689037093726, 25.44886208192143684 ) ) ;
#19893 = CARTESIAN_POINT ( 'NONE',  ( -3.135527875058821579, 197.5041725223112223, 65.90113791807857524 ) ) ;
#19894 = CARTESIAN_POINT ( 'NONE',  ( -8.062137200540920645, 212.9164362838581894, 45.80113791807856671 ) ) ;
#19895 = CYLINDRICAL_SURFACE ( 'NONE', #32464, 6.500000000000000000 ) ;
#19896 = CONTEXT_DEPENDENT_SHAPE_REPRESENTATION ( #23996, #7910 ) ;
#19897 = CARTESIAN_POINT ( 'NONE',  ( -3.044812012440131443, 216.5253028482142952, 19.10113791807856742 ) ) ;
#19898 = CARTESIAN_POINT ( 'NONE',  ( 6.500168698208129925, 211.6636982574063381, 7.701137918078567068 ) ) ;
#19899 = CARTESIAN_POINT ( 'NONE',  ( 44.22499999726880304, 149.9369285172503510, 15.58253174999999580 ) ) ;
#19900 = DIRECTION ( 'NONE',  ( 0.000000000000000000, 0.000000000000000000, -1.000000000000000000 ) ) ;
#19901 = CARTESIAN_POINT ( 'NONE',  ( 87.50000000000002842, 145.7452232778646817, -11.80462230752951136 ) ) ;
#19902 = CARTESIAN_POINT ( 'NONE',  ( 3.753561863808689836, 218.3979405102790565, 28.40113791807856813 ) ) ;
#19903 = CARTESIAN_POINT ( 'NONE',  ( 6.663127973346137267, -3.846958729056325410, -6.460793508093413351 ) ) ;
#19904 = CARTESIAN_POINT ( 'NONE',  ( 3.135527875058820690, 216.4958274776887492, 79.40113791807857524 ) ) ;
#19905 = EDGE_CURVE ( 'NONE', #23990, #22576, #32532, .T. ) ;
#19906 = CARTESIAN_POINT ( 'NONE',  ( -10.01549611932653860, 203.7984951890123000, 48.35113791807857098 ) ) ;
#19907 = CARTESIAN_POINT ( 'NONE',  ( 4.403473400622098133, 6.117907484625861869, 2.043043468777371629E-15 ) ) ;
#19908 = DIRECTION ( 'NONE',  ( -0.9998603841633338929, 0.01669062914075312987, 0.0007969188393214247284 ) ) ;
#19909 = CARTESIAN_POINT ( 'NONE',  ( 12.01549611932659367, 203.1486557965466773, 10.14886208192143435 ) ) ;
#19910 = CARTESIAN_POINT ( 'NONE',  ( -10.00000000000000711, 206.9523078486584495, 17.49886208192143400 ) ) ;
#19911 = CARTESIAN_POINT ( 'NONE',  ( 71.89999999453765156, 150.2886644046228639, -14.50000000000000888 ) ) ;
#19912 = VERTEX_POINT ( 'NONE', #22142 ) ;
#19913 = CARTESIAN_POINT ( 'NONE',  ( 12.00000000000000711, 206.9523078486586485, 62.00113791807856956 ) ) ;
#19914 = CARTESIAN_POINT ( 'NONE',  ( 4.903702542908601636, 200.1653181626581102, 74.45113791807855819 ) ) ;
#19915 = CARTESIAN_POINT ( 'NONE',  ( -8.062137200540822946, 201.0835637161416400, 32.19886208192143329 ) ) ;
#19916 = VECTOR ( 'NONE', #30443, 1000.000000000000000 ) ;
#19917 =( LENGTH_UNIT ( ) NAMED_UNIT ( * ) SI_UNIT ( .MILLI., .METRE. ) );
#19918 = VERTEX_POINT ( 'NONE', #4604 ) ;
#19919 = EDGE_CURVE ( 'NONE', #19336, #734, #13379, .T. ) ;
#19920 = ORIENTED_EDGE ( 'NONE', *, *, #13283, .F. ) ;
#19921 = VERTEX_POINT ( 'NONE', #33218 ) ;
#19922 = B_SPLINE_CURVE_WITH_KNOTS ( 'NONE', 3,
 ( #16279, #8130, #31943, #13714, #8614, #18343 ),
 .UNSPECIFIED., .F., .F.,
 ( 4, 2, 4 ),
 ( 0.002044882221487550125, 0.003063384235218505856, 0.004081886248949461587 ),
 .UNSPECIFIED. ) ;
#19923 = DIRECTION ( 'NONE',  ( 0.000000000000000000, 0.000000000000000000, -1.000000000000000000 ) ) ;
#19924 = LINE ( 'NONE', #9883, #17096 ) ;
#19925 = EDGE_LOOP ( 'NONE', ( #6260, #9285, #30071, #11851, #16058 ) ) ;
#19926 = CARTESIAN_POINT ( 'NONE',  ( -8.015496119326531499, 204.4483345814780364, 30.35113791807856742 ) ) ;
#19927 = B_SPLINE_CURVE_WITH_KNOTS ( 'NONE', 3,
 ( #17262, #19823, #4661, #17604, #2113, #32935 ),
 .UNSPECIFIED., .F., .F.,
 ( 4, 2, 4 ),
 ( 0.002044882221487580917, 0.003063384235218526673, 0.004081886248949471996 ),
 .UNSPECIFIED. ) ;
#19928 = EDGE_CURVE ( 'NONE', #28610, #19887, #24871, .T. ) ;
#19929 = CARTESIAN_POINT ( 'NONE',  ( 85.41132485994282320, 142.2402378747194405, -9.270509831248439525 ) ) ;
#19930 = CARTESIAN_POINT ( 'NONE',  ( -10.00000000000000711, 206.9523078486584495, 17.49886208192143400 ) ) ;
#19931 = CARTESIAN_POINT ( 'NONE',  ( 55.17499999726881299, 145.8408176439707802, -12.60653300113719588 ) ) ;
#19932 = ORIENTED_EDGE ( 'NONE', *, *, #29987, .T. ) ;
#19933 = CARTESIAN_POINT ( 'NONE',  ( 2.517493886308900919, 214.5937144450984420, 46.40113791807856813 ) ) ;
#19934 = CARTESIAN_POINT ( 'NONE',  ( 32.50000000000000000, 155.0000000000000000, 15.00000000000001243 ) ) ;
#19935 =( LENGTH_UNIT ( ) NAMED_UNIT ( * ) SI_UNIT ( .MILLI., .METRE. ) );
#19936 = CARTESIAN_POINT ( 'NONE',  ( 56.81132485994281467, 150.1262045565064227, 15.00000000000001599 ) ) ;
#19937 = CARTESIAN_POINT ( 'NONE',  ( -10.05084501415679732, 217.6133941545940047, 104.9910338291041683 ) ) ;
#19938 = ADVANCED_FACE ( 'NONE', ( #1699, #6647 ), #9710, .T. ) ;
#19939 = CARTESIAN_POINT ( 'NONE',  ( 64.27499999726880731, 160.0630714827496206, 15.58253174999999402 ) ) ;
#19940 = CARTESIAN_POINT ( 'NONE',  ( -9.984503880673473830, 210.2968891136704315, 36.65113791807855392 ) ) ;
#19941 = CARTESIAN_POINT ( 'NONE',  ( -6.831979103402614051, -3.295157223185839701, -6.443785395948805395 ) ) ;
#19942 = CARTESIAN_POINT ( 'NONE',  ( 0.05014649552810505201, 217.5146222423826714, 19.25113791807856600 ) ) ;
#19943 = AXIS2_PLACEMENT_3D ( 'NONE', #28485, #23535, #15194 ) ;
#19944 = DIRECTION ( 'NONE',  ( 0.000000000000000000, -6.982962677686266711E-15, -1.000000000000000000 ) ) ;
#19945 = CARTESIAN_POINT ( 'NONE',  ( 82.40000000000000568, 150.2886644046228639, -14.50000000000000888 ) ) ;
#19946 =( NAMED_UNIT ( * ) SI_UNIT ( $, .STERADIAN. ) SOLID_ANGLE_UNIT ( ) );
#19947 = CARTESIAN_POINT ( 'NONE',  ( 105.9028607166213192, 155.0000000000000000, 0.000000000000000000 ) ) ;
#19948 = CARTESIAN_POINT ( 'NONE',  ( 9.680171189290831535, 199.9079932115568852, -0.6988620819214345081 ) ) ;
#19949 = CARTESIAN_POINT ( 'NONE',  ( 27.50000000000001776, -15.87713240271472870, -2.456200930618646971 ) ) ;
#19950 = CARTESIAN_POINT ( 'NONE',  ( 49.57499999726881157, 164.1591823560292198, -12.60653300113719766 ) ) ;
#19951 = CARTESIAN_POINT ( 'NONE',  ( -10.00000000000000711, 207.0476921513413515, 48.50113791807856956 ) ) ;
#19952 = EDGE_CURVE ( 'NONE', #32104, #33208, #19924, .T. ) ;
#19953 = VECTOR ( 'NONE', #13325, 1000.000000000000000 ) ;
#19954 = CARTESIAN_POINT ( 'NONE',  ( 82.92499999726882720, 145.8408176439707802, -12.60653300113719588 ) ) ;
#19955 = CARTESIAN_POINT ( 'NONE',  ( 2.000000000000000000, 0.000000000000000000, 0.000000000000000000 ) ) ;
#19956 = CARTESIAN_POINT ( 'NONE',  ( 0.000000000000000000, 1.759474945355380404, -3.047500000000001652 ) ) ;
#19957 = CARTESIAN_POINT ( 'NONE',  ( 50.59999999453762598, 168.7903194862797420, 4.480746418436729606 ) ) ;
#19958 = ORIENTED_EDGE ( 'NONE', *, *, #17375, .T. ) ;
#19959 = CARTESIAN_POINT ( 'NONE',  ( -12.00000000000000711, 207.0476921513413515, 30.50113791807856600 ) ) ;
#19960 = DIRECTION ( 'NONE',  ( -1.000000000000000000, -0.000000000000000000, -0.000000000000000000 ) ) ;
#19961 = CARTESIAN_POINT ( 'NONE',  ( -7.456977232089471386, 217.1783343296987709, 101.9488620819214475 ) ) ;
#19962 = CARTESIAN_POINT ( 'NONE',  ( 65.81132485994281467, 159.8737954434934920, -15.00000000000012434 ) ) ;
#19963 = EDGE_LOOP ( 'NONE', ( #6082, #3752, #27927 ) ) ;
#19964 = CARTESIAN_POINT ( 'NONE',  ( 10.00000000000000711, 206.9523078486586201, 65.00113791807856956 ) ) ;
#19965 = CARTESIAN_POINT ( 'NONE',  ( -0.05014649552828365914, 215.4116977939061144, 21.24886208192143755 ) ) ;
#19966 = ADVANCED_FACE ( 'NONE', ( #17034 ), #12095, .T. ) ;
#19967 = CIRCLE ( 'NONE', #5284, 12.10452846326767684 ) ;
#19968 = CARTESIAN_POINT ( 'NONE',  ( 125.5000000000000000, 261.0000000000000000, 0.000000000000000000 ) ) ;
#19969 = ORIENTED_EDGE ( 'NONE', *, *, #6818, .T. ) ;
#19970 = CARTESIAN_POINT ( 'NONE',  ( -6.444103211791042618, 211.7408657792732356, 3.801137918078566269 ) ) ;
#19971 = EDGE_CURVE ( 'NONE', #866, #27344, #8396, .T. ) ;
#19972 = CARTESIAN_POINT ( 'NONE',  ( -2.452879891156814818, -7.244083172395189507, -0.1007566405101857632 ) ) ;
#19973 = CARTESIAN_POINT ( 'NONE',  ( -9.736236675708031640, 214.0148392665760753, 86.79886208192142760 ) ) ;
#19974 = CARTESIAN_POINT ( 'NONE',  ( 37.67499999726881299, 168.2552932293087906, -9.630534252274387086 ) ) ;
#19976 = ORIENTED_EDGE ( 'NONE', *, *, #31797, .F. ) ;
#19975 = AXIS2_PLACEMENT_3D ( 'NONE', #22237, #21895, #6400 ) ;
#19977 = CARTESIAN_POINT ( 'NONE',  ( 47.42499999726879878, 168.2552932293087906, -9.630534252274385310 ) ) ;
#19978 = CARTESIAN_POINT ( 'NONE',  ( -67.50000000000000000, 122.1366465496900418, -17.00000000000001421 ) ) ;
#19979 = CARTESIAN_POINT ( 'NONE',  ( 54.31132485994280756, 169.2658477444273331, 4.635254915624208216 ) ) ;
#19980 = CARTESIAN_POINT ( 'NONE',  ( 8.062137200540822946, 212.9164362838583315, 72.69886208192143329 ) ) ;
#19981 = EDGE_CURVE ( 'NONE', #22066, #21727, #17069, .T. ) ;
#19982 = CARTESIAN_POINT ( 'NONE',  ( 45.17499999726881299, 145.8408176439707802, -12.60653300113719588 ) ) ;
#19983 = CARTESIAN_POINT ( 'NONE',  ( 1.750000000000012879, 3.031088913245524097, 1.502314598737187430E-15 ) ) ;
#19984 = CARTESIAN_POINT ( 'NONE',  ( 3.135527875058820690, 216.4958274776887492, 7.401137918078566358 ) ) ;
#19985 = FACE_OUTER_BOUND ( 'NONE', #25723, .T. ) ;
#19986 = CARTESIAN_POINT ( 'NONE',  ( 61.90000000000000568, 141.2096805137202580, 4.480746418436733158 ) ) ;
#19987 = CARTESIAN_POINT ( 'NONE',  ( -10.01549611932653860, 203.7984951890123284, 87.35113791807854966 ) ) ;
#19988 = CYLINDRICAL_SURFACE ( 'NONE', #27825, 5.000000000000001776 ) ;
#19989 = CARTESIAN_POINT ( 'NONE',  ( 8.000000000000008882, 207.0476921513415220, 78.99886208192144466 ) ) ;
#19990 = AXIS2_PLACEMENT_3D ( 'NONE', #17506, #30463, #4216 ) ;
#19991 = DIRECTION ( 'NONE',  ( 0.000000000000000000, 0.000000000000000000, -1.000000000000000000 ) ) ;
#19992 = DIRECTION ( 'NONE',  ( 0.000000000000000000, -0.4999999999999994449, 0.8660254037844389297 ) ) ;
#19993 = CARTESIAN_POINT ( 'NONE',  ( 7.375838497908012492, 217.2372850707501186, 87.54886208192142760 ) ) ;
#19994 = CARTESIAN_POINT ( 'NONE',  ( 61.52499999726881441, 169.8198683612136222, -4.815267126137197984 ) ) ;
#19995 = COLOUR_RGB ( '', 0.40784314, 0.44705882, 0.49803922) ;
#19997 = ORIENTED_EDGE ( 'NONE', *, *, #1615, .F. ) ;
#19996 = CARTESIAN_POINT ( 'NONE',  ( -6.220909254589537696, 198.5229672870051445, 24.05113791807856316 ) ) ;
#19998 = VECTOR ( 'NONE', #25441, 1000.000000000000114 ) ;
#19999 = CARTESIAN_POINT ( 'NONE',  ( 42.81132485994281467, 150.1262045565064511, 15.00000000000004086 ) ) ;
#20000 = CARTESIAN_POINT ( 'NONE',  ( 84.47499999726881015, 149.9369285172503510, 15.58253174999999580 ) ) ;
#20001 = CARTESIAN_POINT ( 'NONE',  ( 7.375838497908181246, 196.7627149292499666, 89.45113791807857240 ) ) ;
#20002 = DIRECTION ( 'NONE',  ( 0.000000000000000000, 0.000000000000000000, 1.000000000000000000 ) ) ;
#20003 = CIRCLE ( 'NONE', #31955, 5.250000000000004441 ) ;
#20004 = ORIENTED_EDGE ( 'NONE', *, *, #21426, .T. ) ;
#20005 = CARTESIAN_POINT ( 'NONE',  ( -7.375838497908014268, 196.7627149292498530, 71.04886208192142760 ) ) ;
#20006 = CARTESIAN_POINT ( 'NONE',  ( 6.139770520408223575, 215.5359834540460611, 72.54886208192142760 ) ) ;
#20007 = CARTESIAN_POINT ( 'NONE',  ( 3.662846001189864698, 218.4274158808046593, 18.39886208192143613 ) ) ;
#20008 = CARTESIAN_POINT ( 'NONE',  ( -27.50000000000000711, -5.348566131067991947, -17.76938258631346912 ) ) ;
#20009 = CARTESIAN_POINT ( 'NONE',  ( -9.984503880673473830, 210.2968891136704315, 33.65113791807856813 ) ) ;
#20010 = VERTEX_POINT ( 'NONE', #17377 ) ;
#20011 = CARTESIAN_POINT ( 'NONE',  ( 10.00000000000000711, 207.0476921513415220, 96.99886208192143044 ) ) ;
#20012 = ADVANCED_FACE ( 'NONE', ( #4425 ), #14813, .T. ) ;
#20013 = EDGE_LOOP ( 'NONE', ( #14648, #1620, #26070, #12012 ) ) ;
#20014 = FACE_OUTER_BOUND ( 'NONE', #5434, .T. ) ;
#20015 = CARTESIAN_POINT ( 'NONE',  ( 6.444103211790928043, 211.7408657792734061, 78.69886208192143329 ) ) ;
#20016 = AXIS2_PLACEMENT_3D ( 'NONE', #17461, #17634, #5026 ) ;
#20017 = ORIENTED_EDGE ( 'NONE', *, *, #3133, .F. ) ;
#20018 = EDGE_CURVE ( 'NONE', #27344, #8324, #25787, .T. ) ;
#20019 = VECTOR ( 'NONE', #6131, 1000.000000000000000 ) ;
#20020 = CARTESIAN_POINT ( 'NONE',  ( 3.500000000000004441, -1.692071238847163928, -2.682267049545481896 ) ) ;
#20021 = ORIENTED_EDGE ( 'NONE', *, *, #25595, .F. ) ;
#20022 = DIRECTION ( 'NONE',  ( -1.000000000000000000, -0.000000000000000000, -0.000000000000000000 ) ) ;
#20023 = CARTESIAN_POINT ( 'NONE',  ( 74.22499999726881015, 149.9369285172503510, 15.58253174999999580 ) ) ;
#20024 = DIRECTION ( 'NONE',  ( 0.000000000000000000, 0.000000000000000000, 1.000000000000000000 ) ) ;
#20025 = CARTESIAN_POINT ( 'NONE',  ( 2.517493886308900919, 214.5937144450984420, 82.40113791807856103 ) ) ;
#20026 = CARTESIAN_POINT ( 'NONE',  ( 87.50000000000002842, 169.3860439379083402, -5.988074444788474615 ) ) ;
#20027 = CIRCLE ( 'NONE', #981, 5.250000000000004441 ) ;
#20028 = FILL_AREA_STYLE_COLOUR ( '', #15362 ) ;
#20029 = CARTESIAN_POINT ( 'NONE',  ( 41.00000000000000711, 170.2462022514548323, -7.872454543227099337E-15 ) ) ;
#20030 = CARTESIAN_POINT ( 'NONE',  ( -0.05014649552828365914, 215.4116977939061144, 54.24886208192144466 ) ) ;
#20031 = CARTESIAN_POINT ( 'NONE',  ( 6.499999999999999112, 3.752776749732563477, -6.177805531628536961 ) ) ;
#20032 = DIRECTION ( 'NONE',  ( 1.000000000000000000, 0.000000000000000000, 0.000000000000000000 ) ) ;
#20033 = CARTESIAN_POINT ( 'NONE',  ( 95.59906517536109050, 155.0000000000000000, 31.00000000000000000 ) ) ;
#20034 = CARTESIAN_POINT ( 'NONE',  ( 48.62499999726880162, 138.6155565068815747, -3.929120461958505118E-15 ) ) ;
#20035 = CARTESIAN_POINT ( 'NONE',  ( 60.97499999726881015, 140.1801316387863778, -4.815267126137194431 ) ) ;
#20036 = CARTESIAN_POINT ( 'NONE',  ( -11.98450388067348804, 210.9467285061362247, 54.65113791807857524 ) ) ;
#20037 = CYLINDRICAL_SURFACE ( 'NONE', #32538, 15.00000000000001776 ) ;
#20038 = AXIS2_PLACEMENT_3D ( 'NONE', #1247, #19135, #8912 ) ;
#20039 = CARTESIAN_POINT ( 'NONE',  ( 10.01549611932653860, 210.2015048109876716, 100.8511379180785497 ) ) ;
#20040 = CARTESIAN_POINT ( 'NONE',  ( 10.01549611932653860, 210.2015048109876716, 79.85113791807856387 ) ) ;
#20041 = VECTOR ( 'NONE', #28406, 1000.000000000000000 ) ;
#20042 = CARTESIAN_POINT ( 'NONE',  ( -9.680171189290716072, 199.9079932115567146, 44.19886208192143329 ) ) ;
#20043 = CARTESIAN_POINT ( 'NONE',  ( 10.00000000000000711, 207.0476921513415220, 48.99886208192143044 ) ) ;
#20044 = DIRECTION ( 'NONE',  ( -1.000000000000000000, -0.000000000000000000, -0.000000000000000000 ) ) ;
#20045 = CARTESIAN_POINT ( 'NONE',  ( 3.753561863808689836, 218.3979405102790565, 82.40113791807856103 ) ) ;
#20046 = CARTESIAN_POINT ( 'NONE',  ( 74.78867513459483973, 155.0000000000000000, -15.00000000000002487 ) ) ;
#20047 = CARTESIAN_POINT ( 'NONE',  ( -10.01549611932653860, 203.7984951890123284, 3.351137918078566091 ) ) ;
#20048 = CARTESIAN_POINT ( 'NONE',  ( 8.118202686958138514, 201.1607312380088501, 70.29886208192142760 ) ) ;
#20049 = AXIS2_PLACEMENT_3D ( 'NONE', #14081, #23806, #13412 ) ;
#20050 = ORIENTED_EDGE ( 'NONE', *, *, #29682, .T. ) ;
#20051 = CARTESIAN_POINT ( 'NONE',  ( 7.456977232089471386, 196.8216656703012006, 73.44886208192143329 ) ) ;
#20052 = ORIENTED_EDGE ( 'NONE', *, *, #21018, .T. ) ;
#20053 = CARTESIAN_POINT ( 'NONE',  ( 79.27499999726880731, 149.9369285172503510, -15.58253175000000823 ) ) ;
#20054 = CARTESIAN_POINT ( 'NONE',  ( -6.444103211790928043, 202.2591342207265939, 56.19886208192144039 ) ) ;
#20055 = ORIENTED_EDGE ( 'NONE', *, *, #26661, .F. ) ;
#20056 = CARTESIAN_POINT ( 'NONE',  ( 82.97499999726881015, 140.1801316387863778, -4.815267126137194431 ) ) ;
#20057 = DIRECTION ( 'NONE',  ( 0.000000000000000000, 0.000000000000000000, -1.000000000000000000 ) ) ;
#20058 = CARTESIAN_POINT ( 'NONE',  ( -58.33685448808505214, 194.9217985566783113, -2.500000000000000444 ) ) ;
#20059 = AXIS2_PLACEMENT_3D ( 'NONE', #1602, #29892, #11993 ) ;
#20060 = CARTESIAN_POINT ( 'NONE',  ( 57.62499999726880873, 171.3844434931184253, -7.942151717890132712E-15 ) ) ;
#20061 = FILL_AREA_STYLE ('',( #9328 ) ) ;
#20062 = CARTESIAN_POINT ( 'NONE',  ( 3.044812012439969795, 216.5253028482143520, 45.39886208192143613 ) ) ;
#20063 = ORIENTED_EDGE ( 'NONE', *, *, #1371, .F. ) ;
#20064 = CARTESIAN_POINT ( 'NONE',  ( 6.500000000000000000, 3.752776749732563921, -8.000000000000000000 ) ) ;
#20065 = CONICAL_SURFACE ( 'NONE', #16796, 3.339999999999998970, 0.9599310885968821427 ) ;
#20066 = CARTESIAN_POINT ( 'NONE',  ( 8.000000000000008882, 206.9523078486586485, 11.00113791807856600 ) ) ;
#20067 =( NAMED_UNIT ( * ) SI_UNIT ( $, .STERADIAN. ) SOLID_ANGLE_UNIT ( ) );
#20068 = DIRECTION ( 'NONE',  ( -1.000000000000000000, -0.000000000000000000, -0.000000000000000000 ) ) ;
#20069 = CARTESIAN_POINT ( 'NONE',  ( 125.5000000000000000, 231.4735983853249763, -73.43303922622312996 ) ) ;
#20070 = CARTESIAN_POINT ( 'NONE',  ( 4.984841277089891776, 200.2242689037093726, 28.44886208192142973 ) ) ;
#20071 = CARTESIAN_POINT ( 'NONE',  ( -10.00000000000000711, 207.0476921513413515, 60.50113791807857666 ) ) ;
#20072 = CARTESIAN_POINT ( 'NONE',  ( 9.984503880673470277, 203.7031108863295401, 47.15113791807857524 ) ) ;
#20073 = APPLICATION_CONTEXT ( 'automotive_design' ) ;
#20074 = VECTOR ( 'NONE', #13135, 1000.000000000000000 ) ;
#20075 = CARTESIAN_POINT ( 'NONE',  ( 6.220909254589536808, 215.4770327129947702, 16.55113791807857027 ) ) ;
#20076 = CARTESIAN_POINT ( 'NONE',  ( -2.426778023690262742, 214.6231898156240163, 7.101137918078566535 ) ) ;
#20077 = CARTESIAN_POINT ( 'NONE',  ( 52.82499999726880446, 141.7447067706911810, -9.630534252274385310 ) ) ;
#20078 = FILL_AREA_STYLE ('',( #17009 ) ) ;
#20079 = CARTESIAN_POINT ( 'NONE',  ( 87.50000000000000000, 153.3135855332814401, -15.21687184359932132 ) ) ;
#20080 = CARTESIAN_POINT ( 'NONE',  ( 7.456977232089302632, 217.1783343296989131, 28.55113791807857027 ) ) ;
#20081 = DIRECTION ( 'NONE',  ( 0.000000000000000000, 0.000000000000000000, -1.000000000000000000 ) ) ;
#20082 = CARTESIAN_POINT ( 'NONE',  ( -6.139770520408369237, 215.5359834540460042, 72.95113791807854398 ) ) ;
#20083 = CARTESIAN_POINT ( 'NONE',  ( 8.062137200540920645, 201.0835637161417822, 53.30113791807857382 ) ) ;
#20084 = FACE_OUTER_BOUND ( 'NONE', #4813, .T. ) ;
#20085 = CARTESIAN_POINT ( 'NONE',  ( 54.38867513459481984, 140.7341522555726669, -4.635254915624220651 ) ) ;
#20086 = CARTESIAN_POINT ( 'NONE',  ( 9.736236675708031640, 199.9851607334238963, 10.29886208192143471 ) ) ;
#20087 = CARTESIAN_POINT ( 'NONE',  ( -0.05014649552828402690, 217.5146222423826714, 21.24886208192143400 ) ) ;
#20088 = CARTESIAN_POINT ( 'NONE',  ( 73.89999999453763735, 150.2886644046228639, -14.50000000000000888 ) ) ;
#20089 = VERTEX_POINT ( 'NONE', #30670 ) ;
#20090 = CARTESIAN_POINT ( 'NONE',  ( -7.456977232089304408, 196.8216656703010301, 54.05113791807856671 ) ) ;
#20091 = VECTOR ( 'NONE', #22515, 1000.000000000000227 ) ;
#20092 = CARTESIAN_POINT ( 'NONE',  ( 4.903702542908601636, 200.1653181626581102, 77.45113791807855819 ) ) ;
#20093 = CARTESIAN_POINT ( 'NONE',  ( 6.139770520408223575, 215.5359834540460611, 45.54886208192144181 ) ) ;
#20094 = CARTESIAN_POINT ( 'NONE',  ( 108.0159016311981759, 155.0000000000000000, -12.10452846326767684 ) ) ;
#20095 = ORIENTED_EDGE ( 'NONE', *, *, #1028, .T. ) ;
#20096 = ORIENTED_EDGE ( 'NONE', *, *, #4719, .F. ) ;
#20097 = VERTEX_POINT ( 'NONE', #28103 ) ;
#20098 = CARTESIAN_POINT ( 'NONE',  ( 57.98867513459482836, 146.1832212156128890, 12.13525491562421976 ) ) ;
#20099 = CARTESIAN_POINT ( 'NONE',  ( 1.127757440534757238, 7.231345287187090243, -6.344532336093706704 ) ) ;
#20100 = EDGE_LOOP ( 'NONE', ( #22823, #21681, #10716, #19136 ) ) ;
#20101 =( BOUNDED_CURVE ( )  B_SPLINE_CURVE ( 2, ( #2218, #12947, #12601, #20775, #28286, #15828, #31171, #7843, #28785, #28618, #5270 ),
 .UNSPECIFIED., .F., .F. ) 
 B_SPLINE_CURVE_WITH_KNOTS ( ( 3, 2, 2, 2, 2, 3 ),
 ( 0.8571428571428572063, 0.8607142857142858761, 0.8642857142857144348, 0.8678571428571429935, 0.8714285714285715523, 0.8750000000000001110 ),
 .UNSPECIFIED. ) 
 CURVE ( )  GEOMETRIC_REPRESENTATION_ITEM ( )  RATIONAL_B_SPLINE_CURVE ( ( 0.9999999999999984457, 0.9510565162951549745, 1.000000000000000000, 0.9510565162951534202, 1.000000000000000000, 0.9510565162951534202, 1.000000000000000000, 0.9510565162951534202, 1.000000000000000000, 0.9510565162951518658, 1.000000000000001554 ) ) 
 REPRESENTATION_ITEM ( '' )  );
#20102 = CARTESIAN_POINT ( 'NONE',  ( -2.426778023690262742, 214.6231898156240163, 31.10113791807856742 ) ) ;
#20103 = CYLINDRICAL_SURFACE ( 'NONE', #30307, 98.00000000000000000 ) ;
#20104 = EDGE_CURVE ( 'NONE', #16641, #4891, #26863, .T. ) ;
#20105 = CARTESIAN_POINT ( 'NONE',  ( 8.062137200540822946, 212.9164362838583315, 9.698862081921435063 ) ) ;
#20106 = CARTESIAN_POINT ( 'NONE',  ( 58.77499999726881441, 140.1801316387863778, 4.815267126137185549 ) ) ;
#20107 = EDGE_LOOP ( 'NONE', ( #18792, #2337, #5060, #1697 ) ) ;
#20108 = CARTESIAN_POINT ( 'NONE',  ( -0.05014649552807731031, 198.5883022060938572, 59.75113791807857666 ) ) ;
#20109 = LINE ( 'NONE', #32541, #5277 ) ;
#20110 = DIRECTION ( 'NONE',  ( -1.000000000000000000, 0.000000000000000000, 0.000000000000000000 ) ) ;
#20111 = VECTOR ( 'NONE', #8515, 1000.000000000000000 ) ;
#20112 = CARTESIAN_POINT ( 'NONE',  ( -6.139770520408224463, 198.4640165459539389, 101.0488620819214134 ) ) ;
#20113 = CARTESIAN_POINT ( 'NONE',  ( 64.67499999726878457, 141.7447067706911810, 9.630534252274376428 ) ) ;
#20114 = CARTESIAN_POINT ( 'NONE',  ( 3.135527875058820690, 216.4958274776887492, 34.40113791807856813 ) ) ;
#20115 = DIRECTION ( 'NONE',  ( -1.000000000000000000, 0.000000000000000000, 0.000000000000000000 ) ) ;
#20116 = CARTESIAN_POINT ( 'NONE',  ( -3.044812012440131443, 216.5253028482142952, 22.10113791807856742 ) ) ;
#20117 = CARTESIAN_POINT ( 'NONE',  ( 132.3999999999999773, 80.04668119422552763, -74.95331880577366235 ) ) ;
#20118 = CARTESIAN_POINT ( 'NONE',  ( 81.69999999999998863, 146.4771138417591203, 11.73074641843673227 ) ) ;
#20119 = CARTESIAN_POINT ( 'NONE',  ( -5.357619327558936585E-16, 7.505553499465137612, -6.064240316920400886 ) ) ;
#20120 = CARTESIAN_POINT ( 'NONE',  ( 10.01549611932653860, 210.2015048109876716, 100.8511379180785497 ) ) ;
#20121 = DIRECTION ( 'NONE',  ( -1.000000000000000000, -0.000000000000000000, -0.000000000000000000 ) ) ;
#20122 = CARTESIAN_POINT ( 'NONE',  ( 52.07499999726881157, 168.2552932293087906, 9.630534252274372875 ) ) ;
#20123 = CARTESIAN_POINT ( 'NONE',  ( -10.00000000000000711, 207.0476921513413515, 51.50113791807857666 ) ) ;
#20124 = CARTESIAN_POINT ( 'NONE',  ( 83.52499999726880731, 169.8198683612136222, -4.815267126137197984 ) ) ;
#20125 = CARTESIAN_POINT ( 'NONE',  ( 42.41132485994280898, 167.7597621252805880, 9.270509831248428867 ) ) ;
#20126 = CARTESIAN_POINT ( 'NONE',  ( -7.500000000000000000, -4.330127018922198090, -7.422398894150034288 ) ) ;
#20127 = CARTESIAN_POINT ( 'NONE',  ( 53.99999999453762456, 155.0000000000000000, -14.50000000000000711 ) ) ;
#20128 = VERTEX_POINT ( 'NONE', #32701 ) ;
#20129 = CARTESIAN_POINT ( 'NONE',  ( 7.375838497908181246, 196.7627149292499666, 32.45113791807856529 ) ) ;
#20130 = DIRECTION ( 'NONE',  ( 0.000000000000000000, 0.000000000000000000, -1.000000000000000000 ) ) ;
#20131 = CARTESIAN_POINT ( 'NONE',  ( -3.044812012439970683, 197.4746971517856196, 7.898862081921434353 ) ) ;
#20132 = CARTESIAN_POINT ( 'NONE',  ( 32.50000000000000000, 155.0000000000000000, -15.00000000000002487 ) ) ;
#20133 = VERTEX_POINT ( 'NONE', #2885 ) ;
#20134 = CARTESIAN_POINT ( 'NONE',  ( 9.984503880673470277, 203.7031108863295401, 2.151137918078565914 ) ) ;
#20135 = CARTESIAN_POINT ( 'NONE',  ( 8.062137200540920645, 201.0835637161417822, 59.30113791807857382 ) ) ;
#20136 = ADVANCED_FACE ( 'NONE', ( #23339 ), #5439, .T. ) ;
#20137 = VERTEX_POINT ( 'NONE', #7504 ) ;
#20138 = CARTESIAN_POINT ( 'NONE',  ( 0.05014649552828262524, 198.5883022060938572, 25.74886208192143755 ) ) ;
#20139 = DIRECTION ( 'NONE',  ( 0.000000000000000000, -1.224646799147353454E-16, 1.000000000000000000 ) ) ;
#20140 = VERTEX_POINT ( 'NONE', #22994 ) ;
#20141 = CARTESIAN_POINT ( 'NONE',  ( -2.517493886308901807, 199.4062855549015012, -0.09886208192143407236 ) ) ;
#20142 = EDGE_CURVE ( 'NONE', #10102, #15361, #31978, .T. ) ;
#20143 = DIRECTION ( 'NONE',  ( -0.000000000000000000, 0.000000000000000000, 1.000000000000000000 ) ) ;
#20144 = CARTESIAN_POINT ( 'NONE',  ( -9.736236675708031640, 214.0148392665760753, 89.79886208192142760 ) ) ;
#20145 = CARTESIAN_POINT ( 'NONE',  ( 34.87499999726881583, 138.6155565068815747, -3.929120461958505118E-15 ) ) ;
#20146 = ORIENTED_EDGE ( 'NONE', *, *, #28931, .F. ) ;
#20147 = CARTESIAN_POINT ( 'NONE',  ( 41.42499999726881299, 168.2552932293087906, -9.630534252274385310 ) ) ;
#20148 = CARTESIAN_POINT ( 'NONE',  ( 53.91132485994280898, 163.8167787843871110, -12.13525491562423397 ) ) ;
#20149 = CARTESIAN_POINT ( 'NONE',  ( -10.00000000000000711, 206.9523078486584495, 71.49886208192144466 ) ) ;
#20150 = CARTESIAN_POINT ( 'NONE',  ( 45.37499999726880873, 155.0000000000000000, -15.58253175000000823 ) ) ;
#20151 = FACE_BOUND ( 'NONE', #3793, .T. ) ;
#20152 = CARTESIAN_POINT ( 'NONE',  ( -6.139770520408369237, 215.5359834540460042, 0.9511379180785658471 ) ) ;
#20153 = CARTESIAN_POINT ( 'NONE',  ( 53.71132485994279904, 155.0000000000000000, -15.00000000000002487 ) ) ;
#20154 = EDGE_CURVE ( 'NONE', #16522, #1291, #4456, .T. ) ;
#20155 = CARTESIAN_POINT ( 'NONE',  ( 58.99999999999999289, 170.2462022514548323, -7.872454543227099337E-15 ) ) ;
#20156 = CARTESIAN_POINT ( 'NONE',  ( -10.00000000000000711, 207.0476921513413515, 87.50113791807858377 ) ) ;
#20157 = DIRECTION ( 'NONE',  ( 0.000000000000000000, 0.000000000000000000, 1.000000000000000000 ) ) ;
#20158 = ADVANCED_BREP_SHAPE_REPRESENTATION ( '', ( #12555, #2404 ), #19701 ) ;
#20159 = CARTESIAN_POINT ( 'NONE',  ( -8.118202686958039038, 201.1607312380087080, 78.20113791807857240 ) ) ;
#20160 = CARTESIAN_POINT ( 'NONE',  ( 92.60208470531341618, 155.0000000000000000, 12.99999999999999822 ) ) ;
#20161 = DIRECTION ( 'NONE',  ( 0.000000000000000000, 0.000000000000000000, -1.000000000000000000 ) ) ;
#20162 = CARTESIAN_POINT ( 'NONE',  ( 12.01549611932659367, 203.1486557965466773, 91.14886208192143613 ) ) ;
#20163 = CARTESIAN_POINT ( 'NONE',  ( 61.02499999726880020, 149.9369285172503510, -15.58253175000000823 ) ) ;
#20165 = ORIENTED_EDGE ( 'NONE', *, *, #33290, .T. ) ;
#20164 = CARTESIAN_POINT ( 'NONE',  ( -3.135527875058821579, 197.5041725223112223, 32.90113791807857524 ) ) ;
#20166 = CARTESIAN_POINT ( 'NONE',  ( -10.83124253962819949, 25.50084400951695329, -0.1142222407377227189 ) ) ;
#20167 = CARTESIAN_POINT ( 'NONE',  ( 87.97499999726882436, 169.8198683612136222, 4.815267126137181997 ) ) ;
#20168 = CARTESIAN_POINT ( 'NONE',  ( -3.662846001190052991, 218.4274158808045740, 91.10113791807859229 ) ) ;
#20169 = EDGE_CURVE ( 'NONE', #2726, #12310, #21441, .T. ) ;
#20170 = DIRECTION ( 'NONE',  ( 0.000000000000000000, 0.000000000000000000, -1.000000000000000000 ) ) ;
#20171 = EDGE_LOOP ( 'NONE', ( #10563, #31079, #13063, #26628 ) ) ;
#20172 = CARTESIAN_POINT ( 'NONE',  ( -3.044812012439970683, 197.4746971517856196, 82.89886208192145034 ) ) ;
#20173 = CIRCLE ( 'NONE', #17992, 3.999999999999999112 ) ;
#20174 = CARTESIAN_POINT ( 'NONE',  ( 11.98450388067341876, 210.9467285061363953, 9.848862081921433642 ) ) ;
#20175 = CARTESIAN_POINT ( 'NONE',  ( -6.831985876597697072, 3.295913427296342402, -6.443925148804115821 ) ) ;
#20176 = CARTESIAN_POINT ( 'NONE',  ( 6.139770520408368348, 198.4640165459539674, 32.45113791807856529 ) ) ;
#20177 = EDGE_CURVE ( 'NONE', #3832, #21298, #15660, .T. ) ;
#20178 = CARTESIAN_POINT ( 'NONE',  ( -2.459698528280933161, 7.240146430416066536, -0.09933465333851029810 ) ) ;
#20179 = CARTESIAN_POINT ( 'NONE',  ( -3.044812012439970683, 197.4746971517856196, 97.89886208192145034 ) ) ;
#20180 = CARTESIAN_POINT ( 'NONE',  ( 6.878751942472531411, 3.924677726130922473, -6.573129608219089981 ) ) ;
#20181 = ORIENTED_EDGE ( 'NONE', *, *, #18354, .F. ) ;
#20182 = CARTESIAN_POINT ( 'NONE',  ( -11.40740920524442004, -25.16819403002536859, -17.99999999999998579 ) ) ;
#20183 = CARTESIAN_POINT ( 'NONE',  ( 0.05014649552828262524, 198.5883022060938572, 82.74886208192144466 ) ) ;
#20184 = EDGE_LOOP ( 'NONE', ( #2733, #12165, #30964, #14983 ) ) ;
#20185 = DIRECTION ( 'NONE',  ( -1.000000000000000000, -4.625929269271485914E-16, 0.000000000000000000 ) ) ;
#20186 = VERTEX_POINT ( 'NONE', #2387 ) ;
#20187 = CARTESIAN_POINT ( 'NONE',  ( 6.484173630542770184, 4.916614646782027087, -7.642786413619098163 ) ) ;
#20188 = CARTESIAN_POINT ( 'NONE',  ( 72.77499999726882152, 140.1801316387863778, 4.815267126137185549 ) ) ;
#20189 = CARTESIAN_POINT ( 'NONE',  ( 80.52499999726880731, 140.1801316387863778, 4.815267126137185549 ) ) ;
#20190 = DIRECTION ( 'NONE',  ( 1.000000000000000000, 0.000000000000000000, 0.000000000000000000 ) ) ;
#20191 = CARTESIAN_POINT ( 'NONE',  ( -8.000000000000008882, 207.0476921513413515, 78.50113791807856956 ) ) ;
#20192 = CARTESIAN_POINT ( 'NONE',  ( 4.000000000000000000, -1.759474945355388176, -3.047499999999998099 ) ) ;
#20193 =( NAMED_UNIT ( * ) SI_UNIT ( $, .STERADIAN. ) SOLID_ANGLE_UNIT ( ) );
#20194 = CARTESIAN_POINT ( 'NONE',  ( 39.00000000000000000, 170.2462022514548323, -7.872454543227099337E-15 ) ) ;
#20195 = CARTESIAN_POINT ( 'NONE',  ( -4.903702542908436435, 200.1653181626580249, 56.04886208192144181 ) ) ;
#20196 = EDGE_CURVE ( 'NONE', #16646, #10890, #7838, .T. ) ;
#20197 = EDGE_CURVE ( 'NONE', #31548, #10267, #21418, .T. ) ;
#20198 = DIRECTION ( 'NONE',  ( 1.000000000000000000, 0.000000000000000000, 0.000000000000000000 ) ) ;
#20199 = CARTESIAN_POINT ( 'NONE',  ( 78.18867513459481700, 140.7341522555726669, 4.635254915624211769 ) ) ;
#20200 = CARTESIAN_POINT ( 'NONE',  ( -125.6872233929727827, 5.250000000000003553, 35.00001199999999812 ) ) ;
#20201 = CARTESIAN_POINT ( 'NONE',  ( 60.42499999726881299, 141.7447067706911810, 9.630534252274376428 ) ) ;
#20202 = CARTESIAN_POINT ( 'NONE',  ( 66.17499999726881299, 164.1591823560292198, 12.60653300113718167 ) ) ;
#20203 = CARTESIAN_POINT ( 'NONE',  ( -9.680171189290831535, 214.0920067884431148, 60.80113791807858092 ) ) ;
#20204 = DIRECTION ( 'NONE',  ( 0.7071067811865461294, 0.000000000000000000, -0.7071067811865489050 ) ) ;
#20205 = CARTESIAN_POINT ( 'NONE',  ( 12.00000000000000711, 206.9523078486586485, 2.001137918078565114 ) ) ;
#20206 = EDGE_CURVE ( 'NONE', #23990, #12774, #11096, .T. ) ;
#20207 = CARTESIAN_POINT ( 'NONE',  ( -8.062137200540920645, 212.9164362838581894, 75.80113791807858092 ) ) ;
#20208 = CARTESIAN_POINT ( 'NONE',  ( 12.01549611932659367, 203.1486557965466773, 46.14886208192143613 ) ) ;
#20209 = CARTESIAN_POINT ( 'NONE',  ( 6.139770520408223575, 215.5359834540460611, 51.54886208192142760 ) ) ;
#20210 = DIRECTION ( 'NONE',  ( 1.000000000000000000, 0.000000000000000000, 0.000000000000000000 ) ) ;
#20211 = CARTESIAN_POINT ( 'NONE',  ( 12.01549611932652972, 210.8513442034534933, 82.85113791807857808 ) ) ;
#20212 = FACE_OUTER_BOUND ( 'NONE', #18717, .T. ) ;
#20213 = CARTESIAN_POINT ( 'NONE',  ( 10.01549611932653860, 210.2015048109876716, 7.851137918078566535 ) ) ;
#20214 = EDGE_CURVE ( 'NONE', #2588, #5010, #12940, .T. ) ;
#20215 = CARTESIAN_POINT ( 'NONE',  ( 6.220909254589681581, 198.5229672870052582, 67.44886208192143329 ) ) ;
#20216 = DIRECTION ( 'NONE',  ( -1.000000000000000000, -0.000000000000000000, -0.000000000000000000 ) ) ;
#20217 = ORIENTED_EDGE ( 'NONE', *, *, #30373, .T. ) ;
#20218 = CARTESIAN_POINT ( 'NONE',  ( 7.375838497908012492, 217.2372850707501186, 75.54886208192142760 ) ) ;
#20219 = VECTOR ( 'NONE', #1216, 1000.000000000000000 ) ;
#20220 = EDGE_LOOP ( 'NONE', ( #26878, #28937, #32318, #8326 ) ) ;
#20221 = CARTESIAN_POINT ( 'NONE',  ( 79.57499999726881867, 164.1591823560292198, -12.60653300113719766 ) ) ;
#20222 = CARTESIAN_POINT ( 'NONE',  ( 2.426778023690075337, 214.6231898156240447, 51.39886208192145745 ) ) ;
#20223 = VERTEX_POINT ( 'NONE', #7671 ) ;
#20224 = CARTESIAN_POINT ( 'NONE',  ( 73.72499999726881015, 169.8198683612136222, 4.815267126137181997 ) ) ;
#20225 = DIRECTION ( 'NONE',  ( 0.000000000000000000, 0.000000000000000000, -1.000000000000000000 ) ) ;
#20226 = CARTESIAN_POINT ( 'NONE',  ( -2.262848203703084593, -6.566616684922157887, -6.208169345099794789 ) ) ;
#20227 = AXIS2_PLACEMENT_3D ( 'NONE', #6865, #1250, #16913 ) ;
#20228 = CARTESIAN_POINT ( 'NONE',  ( 64.82499999726881867, 141.7447067706911810, -9.630534252274385310 ) ) ;
#20229 = FILL_AREA_STYLE ('',( #26024 ) ) ;
#20230 = CARTESIAN_POINT ( 'NONE',  ( -10.00000000000000711, 206.9523078486584495, 38.49886208192143755 ) ) ;
#20231 = ORIENTED_EDGE ( 'NONE', *, *, #11384, .F. ) ;
#20232 = FACE_OUTER_BOUND ( 'NONE', #22068, .T. ) ;
#20233 = SHAPE_REPRESENTATION_RELATIONSHIP ( 'NONE' , 'NONE' ,  #12832, #2741 ) ;
#20234 = DIRECTION ( 'NONE',  ( 0.000000000000000000, 0.000000000000000000, -1.000000000000000000 ) ) ;
#20235 = DIRECTION ( 'NONE',  ( 0.000000000000000000, 0.000000000000000000, -1.000000000000000000 ) ) ;
#20236 = CARTESIAN_POINT ( 'NONE',  ( -2.426778023690076225, 199.3768101843759553, 28.89886208192143613 ) ) ;
#20237 = CARTESIAN_POINT ( 'NONE',  ( -6.139770520408369237, 215.5359834540460042, 72.95113791807854398 ) ) ;
#20238 = DIRECTION ( 'NONE',  ( 1.000000000000000000, 0.000000000000000000, 0.000000000000000000 ) ) ;
#20239 = CARTESIAN_POINT ( 'NONE',  ( 9.984503880673470277, 203.7031108863295401, 50.15113791807855392 ) ) ;
#20240 = CARTESIAN_POINT ( 'NONE',  ( 3.044812012440130555, 197.4746971517856764, 14.60113791807856565 ) ) ;
#20241 = CARTESIAN_POINT ( 'NONE',  ( 6.500168698208129925, 211.6636982574063381, 4.701137918078565292 ) ) ;
#20242 = CARTESIAN_POINT ( 'NONE',  ( 109.0104235265664272, 155.0000000000000000, 0.000000000000000000 ) ) ;
#20243 = CARTESIAN_POINT ( 'NONE',  ( 36.02499999726881441, 160.0630714827496206, 15.58253174999999224 ) ) ;
#20244 = CARTESIAN_POINT ( 'NONE',  ( 9.736236675707914401, 214.0148392665762458, 31.70113791807856529 ) ) ;
#20245 = CARTESIAN_POINT ( 'NONE',  ( 115.4999999999999858, 258.9084171661918958, -28.95509836041981089 ) ) ;
#20246 =( BOUNDED_CURVE ( )  B_SPLINE_CURVE ( 2, ( #3758, #11258, #13974, #8698, #26583, #10931, #13808, #11099, #21642, #24030, #21805 ),
 .UNSPECIFIED., .F., .T. ) 
 B_SPLINE_CURVE_WITH_KNOTS ( ( 3, 2, 2, 2, 2, 3 ),
 ( 0.2857142857142856984, 0.2892857142857143127, 0.2928571428571428714, 0.2964285714285714302, 0.2999999999999999889, 0.3035714285714285476 ),
 .UNSPECIFIED. ) 
 CURVE ( )  GEOMETRIC_REPRESENTATION_ITEM ( )  RATIONAL_B_SPLINE_CURVE ( ( 1.000000000000000000, 0.9510565162951534202, 1.000000000000000000, 0.9510565162951534202, 1.000000000000000000, 0.9510565162951534202, 1.000000000000000000, 0.9510565162951534202, 1.000000000000000000, 0.9510565162951534202, 1.000000000000000000 ) ) 
 REPRESENTATION_ITEM ( '' )  );
#20247 = CARTESIAN_POINT ( 'NONE',  ( 8.118202686958039038, 212.8392687619912635, 76.70113791807857240 ) ) ;
#20248 = CARTESIAN_POINT ( 'NONE',  ( -3.135527875058821579, 197.5041725223112223, 53.90113791807857524 ) ) ;
#20249 = DIRECTION ( 'NONE',  ( -0.000000000000000000, -0.000000000000000000, 1.000000000000000000 ) ) ;
#20250 = CARTESIAN_POINT ( 'NONE',  ( 53.88867513459484115, 150.1262045565061385, 14.99999999999982947 ) ) ;
#20251 = CARTESIAN_POINT ( 'NONE',  ( 3.753561863808876797, 195.6020594897209719, 16.59886208192143187 ) ) ;
#20252 = CARTESIAN_POINT ( 'NONE',  ( 9.984503880673420539, 210.2968891136705736, 21.84886208192143542 ) ) ;
#20253 = CARTESIAN_POINT ( 'NONE',  ( 71.39999999453763735, 141.2096805137202580, 4.480746418436733158 ) ) ;
#20254 = AXIS2_PLACEMENT_3D ( 'NONE', #961, #8793, #24470 ) ;
#20255 = ORIENTED_EDGE ( 'NONE', *, *, #16795, .F. ) ;
#20256 = CARTESIAN_POINT ( 'NONE',  ( -9.680171189290831535, 214.0920067884431148, 54.80113791807857382 ) ) ;
#20257 = CARTESIAN_POINT ( 'NONE',  ( -8.015496119326531499, 204.4483345814780364, 75.35113791807856387 ) ) ;
#20258 = VECTOR ( 'NONE', #531, 1000.000000000000227 ) ;
#20259 = CARTESIAN_POINT ( 'NONE',  ( 6.220909254589681581, 198.5229672870052582, 43.44886208192143329 ) ) ;
#20260 = DIRECTION ( 'NONE',  ( -1.000000000000000000, 0.000000000000000000, -0.000000000000000000 ) ) ;
#20261 = EDGE_LOOP ( 'NONE', ( #21059, #19750 ) ) ;
#20262 = ORIENTED_EDGE ( 'NONE', *, *, #29945, .F. ) ;
#20263 = ORIENTED_EDGE ( 'NONE', *, *, #19488, .T. ) ;
#20264 = DIRECTION ( 'NONE',  ( 1.000000000000000000, -0.000000000000000000, -0.000000000000000000 ) ) ;
#20265 = AXIS2_PLACEMENT_3D ( 'NONE', #22330, #19944, #27951 ) ;
#20266 = DIRECTION ( 'NONE',  ( 0.000000000000000000, 0.5000000000000009992, 0.8660254037844380415 ) ) ;
#20267 = ORIENTED_EDGE ( 'NONE', *, *, #17013, .T. ) ;
#20268 = CARTESIAN_POINT ( 'NONE',  ( -6.444103211791042618, 211.7408657792732356, 33.80113791807857382 ) ) ;
#20269 = CARTESIAN_POINT ( 'NONE',  ( 55.21132485994282746, 139.2280666364260071, -4.041636747397287284E-15 ) ) ;
#20270 = CARTESIAN_POINT ( 'NONE',  ( -0.05014649552828403384, 217.5146222423826714, 9.248862081921432221 ) ) ;
#20271 = CARTESIAN_POINT ( 'NONE',  ( 59.27499999726882152, 149.9369285172503510, -15.58253175000000823 ) ) ;
#20272 = ORIENTED_EDGE ( 'NONE', *, *, #22842, .F. ) ;
#20273 = CARTESIAN_POINT ( 'NONE',  ( 0.05014649552807626948, 215.4116977939061144, 64.25113791807856956 ) ) ;
#20274 = CARTESIAN_POINT ( 'NONE',  ( 6.500000000000000000, -3.752776749732574135, -6.064240316920400886 ) ) ;
#20275 = AXIS2_PLACEMENT_3D ( 'NONE', #22249, #32970, #14242 ) ;
#20276 = CARTESIAN_POINT ( 'NONE',  ( 125.5000000000000000, 155.0000000000000000, -112.0000000000000711 ) ) ;
#20277 = CARTESIAN_POINT ( 'NONE',  ( -10.10169002831358576, 228.2744804605295315, 105.4832055762869061 ) ) ;
#20278 = CIRCLE ( 'NONE', #28988, 2.149999999999974598 ) ;
#20279 = CARTESIAN_POINT ( 'NONE',  ( 63.97499999726881725, 169.8198683612136222, 4.815267126137181997 ) ) ;
#20280 = CARTESIAN_POINT ( 'NONE',  ( -10.01549611932653860, 203.7984951890123284, 45.35113791807857808 ) ) ;
#20281 = CARTESIAN_POINT ( 'NONE',  ( -6.815830331203685866, -1.210827632163352847E-13, -6.171384342982610960 ) ) ;
#20282 = CARTESIAN_POINT ( 'NONE',  ( 10.01549611932653860, 210.2015048109876716, 19.85113791807856387 ) ) ;
#20283 = CARTESIAN_POINT ( 'NONE',  ( 3.135527875058981895, 197.5041725223112792, 103.5988620819214390 ) ) ;
#20284 = DIRECTION ( 'NONE',  ( 1.000000000000000000, 0.000000000000000000, 6.123233995736766036E-17 ) ) ;
#20285 = CARTESIAN_POINT ( 'NONE',  ( 33.12499999726880873, 155.0000000000000000, -15.58253175000000823 ) ) ;
#20286 = DIRECTION ( 'NONE',  ( 0.000000000000000000, 0.000000000000000000, -1.000000000000000000 ) ) ;
#20287 = DIRECTION ( 'NONE',  ( -2.312964634635740985E-16, 1.000000000000000000, 0.000000000000000000 ) ) ;
#20288 = CARTESIAN_POINT ( 'NONE',  ( 3.753561863808689836, 218.3979405102790565, 4.401137918078566358 ) ) ;
#20289 = DIRECTION ( 'NONE',  ( -1.000000000000000000, -0.000000000000000000, -0.000000000000000000 ) ) ;
#20290 = CARTESIAN_POINT ( 'NONE',  ( 49.97499999726881725, 169.8198683612136222, 4.815267126137181997 ) ) ;
#20291 = CARTESIAN_POINT ( 'NONE',  ( 3.135527875058820690, 216.4958274776887492, 49.40113791807857524 ) ) ;
#20292 = CARTESIAN_POINT ( 'NONE',  ( 87.02499999726879309, 149.9369285172503510, -15.58253175000000823 ) ) ;
#20293 = CONICAL_SURFACE ( 'NONE', #32248, 32.00000000000000000, 0.1047197551197278087 ) ;
#20294 = DIRECTION ( 'NONE',  ( 0.000000000000000000, 0.000000000000000000, 1.000000000000000000 ) ) ;
#20295 = CARTESIAN_POINT ( 'NONE',  ( 107.5000000000000000, 155.0000000000000000, -6.938893903907228378E-15 ) ) ;
#20296 = CARTESIAN_POINT ( 'NONE',  ( 56.29999999453762172, 167.3344367211045096, -8.961492836873482304 ) ) ;
#20297 = VERTEX_POINT ( 'NONE', #15497 ) ;
#20298 = CARTESIAN_POINT ( 'NONE',  ( -11.98450388067348804, 210.9467285061362247, 30.65113791807856458 ) ) ;
#20299 = LINE ( 'NONE', #25409, #12725 ) ;
#20300 = EDGE_CURVE ( 'NONE', #23132, #18459, #8916, .T. ) ;
#20301 = CARTESIAN_POINT ( 'NONE',  ( 0.05014649552828275708, 196.4853777576173002, 7.748862081921435774 ) ) ;
#20302 = CARTESIAN_POINT ( 'NONE',  ( 60.41132485994281609, 167.7597621252805880, 9.270509831248428867 ) ) ;
#20303 = ORIENTED_EDGE ( 'NONE', *, *, #27480, .F. ) ;
#20304 =( BOUNDED_CURVE ( )  B_SPLINE_CURVE ( 2, ( #24353, #16680, #10839, #25360, #2671, #2032, #1858, #13212, #17527, #8118, #5540 ),
 .UNSPECIFIED., .F., .F. ) 
 B_SPLINE_CURVE_WITH_KNOTS ( ( 3, 2, 2, 2, 2, 3 ),
 ( 0.03571428571428574700, 0.03928571428571427104, 0.04285714285714279509, 0.04642857142857131914, 0.04999999999999984318, 0.05357142857142836723 ),
 .UNSPECIFIED. ) 
 CURVE ( )  GEOMETRIC_REPRESENTATION_ITEM ( )  RATIONAL_B_SPLINE_CURVE ( ( 0.9999999999999993339, 0.9510565162951540863, 1.000000000000000000, 0.9510565162951534202, 1.000000000000000000, 0.9510565162951534202, 1.000000000000000000, 0.9510565162951534202, 1.000000000000000000, 0.9510565162951550855, 0.9999999999999983347 ) ) 
 REPRESENTATION_ITEM ( '' )  );
#20305 = CARTESIAN_POINT ( 'NONE',  ( 3.044812012440130555, 197.4746971517856764, 8.601137918078565647 ) ) ;
#20306 = CARTESIAN_POINT ( 'NONE',  ( -10.00000000000000711, 207.0476921513413515, 60.50113791807857666 ) ) ;
#20307 = CIRCLE ( 'NONE', #27911, 70.00000000000000000 ) ;
#20308 = ORIENTED_EDGE ( 'NONE', *, *, #28899, .F. ) ;
#20309 = CARTESIAN_POINT ( 'NONE',  ( 8.015496119326595448, 204.4483345814782638, 22.14886208192143613 ) ) ;
#20310 = AXIS2_PLACEMENT_3D ( 'NONE', #9760, #32920, #20143 ) ;
#20311 = CARTESIAN_POINT ( 'NONE',  ( 117.5000000000000142, 155.0000000000000000, -6.938893903907228378E-15 ) ) ;
#20312 = VERTEX_POINT ( 'NONE', #8173 ) ;
#20313 = CARTESIAN_POINT ( 'NONE',  ( -2.426778023690262742, 214.6231898156240163, 7.101137918078566535 ) ) ;
#20314 = CARTESIAN_POINT ( 'NONE',  ( 9.736236675708031640, 199.9851607334238963, 85.29886208192145602 ) ) ;
#20315 = CARTESIAN_POINT ( 'NONE',  ( 36.17499999726880588, 164.1591823560292198, 12.60653300113718167 ) ) ;
#20316 = ORIENTED_EDGE ( 'NONE', *, *, #21435, .T. ) ;
#20317 = CARTESIAN_POINT ( 'NONE',  ( 42.32499999726881157, 145.8408176439707802, 12.60653300113718345 ) ) ;
#20318 = CARTESIAN_POINT ( 'NONE',  ( 7.499999999999999112, 1.854554393013827296, -0.1880126015361732184 ) ) ;
#20319 = CARTESIAN_POINT ( 'NONE',  ( 8.118202686958039038, 212.8392687619912635, 1.701137918078565736 ) ) ;
#20320 = CONICAL_SURFACE ( 'NONE', #1799, 3.499999999999999556, 1.047197551196589638 ) ;
#20321 =( GEOMETRIC_REPRESENTATION_CONTEXT ( 3 ) GLOBAL_UNCERTAINTY_ASSIGNED_CONTEXT ( ( #11797 ) ) GLOBAL_UNIT_ASSIGNED_CONTEXT ( ( #22406, #6408, #4019 ) ) REPRESENTATION_CONTEXT ( 'NONE', 'WORKASPACE' ) );
#20322 = CARTESIAN_POINT ( 'NONE',  ( 8.118202686958138514, 201.1607312380088501, 70.29886208192142760 ) ) ;
#20323 = CARTESIAN_POINT ( 'NONE',  ( 49.37499999726880873, 155.0000000000000000, -15.58253175000000823 ) ) ;
#20324 = CARTESIAN_POINT ( 'NONE',  ( 13.75000000000000888, -23.81569860407206463, 0.000000000000000000 ) ) ;
#20325 = CARTESIAN_POINT ( 'NONE',  ( 3.044812012440130555, 197.4746971517856764, 2.601137918078566091 ) ) ;
#20326 = CARTESIAN_POINT ( 'NONE',  ( 58.01132485994281751, 167.7597621252805880, -9.270509831248443078 ) ) ;
#20327 =( REPRESENTATION_RELATIONSHIP ('NONE','NONE', #25663, #30243 ) REPRESENTATION_RELATIONSHIP_WITH_TRANSFORMATION ( #2359 )SHAPE_REPRESENTATION_RELATIONSHIP( ) );
#20328 = MECHANICAL_DESIGN_GEOMETRIC_PRESENTATION_REPRESENTATION (  '', ( #26308 ), #33393 ) ;
#20329 = CARTESIAN_POINT ( 'NONE',  ( 68.70000000000001705, 163.5228861582408797, -11.73074641843674470 ) ) ;
#20330 = CARTESIAN_POINT ( 'NONE',  ( -6.139770520408369237, 215.5359834540460042, 87.95113791807858661 ) ) ;
#20331 = DIRECTION ( 'NONE',  ( 0.000000000000000000, 0.7071067811865475727, 0.7071067811865475727 ) ) ;
#20332 = CARTESIAN_POINT ( 'NONE',  ( -6.220909254589537696, 198.5229672870051161, 72.05113791807853829 ) ) ;
#20333 = CARTESIAN_POINT ( 'NONE',  ( -67.50000000000000000, 0.000000000000000000, 17.00000000000001421 ) ) ;
#20334 = AXIS2_PLACEMENT_3D ( 'NONE', #13026, #10481, #31421 ) ;
#20335 = CARTESIAN_POINT ( 'NONE',  ( 34.87499999726880873, 138.6155565068815463, -3.929120461958505118E-15 ) ) ;
#20336 = CARTESIAN_POINT ( 'NONE',  ( -12.01549611932659722, 210.8513442034533227, 83.64886208192143613 ) ) ;
#20337 = VECTOR ( 'NONE', #3576, 1000.000000000000114 ) ;
#20338 = CARTESIAN_POINT ( 'NONE',  ( 65.82499999726881867, 168.2552932293087906, 9.630534252274372875 ) ) ;
#20340 = ORIENTED_EDGE ( 'NONE', *, *, #21993, .F. ) ;
#20339 = CARTESIAN_POINT ( 'NONE',  ( 10.00000000000000711, 206.9523078486586201, 26.00113791807856956 ) ) ;
#20341 = CARTESIAN_POINT ( 'NONE',  ( -60.38337337305365793, 194.9660334721754111, 1.652118058477962004 ) ) ;
#20342 = CARTESIAN_POINT ( 'NONE',  ( 36.29999999453763593, 167.3344367211045096, -8.961492836873482304 ) ) ;
#20343 = CARTESIAN_POINT ( 'NONE',  ( -9.680171189290831535, 214.0920067884431148, 96.80113791807858092 ) ) ;
#20344 = FACE_OUTER_BOUND ( 'NONE', #27376, .T. ) ;
#20345 = EDGE_CURVE ( 'NONE', #6342, #4633, #15446, .T. ) ;
#20346 = ORIENTED_EDGE ( 'NONE', *, *, #7239, .T. ) ;
#20347 = MECHANICAL_DESIGN_GEOMETRIC_PRESENTATION_REPRESENTATION (  '', ( #30690 ), #6745 ) ;
#20348 = CARTESIAN_POINT ( 'NONE',  ( -10.00000000000000711, 206.9523078486584495, 83.49886208192143044 ) ) ;
#20349 = CARTESIAN_POINT ( 'NONE',  ( -12.01549611932659722, 210.8513442034533227, 23.64886208192143968 ) ) ;
#20350 = DIRECTION ( 'NONE',  ( 1.000000000000000000, 0.000000000000000000, 0.000000000000000000 ) ) ;
#20351 = EDGE_CURVE ( 'NONE', #7757, #24155, #7842, .T. ) ;
#20352 = CARTESIAN_POINT ( 'NONE',  ( 8.062137200540920645, 201.0835637161417822, 29.30113791807857027 ) ) ;
#20353 = DIRECTION ( 'NONE',  ( 1.000000000000000000, 0.000000000000000000, 0.000000000000000000 ) ) ;
#20354 = CARTESIAN_POINT ( 'NONE',  ( 3.044812012439969795, 216.5253028482143520, 99.39886208192145034 ) ) ;
#20355 = ADVANCED_FACE ( 'NONE', ( #23499 ), #166, .F. ) ;
#20356 = DIRECTION ( 'NONE',  ( -0.000000000000000000, -0.000000000000000000, -1.000000000000000000 ) ) ;
#20357 = PRESENTATION_LAYER_ASSIGNMENT (  '', '', ( #13299 ) ) ;
#20358 = VERTEX_POINT ( 'NONE', #18389 ) ;
#20359 = DIRECTION ( 'NONE',  ( 0.000000000000000000, 0.000000000000000000, 1.000000000000000000 ) ) ;
#20360 = CARTESIAN_POINT ( 'NONE',  ( 6.444103211790928043, 211.7408657792734061, 81.69886208192144750 ) ) ;
#20361 = CIRCLE ( 'NONE', #15995, 5.000000000000001776 ) ;
#20362 = ORIENTED_EDGE ( 'NONE', *, *, #19519, .F. ) ;
#20363 = CARTESIAN_POINT ( 'NONE',  ( 34.31132485994280756, 169.2658477444273331, 4.635254915624208216 ) ) ;
#20364 = EDGE_LOOP ( 'NONE', ( #23895, #19562, #3760, #20482 ) ) ;
#20365 = DIRECTION ( 'NONE',  ( -0.000000000000000000, -0.000000000000000000, -1.000000000000000000 ) ) ;
#20366 = CARTESIAN_POINT ( 'NONE',  ( 6.500168698208129925, 211.6636982574063381, 61.70113791807857240 ) ) ;
#20367 = CARTESIAN_POINT ( 'NONE',  ( 82.72499999726881015, 140.1801316387863778, -4.815267126137194431 ) ) ;
#20368 = EDGE_CURVE ( 'NONE', #24063, #20665, #8918, .T. ) ;
#20369 = CARTESIAN_POINT ( 'NONE',  ( -56.00000000000002132, 209.9999999999999716, 0.000000000000000000 ) ) ;
#20370 = CARTESIAN_POINT ( 'NONE',  ( 2.426778023690261410, 199.3768101843759837, 77.60113791807854966 ) ) ;
#20371 = DIRECTION ( 'NONE',  ( 1.000000000000000000, 0.000000000000000000, 0.000000000000000000 ) ) ;
#20372 =( NAMED_UNIT ( * ) PLANE_ANGLE_UNIT ( ) SI_UNIT ( $, .RADIAN. ) );
#20373 = CARTESIAN_POINT ( 'NONE',  ( 42.50000000000000000, 155.0000000000000000, -14.50000000000000711 ) ) ;
#20374 = CARTESIAN_POINT ( 'NONE',  ( 4.903702542908435547, 213.8346818373419751, 60.54886208192144181 ) ) ;
#20375 = EDGE_CURVE ( 'NONE', #6381, #6493, #19381, .T. ) ;
#20376 = CARTESIAN_POINT ( 'NONE',  ( -3.135527875058821579, 197.5041725223112223, -0.09886208192143428053 ) ) ;
#20377 = DIRECTION ( 'NONE',  ( -1.000000000000000000, 0.000000000000000000, 0.000000000000000000 ) ) ;
#20378 = VECTOR ( 'NONE', #4186, 1000.000000000000000 ) ;
#20379 = DIRECTION ( 'NONE',  ( 0.000000000000000000, 0.000000000000000000, -1.000000000000000000 ) ) ;
#20380 = CARTESIAN_POINT ( 'NONE',  ( 56.02499999726880731, 160.0630714827496206, 15.58253174999999224 ) ) ;
#20381 = CARTESIAN_POINT ( 'NONE',  ( 72.37499999726881583, 155.0000000000000000, 15.58253174999999402 ) ) ;
#20382 = CARTESIAN_POINT ( 'NONE',  ( 12.01549611932652972, 210.8513442034534933, 67.85113791807857808 ) ) ;
#20383 = CARTESIAN_POINT ( 'NONE',  ( -47.49999999999998579, 155.0000000000000000, -12.00000000000001066 ) ) ;
#20384 = CARTESIAN_POINT ( 'NONE',  ( 3.662846001190051659, 195.5725841191953691, 11.60113791807856742 ) ) ;
#20385 = CARTESIAN_POINT ( 'NONE',  ( 8.118202686958039038, 212.8392687619912635, 85.70113791807858661 ) ) ;
#20386 = CARTESIAN_POINT ( 'NONE',  ( -9.736236675708031640, 214.0148392665760753, 41.79886208192143471 ) ) ;
#20387 = CARTESIAN_POINT ( 'NONE',  ( 9.984503880673420539, 210.2968891136705736, 60.84886208192143187 ) ) ;
#20388 = CARTESIAN_POINT ( 'NONE',  ( -1.269541193505925744E-15, 7.895640089090863789, -6.564402953523717166 ) ) ;
#20389 = CARTESIAN_POINT ( 'NONE',  ( 7.456977232089302632, 217.1783343296989131, 97.55113791807858092 ) ) ;
#20390 = DIRECTION ( 'NONE',  ( 1.000000000000000000, 0.000000000000000000, 0.000000000000000000 ) ) ;
#20391 = CARTESIAN_POINT ( 'NONE',  ( -0.05014649552810635652, 196.4853777576173002, 2.751137918078565114 ) ) ;
#20392 = CARTESIAN_POINT ( 'NONE',  ( -6.139770520408224463, 198.4640165459539389, 74.04886208192142760 ) ) ;
#20393 = DIRECTION ( 'NONE',  ( 1.000000000000000000, 0.000000000000000000, 0.000000000000000000 ) ) ;
#20394 = ORIENTED_EDGE ( 'NONE', *, *, #21184, .T. ) ;
#20395 = CARTESIAN_POINT ( 'NONE',  ( 11.98450388067341876, 210.9467285061363953, 66.84886208192143897 ) ) ;
#20396 = CARTESIAN_POINT ( 'NONE',  ( 0.05014649552810505201, 217.5146222423826714, 91.25113791807858377 ) ) ;
#20397 = ORIENTED_EDGE ( 'NONE', *, *, #7919, .T. ) ;
#20398 = CARTESIAN_POINT ( 'NONE',  ( 79.87499999726880162, 171.3844434931184253, -7.942151717890132712E-15 ) ) ;
#20399 = CARTESIAN_POINT ( 'NONE',  ( -7.984503880673422316, 204.3529502787951628, 53.34886208192144608 ) ) ;
#20400 = ORIENTED_EDGE ( 'NONE', *, *, #5018, .F. ) ;
#20401 = EDGE_CURVE ( 'NONE', #30922, #18140, #26335, .T. ) ;
#20402 = CARTESIAN_POINT ( 'NONE',  ( 70.82499999726881867, 141.7447067706911810, -9.630534252274387086 ) ) ;
#20403 = CARTESIAN_POINT ( 'NONE',  ( 6.500000000000000888, 1.355443906731431669, -5.756734754743127347 ) ) ;
#20404 = DIRECTION ( 'NONE',  ( 0.000000000000000000, 0.9988620819214349966, -0.04769215134146094492 ) ) ;
#20405 = CARTESIAN_POINT ( 'NONE',  ( 66.02499999726879309, 160.0630714827496206, 15.58253174999999402 ) ) ;
#20406 = EDGE_CURVE ( 'NONE', #24364, #31583, #21598, .T. ) ;
#20407 = CARTESIAN_POINT ( 'NONE',  ( 2.000000000000000000, 1.773042676681340968, -2.276824562219559311E-15 ) ) ;
#20408 = CARTESIAN_POINT ( 'NONE',  ( -10.00000000000000711, 206.9523078486584495, 56.49886208192143755 ) ) ;
#20409 = ORIENTED_EDGE ( 'NONE', *, *, #20196, .T. ) ;
#20410 = CARTESIAN_POINT ( 'NONE',  ( 0.000000000000000000, 0.000000000000000000, 0.000000000000000000 ) ) ;
#20411 =( NAMED_UNIT ( * ) PLANE_ANGLE_UNIT ( ) SI_UNIT ( $, .RADIAN. ) );
#20412 = CARTESIAN_POINT ( 'NONE',  ( 7.500000000000001776, 0.000000000000000000, 0.000000000000000000 ) ) ;
#20413 = CARTESIAN_POINT ( 'NONE',  ( 6.444103211790928043, 211.7408657792734061, 21.69886208192144039 ) ) ;
#20414 = EDGE_CURVE ( 'NONE', #31059, #5646, #2953, .T. ) ;
#20415 = CARTESIAN_POINT ( 'NONE',  ( 8.062137200540920645, 201.0835637161417822, 68.30113791807856671 ) ) ;
#20416 = CARTESIAN_POINT ( 'NONE',  ( 92.60208470531341618, 155.0000000000000000, -12.10452846326765020 ) ) ;
#20417 = CARTESIAN_POINT ( 'NONE',  ( -3.044812012440131443, 216.5253028482142952, 55.10113791807857098 ) ) ;
#20418 = CARTESIAN_POINT ( 'NONE',  ( -10.00000000000000711, 207.0476921513413515, 24.50113791807856600 ) ) ;
#20419 = CARTESIAN_POINT ( 'NONE',  ( 8.000000000000008882, 206.9523078486586485, 2.001137918078566003 ) ) ;
#20420 = CARTESIAN_POINT ( 'NONE',  ( -6.539196172009840602, 3.775406670193650172, -6.286444963328100322 ) ) ;
#20421 = DIRECTION ( 'NONE',  ( 0.000000000000000000, 0.000000000000000000, 1.000000000000000000 ) ) ;
#20422 = CARTESIAN_POINT ( 'NONE',  ( 36.82499999726881157, 141.7447067706911810, -9.630534252274387086 ) ) ;
#20423 = CARTESIAN_POINT ( 'NONE',  ( -3.662846001190052991, 218.4274158808045740, 25.10113791807856742 ) ) ;
#20424 = CARTESIAN_POINT ( 'NONE',  ( 6.500000000000000000, -3.752776749732574135, -6.064240316920400886 ) ) ;
#20425 = CARTESIAN_POINT ( 'NONE',  ( -10.00000000000000711, 207.0476921513413515, 84.50113791807856956 ) ) ;
#20426 = CARTESIAN_POINT ( 'NONE',  ( 3.044812012440130555, 197.4746971517856764, 50.60113791807857808 ) ) ;
#20427 = CARTESIAN_POINT ( 'NONE',  ( 100.3007760113082156, 155.0000000000000000, 0.000000000000000000 ) ) ;
#20428 = CARTESIAN_POINT ( 'NONE',  ( -3.753561863808878130, 218.3979405102790281, 9.098862081921435419 ) ) ;
#20429 = CARTESIAN_POINT ( 'NONE',  ( -3.135527875058982783, 216.4958274776886924, 30.09886208192143897 ) ) ;
#20430 = CARTESIAN_POINT ( 'NONE',  ( 70.09999999453762598, 159.7113355953771077, -14.50000000000000888 ) ) ;
#20431 = VERTEX_POINT ( 'NONE', #3713 ) ;
#20432 = CARTESIAN_POINT ( 'NONE',  ( 9.736236675707914401, 214.0148392665762458, 58.70113791807857240 ) ) ;
#20433 = CARTESIAN_POINT ( 'NONE',  ( 7.984503880673485376, 204.3529502787953902, 83.15113791807856103 ) ) ;
#20434 = CARTESIAN_POINT ( 'NONE',  ( -0.05014649552828403384, 217.5146222423826714, 36.24886208192143755 ) ) ;
#20435 = FACE_OUTER_BOUND ( 'NONE', #23036, .T. ) ;
#20436 = ORIENTED_EDGE ( 'NONE', *, *, #15135, .F. ) ;
#20437 = CARTESIAN_POINT ( 'NONE',  ( 11.98450388067341876, 210.9467285061363953, 39.84886208192143187 ) ) ;
#20438 = ORIENTED_EDGE ( 'NONE', *, *, #3445, .F. ) ;
#20439 = ORIENTED_EDGE ( 'NONE', *, *, #16025, .T. ) ;
#20440 = EDGE_CURVE ( 'NONE', #16934, #33504, #14102, .T. ) ;
#20441 = CARTESIAN_POINT ( 'NONE',  ( 50.78867513459482552, 155.0000000000000000, -15.00000000000002487 ) ) ;
#20442 = ORIENTED_EDGE ( 'NONE', *, *, #2735, .T. ) ;
#20443 = CARTESIAN_POINT ( 'NONE',  ( 2.517493886308900919, 214.5937144450984420, 34.40113791807856813 ) ) ;
#20444 = EDGE_CURVE ( 'NONE', #12386, #18911, #23617, .T. ) ;
#20445 = LINE ( 'NONE', #22997, #33023 ) ;
#20446 = CARTESIAN_POINT ( 'NONE',  ( 9.984503880673420539, 210.2968891136705167, 9.848862081921435419 ) ) ;
#20447 = CARTESIAN_POINT ( 'NONE',  ( 55.27499999726881441, 149.9369285172503510, -15.58253175000000823 ) ) ;
#20448 = ORIENTED_EDGE ( 'NONE', *, *, #10868, .T. ) ;
#20449 = CARTESIAN_POINT ( 'NONE',  ( 4.903702542908601636, 200.1653181626581102, 59.45113791807857240 ) ) ;
#20450 = DIRECTION ( 'NONE',  ( -0.7071067811865355823, 8.659560562355079537E-17, -0.7071067811865595631 ) ) ;
#20451 = SHAPE_REPRESENTATION_RELATIONSHIP ( 'NONE' , 'NONE' ,  #30038, #1094 ) ;
#20452 = DIRECTION ( 'NONE',  ( -1.000000000000000000, 0.000000000000000000, 0.000000000000000000 ) ) ;
#20453 = CARTESIAN_POINT ( 'NONE',  ( 3.135527875058981895, 197.5041725223112792, 103.5988620819214390 ) ) ;
#20454 = CARTESIAN_POINT ( 'NONE',  ( 65.97499999726881015, 169.8198683612136222, 4.815267126137181997 ) ) ;
#20455 = CARTESIAN_POINT ( 'NONE',  ( 10.01549611932653860, 210.2015048109876716, 37.85113791807854966 ) ) ;
#20456 =( BOUNDED_CURVE ( )  B_SPLINE_CURVE ( 2, ( #6504, #16715, #21496, #5818, #6153, #14165, #11279, #21662, #717, #1058, #3432 ),
 .UNSPECIFIED., .F., .T. ) 
 B_SPLINE_CURVE_WITH_KNOTS ( ( 3, 2, 2, 2, 2, 3 ),
 ( 0.3928571428571426827, 0.3964285714285712414, 0.3999999999999998002, 0.4035714285714283589, 0.4071428571428570287, 0.4107142857142855874 ),
 .UNSPECIFIED. ) 
 CURVE ( )  GEOMETRIC_REPRESENTATION_ITEM ( )  RATIONAL_B_SPLINE_CURVE ( ( 1.000000000000001554, 0.9510565162951518658, 1.000000000000000000, 0.9510565162951534202, 1.000000000000000000, 0.9510565162951534202, 1.000000000000000000, 0.9510565162951534202, 1.000000000000000000, 0.9510565162951549745, 0.9999999999999984457 ) ) 
 REPRESENTATION_ITEM ( '' )  );
#20457 = CARTESIAN_POINT ( 'NONE',  ( -9.984503880673473830, 210.2968891136704315, 27.65113791807855748 ) ) ;
#20458 = DIRECTION ( 'NONE',  ( 0.000000000000000000, 0.000000000000000000, -1.000000000000000000 ) ) ;
#20459 = APPLICATION_PROTOCOL_DEFINITION ( 'draft international standard', 'automotive_design', 1998, #31616 ) ;
#20460 = CARTESIAN_POINT ( 'NONE',  ( 84.50000000000000000, 155.0000000000000000, -14.50000000000000711 ) ) ;
#20461 = FACE_OUTER_BOUND ( 'NONE', #13853, .T. ) ;
#20462 = CARTESIAN_POINT ( 'NONE',  ( 67.50000000000000000, 155.0000000000000000, -6.938893903907228378E-15 ) ) ;
#20463 = CARTESIAN_POINT ( 'NONE',  ( 12.01549611932652972, 210.8513442034534933, 1.851137918078565647 ) ) ;
#20464 = CARTESIAN_POINT ( 'NONE',  ( 63.88867513459482694, 150.1262045565063659, 14.99999999999997158 ) ) ;
#20465 = CARTESIAN_POINT ( 'NONE',  ( 49.37499999726880873, 155.0000000000000000, -15.58253175000000823 ) ) ;
#20466 = CARTESIAN_POINT ( 'NONE',  ( -6.139770520408369237, 215.5359834540460042, 48.95113791807855108 ) ) ;
#20467 = FACE_OUTER_BOUND ( 'NONE', #31373, .T. ) ;
#20468 = CARTESIAN_POINT ( 'NONE',  ( 77.71132485994280614, 155.0000000000000000, -15.00000000000002487 ) ) ;
#20469 = CARTESIAN_POINT ( 'NONE',  ( 127.5000000000000000, 155.0000000000010800, 106.0000000000000142 ) ) ;
#20470 = CARTESIAN_POINT ( 'NONE',  ( 57.19999999453763451, 146.4771138417591203, 11.73074641843673227 ) ) ;
#20471 = ORIENTED_EDGE ( 'NONE', *, *, #12853, .T. ) ;
#20472 = CARTESIAN_POINT ( 'NONE',  ( -9.736236675707914401, 199.9851607334237542, 27.20113791807857240 ) ) ;
#20473 = CARTESIAN_POINT ( 'NONE',  ( 117.5000000000000000, 248.9486928011511679, 52.99999999999880629 ) ) ;
#20474 = CARTESIAN_POINT ( 'NONE',  ( 8.062137200540822946, 212.9164362838583315, 9.698862081921435063 ) ) ;
#20475 = CARTESIAN_POINT ( 'NONE',  ( 60.61132485994281183, 159.8737954434935489, 15.00000000000006040 ) ) ;
#20476 = EDGE_LOOP ( 'NONE', ( #27426, #6302, #5674 ) ) ;
#20477 = CARTESIAN_POINT ( 'NONE',  ( -9.984503880673473830, 210.2968891136704315, 9.651137918078568134 ) ) ;
#20478 = CARTESIAN_POINT ( 'NONE',  ( -6.220909254589537696, 198.5229672870051161, 72.05113791807853829 ) ) ;
#20479 = ORIENTED_EDGE ( 'NONE', *, *, #23497, .T. ) ;
#20480 = CARTESIAN_POINT ( 'NONE',  ( 6.500168698208244500, 202.3363017425938324, 25.29886208192143826 ) ) ;
#20481 = DIRECTION ( 'NONE',  ( 0.000000000000000000, 0.000000000000000000, -1.000000000000000000 ) ) ;
#20482 = ORIENTED_EDGE ( 'NONE', *, *, #22715, .F. ) ;
#20483 = CARTESIAN_POINT ( 'NONE',  ( 8.000000000000008882, 206.9523078486586485, 8.001137918078566003 ) ) ;
#20484 = AXIS2_PLACEMENT_3D ( 'NONE', #30706, #25751, #15022 ) ;
#20485 = CARTESIAN_POINT ( 'NONE',  ( 11.98450388067341876, 210.9467285061363953, 84.84886208192142476 ) ) ;
#20486 = CARTESIAN_POINT ( 'NONE',  ( 37.87499999726880873, 171.3844434931184253, -7.942151717890134290E-15 ) ) ;
#20487 = ORIENTED_EDGE ( 'NONE', *, *, #7878, .T. ) ;
#20488 = CARTESIAN_POINT ( 'NONE',  ( 42.92499999726881299, 145.8408176439707802, -12.60653300113719588 ) ) ;
#20489 = EDGE_CURVE ( 'NONE', #26841, #18587, #20361, .T. ) ;
#20490 = CARTESIAN_POINT ( 'NONE',  ( 129.1982509225904039, 3.226370279868336244, 35.00001199999999102 ) ) ;
#20491 = CARTESIAN_POINT ( 'NONE',  ( 8.118202686958039038, 212.8392687619912635, 4.701137918078565292 ) ) ;
#20492 = CARTESIAN_POINT ( 'NONE',  ( 10.01549611932659545, 203.7984951890123853, 73.14886208192143613 ) ) ;
#20493 = CARTESIAN_POINT ( 'NONE',  ( 44.27499999726881441, 160.0630714827496206, 15.58253174999999402 ) ) ;
#20494 = CARTESIAN_POINT ( 'NONE',  ( -67.50001199999998391, 144.6301735379005038, 13.51682963488643807 ) ) ;
#20495 = CARTESIAN_POINT ( 'NONE',  ( -10.00000000000000711, 207.0476921513413515, 12.50113791807856778 ) ) ;
#20496 = DIRECTION ( 'NONE',  ( 0.000000000000000000, 0.000000000000000000, -1.000000000000000000 ) ) ;
#20497 = EDGE_CURVE ( 'NONE', #31619, #9541, #7421, .T. ) ;
#20498 = AXIS2_PLACEMENT_3D ( 'NONE', #7304, #32668, #22447 ) ;
#20499 = CARTESIAN_POINT ( 'NONE',  ( 69.70000000000001705, 146.4771138417591203, 11.73074641843673227 ) ) ;
#20500 = CARTESIAN_POINT ( 'NONE',  ( -10.00000000000000711, 207.0476921513413515, 102.5011379180785838 ) ) ;
#20501 = CARTESIAN_POINT ( 'NONE',  ( -54.30000000000002558, -88.00000000000000000, 20.00000000000000000 ) ) ;
#20502 = CARTESIAN_POINT ( 'NONE',  ( -8.062137200540920645, 212.9164362838581894, 78.80113791807858092 ) ) ;
#20503 = CARTESIAN_POINT ( 'NONE',  ( 3.499999999999999556, 0.000000000000000000, 0.000000000000000000 ) ) ;
#20504 = CARTESIAN_POINT ( 'NONE',  ( 5.000000000000000000, 0.000000000000000000, 0.000000000000000000 ) ) ;
#20505 = CARTESIAN_POINT ( 'NONE',  ( 11.98450388067341876, 210.9467285061363953, 84.84886208192142476 ) ) ;
#20506 = CARTESIAN_POINT ( 'NONE',  ( 73.22499999726881015, 160.0630714827496206, -15.58253175000000823 ) ) ;
#20507 = ORIENTED_EDGE ( 'NONE', *, *, #8927, .T. ) ;
#20508 = CARTESIAN_POINT ( 'NONE',  ( -61.00005817115211926, 195.0000036356967712, -0.1622090645192997005 ) ) ;
#20509 = CARTESIAN_POINT ( 'NONE',  ( 34.89999999453762314, 159.7113355953771077, 14.49999999999999289 ) ) ;
#20510 = CARTESIAN_POINT ( 'NONE',  ( 12.00000000000000711, 206.9523078486586485, 92.00113791807858377 ) ) ;
#20511 = FACE_BOUND ( 'NONE', #33116, .T. ) ;
#20512 =( GEOMETRIC_REPRESENTATION_CONTEXT ( 3 ) GLOBAL_UNCERTAINTY_ASSIGNED_CONTEXT ( ( #790 ) ) GLOBAL_UNIT_ASSIGNED_CONTEXT ( ( #19917, #4080, #14806 ) ) REPRESENTATION_CONTEXT ( 'NONE', 'WORKASPACE' ) );
#20513 = ORIENTED_EDGE ( 'NONE', *, *, #5234, .T. ) ;
#20514 = CIRCLE ( 'NONE', #29744, 0.6186547224754559426 ) ;
#20515 = CARTESIAN_POINT ( 'NONE',  ( 0.05014649552828275014, 196.4853777576173002, 85.74886208192141623 ) ) ;
#20516 = CARTESIAN_POINT ( 'NONE',  ( -7.456977232089471386, 217.1783343296987709, 26.94886208192142973 ) ) ;
#20517 = LINE ( 'NONE', #25802, #12642 ) ;
#20518 = CARTESIAN_POINT ( 'NONE',  ( 6.220909254589536808, 215.4770327129947702, 43.55113791807857382 ) ) ;
#20519 = VERTEX_POINT ( 'NONE', #13430 ) ;
#20520 = CARTESIAN_POINT ( 'NONE',  ( -9.984503880673420539, 203.7031108863293980, 101.3488620819213963 ) ) ;
#20521 = LINE ( 'NONE', #30415, #6136 ) ;
#20522 = ORIENTED_EDGE ( 'NONE', *, *, #26650, .F. ) ;
#20523 = CARTESIAN_POINT ( 'NONE',  ( -4.984841277089891776, 213.7757310962905990, 80.94886208192143329 ) ) ;
#20524 = EDGE_LOOP ( 'NONE', ( #29104, #8650, #33303, #26590, #18221, #11677 ) ) ;
#20525 = CARTESIAN_POINT ( 'NONE',  ( 87.50000000000002842, 169.3860439379083402, -5.988074444788474615 ) ) ;
#20526 = VERTEX_POINT ( 'NONE', #24160 ) ;
#20527 = CARTESIAN_POINT ( 'NONE',  ( 64.50000000000000000, -103.0000000000000000, -20.00000000000000000 ) ) ;
#20528 = CARTESIAN_POINT ( 'NONE',  ( -2.517493886308901807, 199.4062855549015012, 62.90113791807858945 ) ) ;
#20529 = CARTESIAN_POINT ( 'NONE',  ( 82.92499999726882720, 145.8408176439707802, -12.60653300113719588 ) ) ;
#20530 = DIRECTION ( 'NONE',  ( 0.000000000000000000, 0.000000000000000000, -1.000000000000000000 ) ) ;
#20531 = CARTESIAN_POINT ( 'NONE',  ( -2.517493886308901807, 199.4062855549015012, 83.90113791807856103 ) ) ;
#20532 = CARTESIAN_POINT ( 'NONE',  ( 2.000000000000000000, -1.773042676681340524, 1.734723475976807094E-15 ) ) ;
#20533 = EDGE_CURVE ( 'NONE', #29612, #5632, #11549, .T. ) ;
#20534 = AXIS2_PLACEMENT_3D ( 'NONE', #12726, #7284, #25497 ) ;
#20535 = CARTESIAN_POINT ( 'NONE',  ( 47.80000000000000426, 142.6655632788954620, 8.961492836873471646 ) ) ;
#20536 = CARTESIAN_POINT ( 'NONE',  ( -7.984503880673422316, 204.3529502787951628, 59.34886208192144608 ) ) ;
#20537 = CARTESIAN_POINT ( 'NONE',  ( 38.61132485994280472, 159.8737954434936910, 14.99999999999996447 ) ) ;
#20538 = AXIS2_PLACEMENT_3D ( 'NONE', #32423, #3982, #11318 ) ;
#20539 = EDGE_CURVE ( 'NONE', #734, #866, #3494, .T. ) ;
#20540 = CARTESIAN_POINT ( 'NONE',  ( 0.05014649552810506589, 217.5146222423826714, 1.251137918078566003 ) ) ;
#20541 = CARTESIAN_POINT ( 'NONE',  ( -5.000000000000000888, 5.773502691896258199, -7.063244554130002406 ) ) ;
#20542 = CARTESIAN_POINT ( 'NONE',  ( 27.50000000000000000, 6.731471899275976334, -17.54777384619328018 ) ) ;
#20543 = CARTESIAN_POINT ( 'NONE',  ( 56.82499999726881157, 141.7447067706911810, -9.630534252274387086 ) ) ;
#20544 = CARTESIAN_POINT ( 'NONE',  ( 71.37499999726881583, 155.0000000000000000, -15.58253175000000823 ) ) ;
#20545 = CARTESIAN_POINT ( 'NONE',  ( 12.00000000000000711, 206.9523078486586485, 65.00113791807856956 ) ) ;
#20546 = CARTESIAN_POINT ( 'NONE',  ( 46.71132485994281325, 155.0000000000000000, 15.00000000000001243 ) ) ;
#20547 = CARTESIAN_POINT ( 'NONE',  ( 11.98450388067348271, 203.0532714938637753, 11.15113791807856636 ) ) ;
#20548 = CARTESIAN_POINT ( 'NONE',  ( -9.984503880673475606, 210.2968891136704315, 84.65113791807857524 ) ) ;
#20549 = CARTESIAN_POINT ( 'NONE',  ( 9.736236675708031640, 199.9851607334238963, 49.29886208192143471 ) ) ;
#20550 = CARTESIAN_POINT ( 'NONE',  ( 8.118202686958138514, 201.1607312380088501, 55.29886208192144181 ) ) ;
#20551 = CARTESIAN_POINT ( 'NONE',  ( -63.50000000000004263, 215.0000000000000000, -2.500000000000000000 ) ) ;
#20552 = CARTESIAN_POINT ( 'NONE',  ( -7.456977232089304408, 196.8216656703010301, 99.05113791807858092 ) ) ;
#20553 = DIRECTION ( 'NONE',  ( 0.000000000000000000, 0.000000000000000000, -1.000000000000000000 ) ) ;
#20554 = CONICAL_SURFACE ( 'NONE', #11846, 6.500000000000000888, 0.8987552595851582282 ) ;
#20555 = CARTESIAN_POINT ( 'NONE',  ( 6.220909254589536808, 215.4770327129947702, 4.551137918078564937 ) ) ;
#20556 = CARTESIAN_POINT ( 'NONE',  ( -6.139770520408224463, 198.4640165459539389, 65.04886208192144181 ) ) ;
#20557 = CONICAL_SURFACE ( 'NONE', #29258, 12.00000000000001066, 0.1047197551196174109 ) ;
#20558 = DIRECTION ( 'NONE',  ( -1.000000000000000000, 0.000000000000000000, 0.000000000000000000 ) ) ;
#20559 = ORIENTED_EDGE ( 'NONE', *, *, #29077, .F. ) ;
#20560 = CARTESIAN_POINT ( 'NONE',  ( 12.01549611932659367, 203.1486557965466773, 79.14886208192143613 ) ) ;
#20561 = MECHANICAL_DESIGN_GEOMETRIC_PRESENTATION_REPRESENTATION (  '', ( #19460 ), #22751 ) ;
#20562 = CARTESIAN_POINT ( 'NONE',  ( -10.01549611932653860, 203.7984951890123284, 93.35113791807857808 ) ) ;
#20563 = ORIENTED_EDGE ( 'NONE', *, *, #14726, .F. ) ;
#20564 = CARTESIAN_POINT ( 'NONE',  ( 77.27499999726880731, 149.9369285172503510, -15.58253175000000823 ) ) ;
#20565 = CARTESIAN_POINT ( 'NONE',  ( -6.444103211790928043, 202.2591342207265939, 53.19886208192144039 ) ) ;
#20566 = ADVANCED_FACE ( 'NONE', ( #11216 ), #11058, .F. ) ;
#20567 = ORIENTED_EDGE ( 'NONE', *, *, #13352, .T. ) ;
#20568 = CONICAL_SURFACE ( 'NONE', #30916, 11.99999999999998224, 0.1047197551196726167 ) ;
#20569 = CARTESIAN_POINT ( 'NONE',  ( 71.92499999726881299, 164.1591823560292198, 12.60653300113718167 ) ) ;
#20570 = CARTESIAN_POINT ( 'NONE',  ( 6.832273232158034837, 3.329759989367264694, -6.449140625371624580 ) ) ;
#20571 = CARTESIAN_POINT ( 'NONE',  ( 111.1125082318798007, 155.0000000000000000, 32.00000000000002842 ) ) ;
#20572 = CARTESIAN_POINT ( 'NONE',  ( 61.52499999726881441, 169.8198683612136222, -4.815267126137197984 ) ) ;
#20573 = DIRECTION ( 'NONE',  ( 0.000000000000000000, -0.5000000000000011102, -0.8660254037844379305 ) ) ;
#20574 = EDGE_CURVE ( 'NONE', #27759, #18729, #25810, .T. ) ;
#20575 = CARTESIAN_POINT ( 'NONE',  ( -9.984503880673420539, 203.7031108863293980, 50.34886208192141765 ) ) ;
#20576 = ORIENTED_EDGE ( 'NONE', *, *, #27010, .F. ) ;
#20577 = FACE_OUTER_BOUND ( 'NONE', #30356, .T. ) ;
#20578 =( LENGTH_UNIT ( ) NAMED_UNIT ( * ) SI_UNIT ( .MILLI., .METRE. ) );
#20579 = LINE ( 'NONE', #30984, #18664 ) ;
#20580 = CARTESIAN_POINT ( 'NONE',  ( -4.984841277089891776, 213.7757310962905990, 38.94886208192144039 ) ) ;
#20581 = CIRCLE ( 'NONE', #993, 16.00000000000000000 ) ;
#20582 = CARTESIAN_POINT ( 'NONE',  ( -6.139770520408369237, 215.5359834540460042, 69.95113791807857240 ) ) ;
#20583 = DIRECTION ( 'NONE',  ( 0.000000000000000000, -1.000000000000000000, 9.682177540335733218E-15 ) ) ;
#20584 = CARTESIAN_POINT ( 'NONE',  ( -8.062137200540920645, 212.9164362838581894, 57.80113791807857382 ) ) ;
#20585 = AXIS2_PLACEMENT_3D ( 'NONE', #14609, #11889, #4211 ) ;
#20586 = CONTEXT_DEPENDENT_SHAPE_REPRESENTATION ( #4658, #10903 ) ;
#20587 = ADVANCED_FACE ( 'NONE', ( #31823 ), #13766, .F. ) ;
#20588 = CARTESIAN_POINT ( 'NONE',  ( 8.118202686958039038, 212.8392687619912635, 28.70113791807856884 ) ) ;
#20589 = CARTESIAN_POINT ( 'NONE',  ( 4.984841277089725686, 213.7757310962907411, 19.55113791807856671 ) ) ;
#20590 = CARTESIAN_POINT ( 'NONE',  ( -58.50000000000002132, 209.9999999999999716, 0.000000000000000000 ) ) ;
#20591 = CARTESIAN_POINT ( 'NONE',  ( 10.00000000000000888, 207.9248754155063637, 0.9569796661747027589 ) ) ;
#20592 = CARTESIAN_POINT ( 'NONE',  ( 39.42499999726881299, 168.2552932293087906, -9.630534252274387086 ) ) ;
#20593 = CARTESIAN_POINT ( 'NONE',  ( 7.375838497908181246, 196.7627149292499666, 41.45113791807857240 ) ) ;
#20594 = DIRECTION ( 'NONE',  ( 1.000000000000000000, 0.000000000000000000, 0.000000000000000000 ) ) ;
#20595 = CARTESIAN_POINT ( 'NONE',  ( 8.118202686958039038, 212.8392687619912635, 88.70113791807857240 ) ) ;
#20596 = CARTESIAN_POINT ( 'NONE',  ( -8.118202686958039038, 201.1607312380087080, 63.20113791807857240 ) ) ;
#20597 = DIRECTION ( 'NONE',  ( 0.000000000000000000, -0.7071067811865506814, -0.7071067811865442421 ) ) ;
#20598 = CARTESIAN_POINT ( 'NONE',  ( -3.662846001189865142, 195.5725841191952838, 19.89886208192143613 ) ) ;
#20599 = CARTESIAN_POINT ( 'NONE',  ( 3.044812012439969795, 216.5253028482143520, 30.39886208192143613 ) ) ;
#20600 = CARTESIAN_POINT ( 'NONE',  ( 70.79999999453761461, 163.5228861582408797, 11.73074641843673049 ) ) ;
#20601 = EDGE_LOOP ( 'NONE', ( #15608, #4467, #24459 ) ) ;
#20602 = CARTESIAN_POINT ( 'NONE',  ( 3.753561863808689836, 218.3979405102790565, 70.40113791807856103 ) ) ;
#20603 = CARTESIAN_POINT ( 'NONE',  ( -6.444103211791042618, 211.7408657792732356, 78.80113791807858092 ) ) ;
#20604 = ADVANCED_FACE ( 'NONE', ( #5926 ), #16319, .F. ) ;
#20605 = CARTESIAN_POINT ( 'NONE',  ( 10.01549611932659545, 203.7984951890123853, 43.14886208192142192 ) ) ;
#20606 = CARTESIAN_POINT ( 'NONE',  ( 74.71132485994280614, 155.0000000000000000, 15.00000000000001243 ) ) ;
#20607 = VERTEX_POINT ( 'NONE', #16485 ) ;
#20608 = CARTESIAN_POINT ( 'NONE',  ( 0.05014649552828288198, 194.3824533091408000, 49.74886208192143044 ) ) ;
#20609 = ORIENTED_EDGE ( 'NONE', *, *, #18558, .T. ) ;
#20610 = CIRCLE ( 'NONE', #22224, 4.199999999999988631 ) ;
#20611 = EDGE_CURVE ( 'NONE', #23539, #8526, #4028, .T. ) ;
#20612 = VERTEX_POINT ( 'NONE', #19718 ) ;
#20613 = PRODUCT_DEFINITION_SHAPE ( 'NONE', 'NONE',  #33688 ) ;
#20614 = AXIS2_PLACEMENT_3D ( 'NONE', #31950, #13896, #20906 ) ;
#20615 = CARTESIAN_POINT ( 'NONE',  ( 6.815830331203685866, 1.228021141713631082E-13, -6.171384342982610960 ) ) ;
#20616 = CARTESIAN_POINT ( 'NONE',  ( -67.50000000000000000, 122.1366465496900275, 17.00000000000001421 ) ) ;
#20617 = VERTEX_POINT ( 'NONE', #17498 ) ;
#20618 = CARTESIAN_POINT ( 'NONE',  ( 4.903702542908601636, 200.1653181626581102, 44.45113791807857240 ) ) ;
#20619 = CARTESIAN_POINT ( 'NONE',  ( 10.01549611932659545, 203.7984951890123853, 25.14886208192143613 ) ) ;
#20620 = CARTESIAN_POINT ( 'NONE',  ( 60.27499999726881441, 160.0630714827496206, 15.58253174999999224 ) ) ;
#20621 = ORIENTED_EDGE ( 'NONE', *, *, #3894, .T. ) ;
#20622 = DIRECTION ( 'NONE',  ( 0.000000000000000000, 0.000000000000000000, -1.000000000000000000 ) ) ;
#20623 = FACE_OUTER_BOUND ( 'NONE', #28991, .T. ) ;
#20624 = CARTESIAN_POINT ( 'NONE',  ( -6.444103211790928043, 202.2591342207265939, 8.198862081921436840 ) ) ;
#20625 = CARTESIAN_POINT ( 'NONE',  ( 10.00000000000000711, 206.9523078486586201, 41.00113791807856956 ) ) ;
#20626 = CARTESIAN_POINT ( 'NONE',  ( 10.00000000000000711, 206.9523078486586201, 29.00113791807856956 ) ) ;
#20627 = CARTESIAN_POINT ( 'NONE',  ( 6.139770520408223575, 215.5359834540460611, 102.5488620819214134 ) ) ;
#20628 = B_SPLINE_CURVE_WITH_KNOTS ( 'NONE', 3,
 ( #27741, #14789, #12239, #2022, #12411, #9010 ),
 .UNSPECIFIED., .F., .F.,
 ( 4, 2, 4 ),
 ( 0.002044882221487503288, 0.003063384235218505423, 0.004081886248949507558 ),
 .UNSPECIFIED. ) ;
#20629 = SHAPE_DEFINITION_REPRESENTATION ( #15154, #16098 ) ;
#20630 = CARTESIAN_POINT ( 'NONE',  ( 2.517493886309087436, 199.4062855549015865, 79.59886208192143897 ) ) ;
#20631 = CARTESIAN_POINT ( 'NONE',  ( 33.72499999726881725, 169.8198683612136222, 4.815267126137181997 ) ) ;
#20632 = LINE ( 'NONE', #15346, #3914 ) ;
#20633 = CARTESIAN_POINT ( 'NONE',  ( 12.01549611932652972, 210.8513442034534933, 7.851137918078565647 ) ) ;
#20634 = AXIS2_PLACEMENT_3D ( 'NONE', #24776, #14209, #32603 ) ;
#20635 = FACE_BOUND ( 'NONE', #1821, .T. ) ;
#20636 = CARTESIAN_POINT ( 'NONE',  ( 52.17499999726880588, 164.1591823560292198, 12.60653300113718167 ) ) ;
#20637 = EDGE_CURVE ( 'NONE', #19921, #13301, #22277, .T. ) ;
#20638 = CARTESIAN_POINT ( 'NONE',  ( -8.062137200540920645, 212.9164362838581894, 60.80113791807857382 ) ) ;
#20639 = EDGE_CURVE ( 'NONE', #25814, #9574, #8092, .T. ) ;
#20640 = DIRECTION ( 'NONE',  ( 0.000000000000000000, -1.000000000000000000, 1.290957005378097920E-14 ) ) ;
#20641 = AXIS2_PLACEMENT_3D ( 'NONE', #508, #20452, #13 ) ;
#20642 = CARTESIAN_POINT ( 'NONE',  ( 78.41132485994280898, 167.7597621252805880, 9.270509831248428867 ) ) ;
#20643 = CARTESIAN_POINT ( 'NONE',  ( -8.062137200540822946, 201.0835637161416400, 2.198862081921434175 ) ) ;
#20644 = CARTESIAN_POINT ( 'NONE',  ( 50.99999999453763166, 155.0000000000000000, 14.49999999999999467 ) ) ;
#20645 = EDGE_LOOP ( 'NONE', ( #5016, #13108, #17022, #4762 ) ) ;
#20646 = CARTESIAN_POINT ( 'NONE',  ( -12.01549611932652972, 203.1486557965464499, 36.35113791807856387 ) ) ;
#20647 = EDGE_CURVE ( 'NONE', #13027, #31548, #15470, .T. ) ;
#20648 = PRODUCT_RELATED_PRODUCT_CATEGORY ( 'part', '', ( #30091 ) ) ;
#20649 = ADVANCED_FACE ( 'NONE', ( #27727 ), #9497, .F. ) ;
#20650 = LINE ( 'NONE', #28139, #7283 ) ;
#20651 = CARTESIAN_POINT ( 'NONE',  ( 6.220909254589681581, 198.5229672870052582, 16.44886208192143329 ) ) ;
#20652 = CARTESIAN_POINT ( 'NONE',  ( 60.01132485994281041, 167.7597621252805880, -9.270509831248443078 ) ) ;
#20653 = VERTEX_POINT ( 'NONE', #14949 ) ;
#20654 = CARTESIAN_POINT ( 'NONE',  ( 10.01549611932653860, 210.2015048109876716, 10.85113791807856387 ) ) ;
#20655 = CARTESIAN_POINT ( 'NONE',  ( 3.044812012440130555, 197.4746971517856764, 68.60113791807857808 ) ) ;
#20656 = VERTEX_POINT ( 'NONE', #11719 ) ;
#20657 = CARTESIAN_POINT ( 'NONE',  ( 0.05014649552828262524, 198.5883022060938572, 28.74886208192144110 ) ) ;
#20658 = DIRECTION ( 'NONE',  ( 0.000000000000000000, 0.000000000000000000, -1.000000000000000000 ) ) ;
#20659 = CARTESIAN_POINT ( 'NONE',  ( 78.77499999726880731, 140.1801316387863778, 4.815267126137185549 ) ) ;
#20660 = ORIENTED_EDGE ( 'NONE', *, *, #434, .F. ) ;
#20661 = CARTESIAN_POINT ( 'NONE',  ( -6.444103211791042618, 211.7408657792732356, 15.80113791807856849 ) ) ;
#20662 = AXIS2_PLACEMENT_3D ( 'NONE', #31850, #13460, #18584 ) ;
#20663 = CARTESIAN_POINT ( 'NONE',  ( 7.375838497908012492, 217.2372850707501186, 96.54886208192142760 ) ) ;
#20664 = CARTESIAN_POINT ( 'NONE',  ( 36.57499999726881157, 145.8408176439707802, 12.60653300113718345 ) ) ;
#20665 = VERTEX_POINT ( 'NONE', #6605 ) ;
#20666 = CARTESIAN_POINT ( 'NONE',  ( 44.22499999726880304, 149.9369285172503510, 15.58253174999999580 ) ) ;
#20667 = CYLINDRICAL_SURFACE ( 'NONE', #18098, 99.99999999999997158 ) ;
#20668 = CARTESIAN_POINT ( 'NONE',  ( -10.00000000000000711, 207.0476921513413515, 6.501137918078566003 ) ) ;
#20669 = CARTESIAN_POINT ( 'NONE',  ( 9.984503880673420539, 210.2968891136705167, 75.84886208192143897 ) ) ;
#20670 = CARTESIAN_POINT ( 'NONE',  ( 46.47499999726880304, 149.9369285172503510, 15.58253174999999580 ) ) ;
#20671 = CARTESIAN_POINT ( 'NONE',  ( 79.01132485994281751, 142.2402378747194405, 9.270509831248432420 ) ) ;
#20672 = CARTESIAN_POINT ( 'NONE',  ( 3.135527875058820690, 216.4958274776887492, 13.40113791807856636 ) ) ;
#20673 = CARTESIAN_POINT ( 'NONE',  ( 65.00000000000000000, 170.2462022514548323, -7.872454543227099337E-15 ) ) ;
#20674 = CARTESIAN_POINT ( 'NONE',  ( -3.044812012440131443, 216.5253028482142952, 97.10113791807857808 ) ) ;
#20675 = CARTESIAN_POINT ( 'NONE',  ( 111.1125082318798007, 155.0000000000000000, 32.00000000000002842 ) ) ;
#20676 = CARTESIAN_POINT ( 'NONE',  ( -9.984503880673473830, 210.2968891136704315, 81.65113791807857524 ) ) ;
#20677 = CARTESIAN_POINT ( 'NONE',  ( 104.9083388212530537, 155.0000000000000000, 0.000000000000000000 ) ) ;
#20678 = CARTESIAN_POINT ( 'NONE',  ( 27.50000000000000355, 0.000000000000000000, 0.000000000000000000 ) ) ;
#20679 = CARTESIAN_POINT ( 'NONE',  ( 9.736236675708031640, 199.9851607334238963, 100.2988620819214276 ) ) ;
#20680 = CARTESIAN_POINT ( 'NONE',  ( 67.42499999726879878, 168.2552932293087906, -9.630534252274385310 ) ) ;
#20681 = ORIENTED_EDGE ( 'NONE', *, *, #26611, .F. ) ;
#20682 = LINE ( 'NONE', #31080, #14070 ) ;
#20683 = CARTESIAN_POINT ( 'NONE',  ( 36.49999999453763166, 170.2462022514548323, -7.872454543227099337E-15 ) ) ;
#20684 = CARTESIAN_POINT ( 'NONE',  ( 12.01549611932652972, 210.8513442034534933, 91.85113791807857808 ) ) ;
#20685 = CARTESIAN_POINT ( 'NONE',  ( -10.37719565735124938, 206.0286316962952640, 104.3663993655802784 ) ) ;
#20686 = ORIENTED_EDGE ( 'NONE', *, *, #11444, .F. ) ;
#20687 = CARTESIAN_POINT ( 'NONE',  ( -3.044812012439970683, 197.4746971517856196, 88.89886208192143613 ) ) ;
#20688 = CARTESIAN_POINT ( 'NONE',  ( -12.00000000000000711, 206.9523078486584780, 20.49886208192143755 ) ) ;
#20689 = DIRECTION ( 'NONE',  ( 0.000000000000000000, -1.000000000000000000, 1.295896757998781966E-15 ) ) ;
#20690 = CARTESIAN_POINT ( 'NONE',  ( -8.118202686958039038, 201.1607312380087080, 45.20113791807857240 ) ) ;
#20691 = ORIENTED_EDGE ( 'NONE', *, *, #24584, .T. ) ;
#20692 = CARTESIAN_POINT ( 'NONE',  ( -4.903702542908436435, 200.1653181626580249, 2.048862081921434708 ) ) ;
#20693 = CARTESIAN_POINT ( 'NONE',  ( -3.376928366568182163E-14, -72.99999999999997158, 30.00000000000000000 ) ) ;
#20694 = ORIENTED_EDGE ( 'NONE', *, *, #18036, .T. ) ;
#20695 = CARTESIAN_POINT ( 'NONE',  ( -4.903702542908436435, 200.1653181626580249, 83.04886208192144181 ) ) ;
#20696 = ORIENTED_EDGE ( 'NONE', *, *, #11894, .F. ) ;
#20697 = CARTESIAN_POINT ( 'NONE',  ( 8.399999999999998579, 4.898587196589413815E-16, -4.000000000000000888 ) ) ;
#20698 = ORIENTED_EDGE ( 'NONE', *, *, #23335, .F. ) ;
#20699 = DIRECTION ( 'NONE',  ( -1.000000000000000000, -0.000000000000000000, -0.000000000000000000 ) ) ;
#20700 = CARTESIAN_POINT ( 'NONE',  ( 82.42499999726882720, 141.7447067706911810, 9.630534252274376428 ) ) ;
#20701 = DIRECTION ( 'NONE',  ( -1.000000000000000000, 0.000000000000000000, 0.000000000000000000 ) ) ;
#20702 = CARTESIAN_POINT ( 'NONE',  ( 6.500168698208129925, 211.6636982574063381, 85.70113791807858661 ) ) ;
#20703 = DIRECTION ( 'NONE',  ( -1.000000000000000000, 0.000000000000000000, 0.000000000000000000 ) ) ;
#20704 = CARTESIAN_POINT ( 'NONE',  ( 50.20000000000000284, 142.6655632788954620, -8.961492836873480528 ) ) ;
#20705 = CARTESIAN_POINT ( 'NONE',  ( -2.426778023690076225, 199.3768101843759553, 58.89886208192144323 ) ) ;
#20706 = CARTESIAN_POINT ( 'NONE',  ( 67.50000000000000000, 155.0000000000000000, -6.938893903907228378E-15 ) ) ;
#20707 = CARTESIAN_POINT ( 'NONE',  ( 52.12499999726881583, 155.0000000000000000, 15.58253174999999402 ) ) ;
#20708 = CARTESIAN_POINT ( 'NONE',  ( 10.00000000000000711, 206.9523078486586201, 2.001137918078565558 ) ) ;
#20709 = DIRECTION ( 'NONE',  ( 0.000000000000000000, 0.000000000000000000, 1.000000000000000000 ) ) ;
#20710 = AXIS2_PLACEMENT_3D ( 'NONE', #9174, #4219, #24840 ) ;
#20711 = CARTESIAN_POINT ( 'NONE',  ( 59.62499999726881583, 171.3844434931184253, -7.942151717890134290E-15 ) ) ;
#20712 = CARTESIAN_POINT ( 'NONE',  ( 72.17499999726881299, 164.1591823560292198, 12.60653300113718167 ) ) ;
#20713 = CARTESIAN_POINT ( 'NONE',  ( -9.680171189290831535, 214.0920067884431148, 69.80113791807856671 ) ) ;
#20714 = FACE_OUTER_BOUND ( 'NONE', #8931, .T. ) ;
#20715 = CARTESIAN_POINT ( 'NONE',  ( -0.05014649552807705357, 194.3824533091408000, 14.75113791807856600 ) ) ;
#20716 = CARTESIAN_POINT ( 'NONE',  ( 3.044812012440130555, 197.4746971517856764, 86.60113791807857808 ) ) ;
#20717 = CARTESIAN_POINT ( 'NONE',  ( -9.736236675708031640, 214.0148392665760753, 53.79886208192143471 ) ) ;
#20718 = CARTESIAN_POINT ( 'NONE',  ( -8.062137200540822946, 201.0835637161416400, 59.19886208192144039 ) ) ;
#20719 = VECTOR ( 'NONE', #21459, 1000.000000000000000 ) ;
#20720 = CARTESIAN_POINT ( 'NONE',  ( -7.375838497908182134, 217.2372850707499765, 99.95113791807860082 ) ) ;
#20721 = FACE_OUTER_BOUND ( 'NONE', #13517, .T. ) ;
#20722 = CARTESIAN_POINT ( 'NONE',  ( 6.220909254589536808, 215.4770327129947702, 16.55113791807857027 ) ) ;
#20723 = CARTESIAN_POINT ( 'NONE',  ( -10.01549611932659722, 210.2015048109875011, 83.64886208192143613 ) ) ;
#20724 = EDGE_CURVE ( 'NONE', #6902, #11329, #776, .T. ) ;
#20725 = APPLICATION_CONTEXT ( 'automotive_design' ) ;
#20726 = ORIENTED_EDGE ( 'NONE', *, *, #6628, .F. ) ;
#20727 = CARTESIAN_POINT ( 'NONE',  ( 11.98450388067341876, 210.9467285061363953, 78.84886208192143897 ) ) ;
#20728 = CARTESIAN_POINT ( 'NONE',  ( 0.3999999999999975797, 0.000000000000000000, 0.000000000000000000 ) ) ;
#20729 = ORIENTED_EDGE ( 'NONE', *, *, #18464, .T. ) ;
#20730 = CARTESIAN_POINT ( 'NONE',  ( 80.17499999726881299, 164.1591823560292198, 12.60653300113718167 ) ) ;
#20731 = CARTESIAN_POINT ( 'NONE',  ( 6.444103211790928043, 211.7408657792734061, 51.69886208192144039 ) ) ;
#20732 = ORIENTED_EDGE ( 'NONE', *, *, #22599, .T. ) ;
#20733 = CARTESIAN_POINT ( 'NONE',  ( 73.62499999726883004, 171.3844434931184253, -7.942151717890134290E-15 ) ) ;
#20734 = FACE_OUTER_BOUND ( 'NONE', #10062, .T. ) ;
#20735 = DIRECTION ( 'NONE',  ( -1.000000000000000000, 0.000000000000000000, -0.000000000000000000 ) ) ;
#20736 = CIRCLE ( 'NONE', #7145, 2.149999999999999023 ) ;
#20737 = CARTESIAN_POINT ( 'NONE',  ( 61.82499999726881157, 168.2552932293087906, 9.630534252274372875 ) ) ;
#20738 = CARTESIAN_POINT ( 'NONE',  ( -7.500000000000346390, -3.105855721450154316, -7.659356991636309786 ) ) ;
#20739 = CARTESIAN_POINT ( 'NONE',  ( 10.01549611932659545, 203.7984951890123853, 55.14886208192143613 ) ) ;
#20740 = ORIENTED_EDGE ( 'NONE', *, *, #20920, .T. ) ;
#20741 = CYLINDRICAL_SURFACE ( 'NONE', #18372, 19.99999999999998934 ) ;
#20742 = CARTESIAN_POINT ( 'NONE',  ( 127.5000000000000000, 152.8500000000011028, 106.0000000000000426 ) ) ;
#20743 = CARTESIAN_POINT ( 'NONE',  ( -2.517493886309087880, 214.5937144450984135, 36.09886208192144608 ) ) ;
#20744 = CARTESIAN_POINT ( 'NONE',  ( -10.00000000000000711, 207.0476921513413515, 69.50113791807856956 ) ) ;
#20745 = CARTESIAN_POINT ( 'NONE',  ( 45.48867513459483547, 167.7597621252805880, 9.270509831248428867 ) ) ;
#20746 = CARTESIAN_POINT ( 'NONE',  ( -10.01549611932653860, 203.7984951890123284, 57.35113791807856387 ) ) ;
#20747 = CARTESIAN_POINT ( 'NONE',  ( -3.044812012440131443, 216.5253028482142952, 31.10113791807856742 ) ) ;
#20748 = CARTESIAN_POINT ( 'NONE',  ( -4.984841277089726574, 200.2242689037092305, 12.05113791807856849 ) ) ;
#20749 = CARTESIAN_POINT ( 'NONE',  ( -58.50000000000002132, 209.9999999999999716, 0.000000000000000000 ) ) ;
#20750 = CARTESIAN_POINT ( 'NONE',  ( -64.96121601855533356, -1.809269760319447418, 19.53878398144468775 ) ) ;
#20751 = CARTESIAN_POINT ( 'NONE',  ( 41.32499999726881157, 164.1591823560292198, -12.60653300113719766 ) ) ;
#20752 = CARTESIAN_POINT ( 'NONE',  ( 12.01549611932652972, 210.8513442034534933, 40.85113791807856387 ) ) ;
#20753 = FACE_BOUND ( 'NONE', #28856, .T. ) ;
#20754 = CARTESIAN_POINT ( 'NONE',  ( 10.01549611932653860, 210.2015048109876716, 82.85113791807854966 ) ) ;
#20755 = CARTESIAN_POINT ( 'NONE',  ( -10.01549611932653860, 203.7984951890123000, 54.35113791807856387 ) ) ;
#20756 = DIRECTION ( 'NONE',  ( 0.000000000000000000, 0.000000000000000000, -1.000000000000000000 ) ) ;
#20757 = CARTESIAN_POINT ( 'NONE',  ( -12.00000000000000711, 206.9523078486584780, 23.49886208192144110 ) ) ;
#20758 = CARTESIAN_POINT ( 'NONE',  ( 6.220909254589680693, 198.5229672870052582, 28.44886208192143684 ) ) ;
#20759 = AXIS2_PLACEMENT_3D ( 'NONE', #28514, #4999, #31237 ) ;
#20760 = CARTESIAN_POINT ( 'NONE',  ( 78.69999999453762030, 167.3344367211045096, 8.961492836873468093 ) ) ;
#20761 = CARTESIAN_POINT ( 'NONE',  ( -12.01549611932652972, 203.1486557965464499, 72.35113791807857808 ) ) ;
#20762 = CARTESIAN_POINT ( 'NONE',  ( 8.000000000000008882, 206.9523078486586485, 86.00113791807856956 ) ) ;
#20763 = CARTESIAN_POINT ( 'NONE',  ( -10.00000000000000711, 206.9523078486584495, 44.49886208192143755 ) ) ;
#20764 = ADVANCED_FACE ( 'NONE', ( #32492 ), #16989, .F. ) ;
#20765 = CARTESIAN_POINT ( 'NONE',  ( 63.78867513459482552, 155.0000000000000000, 15.00000000000001243 ) ) ;
#20766 = ORIENTED_EDGE ( 'NONE', *, *, #14716, .F. ) ;
#20767 = CARTESIAN_POINT ( 'NONE',  ( -3.753561863808878130, 218.3979405102790281, 48.09886208192143897 ) ) ;
#20768 = ORIENTED_EDGE ( 'NONE', *, *, #28307, .T. ) ;
#20769 = ORIENTED_EDGE ( 'NONE', *, *, #4731, .F. ) ;
#20770 = CARTESIAN_POINT ( 'NONE',  ( -52.50000000000002132, -95.00000000000000000, -20.00000000000000000 ) ) ;
#20771 = EDGE_CURVE ( 'NONE', #4891, #16641, #24163, .T. ) ;
#20772 = CARTESIAN_POINT ( 'NONE',  ( -7.894787914004607998, -1.230850257101226302E-13, -7.591390474663425536 ) ) ;
#20773 = ORIENTED_EDGE ( 'NONE', *, *, #19952, .F. ) ;
#20774 = CARTESIAN_POINT ( 'NONE',  ( -0.05014649552807731031, 198.5883022060938572, 41.75113791807856956 ) ) ;
#20775 = CARTESIAN_POINT ( 'NONE',  ( 82.01132485994281751, 167.7597621252805880, -9.270509831248443078 ) ) ;
#20776 = CARTESIAN_POINT ( 'NONE',  ( 9.984503880673420539, 210.2968891136705167, 18.84886208192143542 ) ) ;
#20777 = CARTESIAN_POINT ( 'NONE',  ( 61.77499999726881441, 169.8198683612136222, -4.815267126137197984 ) ) ;
#20778 = ORIENTED_EDGE ( 'NONE', *, *, #19447, .T. ) ;
#20779 = CARTESIAN_POINT ( 'NONE',  ( -125.0000000000000000, -95.00000000000000000, 20.00000000000001776 ) ) ;
#20780 = CARTESIAN_POINT ( 'NONE',  ( 32.50000000000000000, 155.0000000000000000, -6.938893903907228378E-15 ) ) ;
#20781 = CARTESIAN_POINT ( 'NONE',  ( 4.984841277089891776, 200.2242689037093726, 4.448862081921435063 ) ) ;
#20782 = B_SPLINE_CURVE_WITH_KNOTS ( 'NONE', 3,
 ( #18944, #32058, #883, #3779, #16548 ),
 .UNSPECIFIED., .F., .F.,
 ( 4, 1, 4 ),
 ( 0.000000000000000000, 0.003752776749732567897, 0.007505553499465135794 ),
 .UNSPECIFIED. ) ;
#20783 = CARTESIAN_POINT ( 'NONE',  ( 6.139770520408368348, 198.4640165459539674, 44.45113791807855819 ) ) ;
#20784 = DIRECTION ( 'NONE',  ( -1.000000000000000000, 0.000000000000000000, 0.000000000000000000 ) ) ;
#20785 = ADVANCED_FACE ( 'NONE', ( #1658 ), #18197, .T. ) ;
#20786 = CARTESIAN_POINT ( 'NONE',  ( -6.139770520408369237, 215.5359834540460042, 27.95113791807856174 ) ) ;
#20787 = CARTESIAN_POINT ( 'NONE',  ( -8.062137200540822946, 201.0835637161416400, 104.1988620819214475 ) ) ;
#20788 = CARTESIAN_POINT ( 'NONE',  ( 7.984503880673422316, 209.6470497212048372, 96.84886208192143897 ) ) ;
#20789 = VECTOR ( 'NONE', #16799, 1000.000000000000000 ) ;
#20790 = CARTESIAN_POINT ( 'NONE',  ( 35.12499999726881583, 155.0000000000000000, -15.58253175000000823 ) ) ;
#20791 = CARTESIAN_POINT ( 'NONE',  ( -58.16962743627800592, 194.9217985566782829, 2.500000000000000000 ) ) ;
#20792 = DIRECTION ( 'NONE',  ( -1.000000000000000000, 0.000000000000000000, -0.000000000000000000 ) ) ;
#20793 = CARTESIAN_POINT ( 'NONE',  ( -7.375838497908182134, 217.2372850707499765, 12.95113791807856707 ) ) ;
#20794 = CARTESIAN_POINT ( 'NONE',  ( 64.18867513459483121, 140.7341522555726669, 4.635254915624211769 ) ) ;
#20795 = CARTESIAN_POINT ( 'NONE',  ( 54.37499999726881583, 155.0000000000000000, 15.58253174999999402 ) ) ;
#20796 = EDGE_CURVE ( 'NONE', #20089, #2726, #2005, .T. ) ;
#20797 = CARTESIAN_POINT ( 'NONE',  ( -3.044812012440131443, 216.5253028482142952, 52.10113791807857808 ) ) ;
#20798 = DIRECTION ( 'NONE',  ( 0.000000000000000000, 0.000000000000000000, -1.000000000000000000 ) ) ;
#20799 = CARTESIAN_POINT ( 'NONE',  ( 42.51132485994281751, 163.8167787843871110, 12.13525491562421621 ) ) ;
#20800 = CARTESIAN_POINT ( 'NONE',  ( 4.000000000000001776, 0.000000000000000000, -2.200000000000001066 ) ) ;
#20801 = CARTESIAN_POINT ( 'NONE',  ( 55.49999999453763166, 139.7537977485451393, -4.138211985947621020E-15 ) ) ;
#20802 = EDGE_LOOP ( 'NONE', ( #17547, #9743, #32609, #21640 ) ) ;
#20803 = CARTESIAN_POINT ( 'NONE',  ( 9.680171189290831535, 199.9079932115568852, 35.30113791807856671 ) ) ;
#20804 = CARTESIAN_POINT ( 'NONE',  ( -47.49999999999998579, 155.0000000000000000, -6.938893903907228378E-15 ) ) ;
#20805 = CARTESIAN_POINT ( 'NONE',  ( -9.984503880673420539, 203.7031108863293980, 8.348862081921435419 ) ) ;
#20806 = DIRECTION ( 'NONE',  ( 1.000000000000000000, 0.000000000000000000, 0.000000000000000000 ) ) ;
#20807 = ORIENTED_EDGE ( 'NONE', *, *, #32365, .T. ) ;
#20808 = AXIS2_PLACEMENT_3D ( 'NONE', #11949, #32892, #9727 ) ;
#20809 = CARTESIAN_POINT ( 'NONE',  ( -8.118202686958039038, 201.1607312380087080, 9.201137918078565292 ) ) ;
#20810 = CARTESIAN_POINT ( 'NONE',  ( -9.984503880673473830, 210.2968891136704315, 69.65113791807854682 ) ) ;
#20811 = ORIENTED_EDGE ( 'NONE', *, *, #19498, .F. ) ;
#20812 = CARTESIAN_POINT ( 'NONE',  ( -6.500168698208244500, 211.6636982574061676, 32.79886208192143471 ) ) ;
#20813 = CARTESIAN_POINT ( 'NONE',  ( 44.51132485994280330, 163.8167787843871110, 12.13525491562421621 ) ) ;
#20814 = ORIENTED_EDGE ( 'NONE', *, *, #20647, .F. ) ;
#20815 = AXIS2_PLACEMENT_3D ( 'NONE', #16040, #13484, #21815 ) ;
#20816 = CARTESIAN_POINT ( 'NONE',  ( 6.500168698208129925, 211.6636982574063381, 16.70113791807856529 ) ) ;
#20817 = EDGE_CURVE ( 'NONE', #32748, #19344, #3418, .T. ) ;
#20818 = EDGE_CURVE ( 'NONE', #355, #25250, #1794, .T. ) ;
#20819 = CARTESIAN_POINT ( 'NONE',  ( -7.456977232089471386, 217.1783343296987709, 98.94886208192143329 ) ) ;
#20820 = CARTESIAN_POINT ( 'NONE',  ( 41.87499999726880873, 171.3844434931184253, -7.942151717890134290E-15 ) ) ;
#20821 = EDGE_LOOP ( 'NONE', ( #25767, #2602 ) ) ;
#20822 = CARTESIAN_POINT ( 'NONE',  ( 51.72499999726881725, 169.8198683612136222, 4.815267126137181997 ) ) ;
#20823 = CARTESIAN_POINT ( 'NONE',  ( 115.4999999999999858, 246.7986928011511907, 52.99999999999882760 ) ) ;
#20824 = CARTESIAN_POINT ( 'NONE',  ( 6.220909254589536808, 215.4770327129947702, 7.551137918078564049 ) ) ;
#20825 = CARTESIAN_POINT ( 'NONE',  ( -9.984503880673420539, 203.7031108863293980, 80.34886208192143897 ) ) ;
#20826 = CARTESIAN_POINT ( 'NONE',  ( 51.17499999726880588, 145.8408176439707802, -12.60653300113719588 ) ) ;
#20827 = CARTESIAN_POINT ( 'NONE',  ( -67.50001199999998391, 146.4804385394329529, -14.75313718340010460 ) ) ;
#20828 = CARTESIAN_POINT ( 'NONE',  ( 0.05014649552810505201, 217.5146222423826714, 13.25113791807856778 ) ) ;
#20829 = DIRECTION ( 'NONE',  ( 0.000000000000000000, 0.000000000000000000, 1.000000000000000000 ) ) ;
#20830 = EDGE_CURVE ( 'NONE', #22913, #11543, #22440, .T. ) ;
#20831 = AXIS2_PLACEMENT_3D ( 'NONE', #12798, #2241, #20798 ) ;
#20832 = CARTESIAN_POINT ( 'NONE',  ( 65.60000000000000853, 150.2886644046228639, 14.49999999999999645 ) ) ;
#20833 = CARTESIAN_POINT ( 'NONE',  ( -9.898309971686792608, 228.3698647632124334, 103.4854814124440452 ) ) ;
#20834 = FACE_OUTER_BOUND ( 'NONE', #16985, .T. ) ;
#20835 = CARTESIAN_POINT ( 'NONE',  ( 6.139770520408368348, 198.4640165459539674, 86.45113791807854398 ) ) ;
#20836 = CARTESIAN_POINT ( 'NONE',  ( 57.28867513459483263, 170.7719333635740497, -7.904646289410545231E-15 ) ) ;
#20837 = CARTESIAN_POINT ( 'NONE',  ( 27.50000000000000000, 6.731471899275977222, -0.4522261538067141595 ) ) ;
#20838 = EDGE_CURVE ( 'NONE', #18599, #1916, #26812, .T. ) ;
#20839 = CARTESIAN_POINT ( 'NONE',  ( -12.01549611932659722, 210.8513442034533227, 95.64886208192143613 ) ) ;
#20840 = CARTESIAN_POINT ( 'NONE',  ( 68.62499999726880162, 138.6155565068815463, -3.929120461958505118E-15 ) ) ;
#20841 = ORIENTED_EDGE ( 'NONE', *, *, #3709, .F. ) ;
#20842 = CARTESIAN_POINT ( 'NONE',  ( 84.71132485994282035, 155.0000000000000000, 15.00000000000001243 ) ) ;
#20843 = VECTOR ( 'NONE', #12169, 1000.000000000000000 ) ;
#20844 = CARTESIAN_POINT ( 'NONE',  ( 37.89999999453763024, 150.2886644046228639, -14.50000000000000888 ) ) ;
#20845 = CARTESIAN_POINT ( 'NONE',  ( 9.736236675707914401, 214.0148392665762458, 97.70113791807858661 ) ) ;
#20846 = B_SPLINE_CURVE_WITH_KNOTS ( 'NONE', 3,
 ( #24165, #21769, #23995, #31994 ),
 .UNSPECIFIED., .F., .F.,
 ( 4, 4 ),
 ( 2.380739282308437107E-07, 0.002044882221487503288 ),
 .UNSPECIFIED. ) ;
#20847 = VECTOR ( 'NONE', #4166, 1000.000000000000227 ) ;
#20848 = FACE_OUTER_BOUND ( 'NONE', #13267, .T. ) ;
#20849 = AXIS2_PLACEMENT_3D ( 'NONE', #8135, #18519, #5558 ) ;
#20850 = ORIENTED_EDGE ( 'NONE', *, *, #7878, .F. ) ;
#20851 = CARTESIAN_POINT ( 'NONE',  ( -6.220909254589682469, 215.4770327129947134, 83.94886208192144750 ) ) ;
#20852 = CARTESIAN_POINT ( 'NONE',  ( -7.456977232089471386, 217.1783343296987709, 23.94886208192143684 ) ) ;
#20853 = CARTESIAN_POINT ( 'NONE',  ( 32.50000000000000000, 155.0000000000000000, -15.00000000000002487 ) ) ;
#20854 = CARTESIAN_POINT ( 'NONE',  ( -9.984503880673473830, 210.2968891136704315, 45.65113791807855392 ) ) ;
#20855 = B_SPLINE_CURVE_WITH_KNOTS ( 'NONE', 3,
 ( #8033, #21295, #18417, #31689, #3399, #13794, #24188, #21627, #32020, #27077 ),
 .UNSPECIFIED., .F., .F.,
 ( 4, 2, 2, 2, 4 ),
 ( 0.01606529487141860474, 0.01806591702017404724, 0.02006653916892948974, 0.02406778346644037475, 0.03207027206146215170 ),
 .UNSPECIFIED. ) ;
#20856 = ORIENTED_EDGE ( 'NONE', *, *, #25399, .T. ) ;
#20857 = CARTESIAN_POINT ( 'NONE',  ( 0.05014649552828262524, 198.5883022060938572, 4.748862081921434886 ) ) ;
#20858 = EDGE_CURVE ( 'NONE', #23868, #17881, #26356, .T. ) ;
#20859 = AXIS2_PLACEMENT_3D ( 'NONE', #25699, #7486, #2201 ) ;
#20860 = ORIENTED_EDGE ( 'NONE', *, *, #978, .F. ) ;
#20861 = CARTESIAN_POINT ( 'NONE',  ( -8.015496119326597224, 209.5516654185217362, 86.64886208192143613 ) ) ;
#20862 = ORIENTED_EDGE ( 'NONE', *, *, #19594, .F. ) ;
#20863 = EDGE_CURVE ( 'NONE', #6342, #27806, #1980, .T. ) ;
#20864 = CARTESIAN_POINT ( 'NONE',  ( 8.000000000000008882, 206.9523078486586485, 29.00113791807856956 ) ) ;
#20865 = CARTESIAN_POINT ( 'NONE',  ( 56.01132485994281041, 167.7597621252805880, -9.270509831248443078 ) ) ;
#20866 = EDGE_LOOP ( 'NONE', ( #4454, #3756, #12628, #27686, #27539 ) ) ;
#20867 = CARTESIAN_POINT ( 'NONE',  ( -0.2791032213812780771, 8.821394357840562250, -7.929128246061909024 ) ) ;
#20868 = CIRCLE ( 'NONE', #24653, 24.99999999999999289 ) ;
#20869 = CIRCLE ( 'NONE', #17070, 17.00000000000000355 ) ;
#20870 = CARTESIAN_POINT ( 'NONE',  ( 85.22499999726882436, 160.0630714827496206, -15.58253175000000823 ) ) ;
#20871 = LINE ( 'NONE', #18153, #19216 ) ;
#20872 = CARTESIAN_POINT ( 'NONE',  ( -0.05014649552807731031, 198.5883022060938572, 86.75113791807856956 ) ) ;
#20873 = CARTESIAN_POINT ( 'NONE',  ( 1.211595439868046853, -7.960739084487661543, -0.4504974108212073114 ) ) ;
#20874 = CONICAL_SURFACE ( 'NONE', #26839, 32.00000000000002842, 0.1047197551196464710 ) ;
#20875 = CARTESIAN_POINT ( 'NONE',  ( 52.50000000000002132, 0.000000000000000000, 0.000000000000000000 ) ) ;
#20876 = CARTESIAN_POINT ( 'NONE',  ( 46.30000000000000426, 146.4771138417591203, -11.73074641843674470 ) ) ;
#20877 = CARTESIAN_POINT ( 'NONE',  ( -2.426778023690076225, 199.3768101843759553, 61.89886208192143613 ) ) ;
#20878 = CARTESIAN_POINT ( 'NONE',  ( 84.71132485994282035, 155.0000000000000000, 15.00000000000001243 ) ) ;
#20879 = CARTESIAN_POINT ( 'NONE',  ( 52.02499999726880020, 160.0630714827496206, 15.58253174999999402 ) ) ;
#20880 = MECHANICAL_DESIGN_GEOMETRIC_PRESENTATION_REPRESENTATION (  '', ( #7833 ), #32298 ) ;
#20881 = CARTESIAN_POINT ( 'NONE',  ( -8.118202686958039038, 201.1607312380087080, 3.201137918078566180 ) ) ;
#20882 = CARTESIAN_POINT ( 'NONE',  ( 100.4058500716420781, 155.0000000000000000, 12.99999999999998401 ) ) ;
#20883 = CARTESIAN_POINT ( 'NONE',  ( 57.52499999726881441, 169.8198683612136222, -4.815267126137197984 ) ) ;
#20884 = CARTESIAN_POINT ( 'NONE',  ( 73.27499999726882152, 149.9369285172503510, -15.58253175000000823 ) ) ;
#20885 = CARTESIAN_POINT ( 'NONE',  ( -7.375838497908182134, 217.2372850707499765, 69.95113791807858661 ) ) ;
#20886 = CARTESIAN_POINT ( 'NONE',  ( 45.91132485994280898, 163.8167787843871110, -12.13525491562423397 ) ) ;
#20887 = CARTESIAN_POINT ( 'NONE',  ( -3.662846001190052991, 218.4274158808045740, 13.10113791807856742 ) ) ;
#20888 = CARTESIAN_POINT ( 'NONE',  ( -3.044812012440131443, 216.5253028482142952, 85.10113791807857808 ) ) ;
#20889 = CYLINDRICAL_SURFACE ( 'NONE', #18488, 97.99999999999997158 ) ;
#20890 = CARTESIAN_POINT ( 'NONE',  ( -3.753561863808878130, 218.3979405102790281, 54.09886208192143897 ) ) ;
#20891 = CARTESIAN_POINT ( 'NONE',  ( 6.220909254589680693, 198.5229672870052582, 61.44886208192142618 ) ) ;
#20892 = AXIS2_PLACEMENT_3D ( 'NONE', #22667, #25225, #1890 ) ;
#20893 = CARTESIAN_POINT ( 'NONE',  ( 12.01549611932652972, 210.8513442034534933, 100.8511379180785781 ) ) ;
#20894 = CARTESIAN_POINT ( 'NONE',  ( -67.50001199999998391, 171.4562830276601346, -4.407803664655100206 ) ) ;
#20895 = CARTESIAN_POINT ( 'NONE',  ( -8.062137200540920645, 212.9164362838581894, 9.801137918078566713 ) ) ;
#20896 = AXIS2_PLACEMENT_3D ( 'NONE', #33391, #2215, #18224 ) ;
#20897 = CARTESIAN_POINT ( 'NONE',  ( 8.118202686958138514, 201.1607312380088501, 79.29886208192144181 ) ) ;
#20898 = EDGE_LOOP ( 'NONE', ( #14760, #12187, #11499, #12559 ) ) ;
#20899 = CARTESIAN_POINT ( 'NONE',  ( 3.753561863808876797, 195.6020594897209719, 76.59886208192142476 ) ) ;
#20900 = DIRECTION ( 'NONE',  ( 0.000000000000000000, 0.000000000000000000, 1.000000000000000000 ) ) ;
#20901 = VERTEX_POINT ( 'NONE', #28241 ) ;
#20902 = CARTESIAN_POINT ( 'NONE',  ( -2.352990130084580066E-16, 8.660254037844390851, -7.422398894150034288 ) ) ;
#20903 = CARTESIAN_POINT ( 'NONE',  ( -8.000000000000008882, 206.9523078486584780, 65.49886208192144466 ) ) ;
#20904 = VERTEX_POINT ( 'NONE', #20571 ) ;
#20905 = CARTESIAN_POINT ( 'NONE',  ( 69.72499999726881015, 169.8198683612136222, 4.815267126137181997 ) ) ;
#20906 = DIRECTION ( 'NONE',  ( 0.000000000000000000, 0.000000000000000000, 1.000000000000000000 ) ) ;
#20907 = CARTESIAN_POINT ( 'NONE',  ( -56.51026148866456111, 194.9712507328865740, 1.522362431316129916 ) ) ;
#20908 = UNCERTAINTY_MEASURE_WITH_UNIT (LENGTH_MEASURE( 1.000000000000000082E-05 ), #19935, 'distance_accuracy_value', 'NONE');
#20909 = CARTESIAN_POINT ( 'NONE',  ( 64.02499999726880731, 160.0630714827496206, 15.58253174999999402 ) ) ;
#20910 = LINE ( 'NONE', #20407, #23259 ) ;
#20911 = CARTESIAN_POINT ( 'NONE',  ( -0.05014649552828403384, 217.5146222423826714, 54.24886208192142334 ) ) ;
#20912 = VERTEX_POINT ( 'NONE', #28741 ) ;
#20913 = CARTESIAN_POINT ( 'NONE',  ( 22.99387487948479603, 18.47874495404627382, -16.90910675883083414 ) ) ;
#20914 = VECTOR ( 'NONE', #13785, 1000.000000000000000 ) ;
#20915 = CARTESIAN_POINT ( 'NONE',  ( 0.000000000000000000, 0.000000000000000000, 3.099999999999998757 ) ) ;
#20916 = CARTESIAN_POINT ( 'NONE',  ( 0.05014649552828262524, 198.5883022060938572, 34.74886208192143755 ) ) ;
#20917 = AXIS2_PLACEMENT_3D ( 'NONE', #18881, #29274, #19217 ) ;
#20918 = CARTESIAN_POINT ( 'NONE',  ( -10.00000000000000711, 207.0476921513413515, 72.50113791807858377 ) ) ;
#20919 = DIRECTION ( 'NONE',  ( 0.8660254037844359321, -0.5000000000000046629, 0.000000000000000000 ) ) ;
#20920 = EDGE_CURVE ( 'NONE', #1453, #13595, #32820, .T. ) ;
#20921 = CARTESIAN_POINT ( 'NONE',  ( -6.139770520408369237, 215.5359834540460042, 60.95113791807857950 ) ) ;
#20922 = CARTESIAN_POINT ( 'NONE',  ( 9.984503880673470277, 203.7031108863295401, 26.15113791807856813 ) ) ;
#20923 = CARTESIAN_POINT ( 'NONE',  ( -7.984503880673488041, 209.6470497212046098, 18.65113791807856458 ) ) ;
#20924 = CARTESIAN_POINT ( 'NONE',  ( -1.650000000000000133, 2.020667218593133001E-16, -2.899999999999999911 ) ) ;
#20925 = PLANE ( 'NONE',  #32305 ) ;
#20926 = CARTESIAN_POINT ( 'NONE',  ( 35.52499999726880731, 169.8198683612136222, -4.815267126137197984 ) ) ;
#20927 = CARTESIAN_POINT ( 'NONE',  ( -3.753561863808691168, 195.6020594897209435, 41.90113791807856813 ) ) ;
#20928 = DIRECTION ( 'NONE',  ( 1.000000000000000000, 0.000000000000000000, 0.000000000000000000 ) ) ;
#20929 = CARTESIAN_POINT ( 'NONE',  ( -3.044812012440131443, 216.5253028482142952, 82.10113791807857808 ) ) ;
#20930 = CARTESIAN_POINT ( 'NONE',  ( 3.135527875058820690, 216.4958274776887492, 55.40113791807857524 ) ) ;
#20931 =( GEOMETRIC_REPRESENTATION_CONTEXT ( 3 ) GLOBAL_UNCERTAINTY_ASSIGNED_CONTEXT ( ( #26095 ) ) GLOBAL_UNIT_ASSIGNED_CONTEXT ( ( #20578, #17850, #28414 ) ) REPRESENTATION_CONTEXT ( 'NONE', 'WORKASPACE' ) );
#20932 = CARTESIAN_POINT ( 'NONE',  ( 11.98450388067341876, 210.9467285061363953, 21.84886208192143542 ) ) ;
#20933 = CARTESIAN_POINT ( 'NONE',  ( -0.05014649552828402690, 217.5146222423826714, 33.24886208192141623 ) ) ;
#20934 = CARTESIAN_POINT ( 'NONE',  ( 80.19999999453763451, 163.5228861582408797, -11.73074641843674470 ) ) ;
#20935 = CARTESIAN_POINT ( 'NONE',  ( -12.00000000000000711, 207.0476921513413515, 63.50113791807856956 ) ) ;
#20936 = CARTESIAN_POINT ( 'NONE',  ( -4.984841277089726574, 200.2242689037092305, 84.05113791807858092 ) ) ;
#20937 = CARTESIAN_POINT ( 'NONE',  ( 10.00000000000000711, 207.0476921513415220, 51.99886208192143755 ) ) ;
#20938 = CARTESIAN_POINT ( 'NONE',  ( 115.4999999999999858, 182.4348187808683690, 102.3881375866409513 ) ) ;
#20939 = ORIENTED_EDGE ( 'NONE', *, *, #28938, .T. ) ;
#20940 = CARTESIAN_POINT ( 'NONE',  ( 0.05014649552828288198, 194.3824533091408000, 55.74886208192143755 ) ) ;
#20941 = ORIENTED_EDGE ( 'NONE', *, *, #28526, .T. ) ;
#20942 = VERTEX_POINT ( 'NONE', #13232 ) ;
#20943 = LINE ( 'NONE', #7503, #32559 ) ;
#20944 = DIRECTION ( 'NONE',  ( -0.000000000000000000, -0.000000000000000000, 1.000000000000000000 ) ) ;
#20945 = CARTESIAN_POINT ( 'NONE',  ( 2.517493886308900919, 214.5937144450984420, 37.40113791807856813 ) ) ;
#20946 =( NAMED_UNIT ( * ) SI_UNIT ( $, .STERADIAN. ) SOLID_ANGLE_UNIT ( ) );
#20947 = CARTESIAN_POINT ( 'NONE',  ( 10.00000000000000711, 207.0476921513415220, 18.99886208192143755 ) ) ;
#20948 = CARTESIAN_POINT ( 'NONE',  ( 64.17499999726879878, 164.1591823560292198, 12.60653300113718167 ) ) ;
#20949 = ORIENTED_EDGE ( 'NONE', *, *, #6664, .T. ) ;
#20950 = FACE_OUTER_BOUND ( 'NONE', #28289, .T. ) ;
#20951 =( LENGTH_UNIT ( ) NAMED_UNIT ( * ) SI_UNIT ( .MILLI., .METRE. ) );
#20952 = CARTESIAN_POINT ( 'NONE',  ( -10.12668159690567649, 1.256356190803088863E-15, -9.999999999999998224 ) ) ;
#20953 = CARTESIAN_POINT ( 'NONE',  ( 6.444103211790928043, 211.7408657792734061, 6.698862081921435063 ) ) ;
#20954 = CARTESIAN_POINT ( 'NONE',  ( 3.044812012440130555, 197.4746971517856764, 38.60113791807857098 ) ) ;
#20955 = PRODUCT_DEFINITION_SHAPE ( 'NONE', 'NONE',  #33702 ) ;
#20956 = EDGE_CURVE ( 'NONE', #20358, #23420, #29015, .T. ) ;
#20957 = CARTESIAN_POINT ( 'NONE',  ( -8.062137200540920645, 212.9164362838581894, 24.80113791807857027 ) ) ;
#20958 = CARTESIAN_POINT ( 'NONE',  ( -9.984503880673420539, 203.7031108863293980, 101.3488620819214248 ) ) ;
#20959 = APPLICATION_PROTOCOL_DEFINITION ( 'draft international standard', 'automotive_design', 1998, #25297 ) ;
#20960 = CARTESIAN_POINT ( 'NONE',  ( -2.426778023690076225, 199.3768101843759553, 91.89886208192143613 ) ) ;
#20961 = CARTESIAN_POINT ( 'NONE',  ( 83.60000000000000853, 150.2886644046228639, 14.49999999999999645 ) ) ;
#20962 = LINE ( 'NONE', #10420, #4461 ) ;
#20963 = CARTESIAN_POINT ( 'NONE',  ( 9.736236675707914401, 214.0148392665762458, 10.70113791807856529 ) ) ;
#20964 = ADVANCED_FACE ( 'NONE', ( #32757 ), #10024, .T. ) ;
#20965 = CARTESIAN_POINT ( 'NONE',  ( 56.37499999726880873, 155.0000000000000000, 15.58253174999999402 ) ) ;
#20966 = CARTESIAN_POINT ( 'NONE',  ( -10.01549611932653860, 203.7984951890123284, 57.35113791807856387 ) ) ;
#20967 = CARTESIAN_POINT ( 'NONE',  ( -9.984503880673475606, 210.2968891136704315, 30.65113791807856813 ) ) ;
#20968 = CYLINDRICAL_SURFACE ( 'NONE', #21906, 2.149999999999985256 ) ;
#20969 = ADVANCED_FACE ( 'NONE', ( #7296 ), #10684, .T. ) ;
#20970 = LINE ( 'NONE', #2914, #3230 ) ;
#20971 = CARTESIAN_POINT ( 'NONE',  ( -10.01549611932659545, 210.2015048109875011, 2.648862081921434353 ) ) ;
#20972 = CARTESIAN_POINT ( 'NONE',  ( 59.79999999453762882, 146.4771138417591203, -11.73074641843674470 ) ) ;
#20973 = VERTEX_POINT ( 'NONE', #5066 ) ;
#20974 = CARTESIAN_POINT ( 'NONE',  ( -12.01549611932652972, 203.1486557965464499, 42.35113791807857098 ) ) ;
#20975 = CARTESIAN_POINT ( 'NONE',  ( -8.542937654374687995, 1.046208125374536008E-15, -6.800000000000000711 ) ) ;
#20976 = CARTESIAN_POINT ( 'NONE',  ( -3.044812012439970683, 197.4746971517856196, 22.89886208192143613 ) ) ;
#20977 = CARTESIAN_POINT ( 'NONE',  ( 44.71132485994280614, 155.0000000000000000, 15.00000000000001243 ) ) ;
#20978 = ORIENTED_EDGE ( 'NONE', *, *, #29706, .F. ) ;
#20979 = CARTESIAN_POINT ( 'NONE',  ( 8.118202686958039038, 212.8392687619912635, 70.70113791807857240 ) ) ;
#20980 = ORIENTED_EDGE ( 'NONE', *, *, #6811, .T. ) ;
#20981 = DIRECTION ( 'NONE',  ( 1.000000000000000000, -0.000000000000000000, -0.000000000000000000 ) ) ;
#20982 = DIRECTION ( 'NONE',  ( -1.000000000000000000, 0.000000000000000000, 0.000000000000000000 ) ) ;
#20983 = ORIENTED_EDGE ( 'NONE', *, *, #16988, .F. ) ;
#20984 = CARTESIAN_POINT ( 'NONE',  ( -6.500168698208129925, 202.3363017425936050, 15.20113791807857062 ) ) ;
#20985 = EDGE_CURVE ( 'NONE', #22562, #3872, #15460, .T. ) ;
#20986 = CARTESIAN_POINT ( 'NONE',  ( -7.375838497908014268, 196.7627149292498530, 95.04886208192144181 ) ) ;
#20987 = CARTESIAN_POINT ( 'NONE',  ( 44.57499999726881157, 145.8408176439707802, 12.60653300113718345 ) ) ;
#20988 = VERTEX_POINT ( 'NONE', #25853 ) ;
#20989 = CARTESIAN_POINT ( 'NONE',  ( 53.22499999726879594, 160.0630714827496206, -15.58253175000000823 ) ) ;
#20990 = DIRECTION ( 'NONE',  ( 1.000000000000000000, 0.000000000000000000, 0.000000000000000000 ) ) ;
#20991 = CARTESIAN_POINT ( 'NONE',  ( -8.062137200540920645, 212.9164362838581894, 12.80113791807856671 ) ) ;
#20992 = CARTESIAN_POINT ( 'NONE',  ( 9.984503880673420539, 210.2968891136705167, 78.84886208192139634 ) ) ;
#20993 = CARTESIAN_POINT ( 'NONE',  ( 52.67499999726880588, 141.7447067706911810, 9.630534252274376428 ) ) ;
#20994 = CARTESIAN_POINT ( 'NONE',  ( 100.3007760113082156, 155.0000000000000000, 0.000000000000000000 ) ) ;
#20995 = CARTESIAN_POINT ( 'NONE',  ( 10.01549611932653860, 210.2015048109876716, 10.85113791807856387 ) ) ;
#20996 = CARTESIAN_POINT ( 'NONE',  ( 44.78867513459481842, 155.0000000000000000, -15.00000000000002487 ) ) ;
#20997 = EDGE_CURVE ( 'NONE', #19344, #32748, #7794, .T. ) ;
#20998 = CARTESIAN_POINT ( 'NONE',  ( 67.90000000000000568, 141.2096805137202580, 4.480746418436733158 ) ) ;
#20999 = CARTESIAN_POINT ( 'NONE',  ( 3.044812012440130555, 197.4746971517856764, 98.60113791807857808 ) ) ;
#21000 = LINE ( 'NONE', #31398, #33287 ) ;
#21001 = CARTESIAN_POINT ( 'NONE',  ( 8.118202686958039038, 212.8392687619912635, 82.70113791807857240 ) ) ;
#21002 = CARTESIAN_POINT ( 'NONE',  ( 86.28867513459482552, 139.2280666364260071, -4.041636747397287284E-15 ) ) ;
#21003 = CARTESIAN_POINT ( 'NONE',  ( 37.07499999726881157, 141.7447067706911810, -9.630534252274385310 ) ) ;
#21004 = CARTESIAN_POINT ( 'NONE',  ( -12.00000000000000711, 206.9523078486584780, 92.49886208192144466 ) ) ;
#21005 = CARTESIAN_POINT ( 'NONE',  ( 69.12499999726881583, 155.0000000000000000, -15.58253175000000823 ) ) ;
#21006 = ORIENTED_EDGE ( 'NONE', *, *, #14919, .F. ) ;
#21007 = DIRECTION ( 'NONE',  ( 1.000000000000000000, 0.000000000000000000, 0.000000000000000000 ) ) ;
#21008 = CARTESIAN_POINT ( 'NONE',  ( 40.49999999453763166, 170.2462022514548323, -7.872454543227099337E-15 ) ) ;
#21009 = ADVANCED_BREP_SHAPE_REPRESENTATION ( '', ( #1296, #2404 ), #11135 ) ;
#21010 = CARTESIAN_POINT ( 'NONE',  ( -11.98450388067348804, 210.9467285061362247, 96.65113791807858945 ) ) ;
#21011 = ADVANCED_FACE ( 'NONE', ( #15617 ), #2371, .T. ) ;
#21012 = CARTESIAN_POINT ( 'NONE',  ( 0.000000000000000000, 0.000000000000000000, -2.899999999999999911 ) ) ;
#21013 = ORIENTED_EDGE ( 'NONE', *, *, #5854, .F. ) ;
#21014 = CARTESIAN_POINT ( 'NONE',  ( -3.135527875058982783, 216.4958274776886924, 99.09886208192143897 ) ) ;
#21015 = CARTESIAN_POINT ( 'NONE',  ( -9.680171189290716072, 199.9079932115567146, 26.19886208192144039 ) ) ;
#21016 = CARTESIAN_POINT ( 'NONE',  ( 8.118202686958039038, 212.8392687619912635, 46.70113791807857240 ) ) ;
#21017 = EDGE_LOOP ( 'NONE', ( #12989, #2438, #27104, #16094 ) ) ;
#21018 = EDGE_CURVE ( 'NONE', #8859, #31412, #19642, .T. ) ;
#21019 = CARTESIAN_POINT ( 'NONE',  ( -6.500168698208244500, 211.6636982574061676, 8.798862081921434708 ) ) ;
#21020 = AXIS2_PLACEMENT_3D ( 'NONE', #17105, #12662, #30734 ) ;
#21021 = CARTESIAN_POINT ( 'NONE',  ( 54.75000000000000000, 7.990820364436479461E-15, -20.00000000000000355 ) ) ;
#21022 = ORIENTED_EDGE ( 'NONE', *, *, #20997, .T. ) ;
#21023 = CARTESIAN_POINT ( 'NONE',  ( 4.903702542908435547, 213.8346818373419751, 93.54886208192142760 ) ) ;
#21024 = CARTESIAN_POINT ( 'NONE',  ( -6.444103211791042618, 211.7408657792732356, 30.80113791807857027 ) ) ;
#21025 = CARTESIAN_POINT ( 'NONE',  ( 6.500000000000000888, 0.000000000000000000, 0.000000000000000000 ) ) ;
#21027 = ORIENTED_EDGE ( 'NONE', *, *, #4303, .T. ) ;
#21026 = CIRCLE ( 'NONE', #6329, 2.149999999999994138 ) ;
#21028 = DIRECTION ( 'NONE',  ( -0.000000000000000000, -0.000000000000000000, -1.000000000000000000 ) ) ;
#21029 = CARTESIAN_POINT ( 'NONE',  ( 34.87499999726880873, 138.6155565068815463, -3.929120461958505118E-15 ) ) ;
#21030 = CARTESIAN_POINT ( 'NONE',  ( 103.3032345859876102, 155.0000000000000000, 31.00000000000000000 ) ) ;
#21031 = CARTESIAN_POINT ( 'NONE',  ( 2.426778023690261410, 199.3768101843759837, 92.60113791807857808 ) ) ;
#21032 = DIRECTION ( 'NONE',  ( 0.000000000000000000, 0.000000000000000000, 1.000000000000000000 ) ) ;
#21033 = CARTESIAN_POINT ( 'NONE',  ( 46.20000000000000995, 142.6655632788954620, -8.961492836873480528 ) ) ;
#21034 = CARTESIAN_POINT ( 'NONE',  ( 8.000000000000008882, 207.0476921513415220, 66.99886208192144466 ) ) ;
#21035 = DIRECTION ( 'NONE',  ( 1.000000000000000000, -0.000000000000000000, -0.000000000000000000 ) ) ;
#21036 = AXIS2_PLACEMENT_3D ( 'NONE', #8896, #15442, #29016 ) ;
#21037 = CARTESIAN_POINT ( 'NONE',  ( 51.82499999726881157, 168.2552932293087906, 9.630534252274372875 ) ) ;
#21038 = VECTOR ( 'NONE', #7340, 1000.000000000000000 ) ;
#21039 = CARTESIAN_POINT ( 'NONE',  ( -6.139770520408368348, 215.5359834540460042, 0.9511379180785657361 ) ) ;
#21040 = CARTESIAN_POINT ( 'NONE',  ( 4.200000000000001954, 0.000000000000000000, 0.000000000000000000 ) ) ;
#21041 = CARTESIAN_POINT ( 'NONE',  ( 63.52499999726880731, 169.8198683612136222, -4.815267126137197984 ) ) ;
#21042 = CARTESIAN_POINT ( 'NONE',  ( 66.97499999726881015, 140.1801316387863778, -4.815267126137194431 ) ) ;
#21043 = CARTESIAN_POINT ( 'NONE',  ( -12.01549611932652972, 203.1486557965464499, 63.35113791807857098 ) ) ;
#21044 = CARTESIAN_POINT ( 'NONE',  ( -6.663120783604270514, -3.846954578056921648, -6.460786012259833733 ) ) ;
#21045 = ADVANCED_FACE ( 'NONE', ( #26506 ), #27304, .T. ) ;
#21046 = ADVANCED_FACE ( 'NONE', ( #23790 ), #14520, .F. ) ;
#21047 = CARTESIAN_POINT ( 'NONE',  ( -8.062137200540920645, 212.9164362838581894, 90.80113791807858092 ) ) ;
#21048 = DIRECTION ( 'NONE',  ( -0.000000000000000000, -0.000000000000000000, -1.000000000000000000 ) ) ;
#21049 = CONICAL_SURFACE ( 'NONE', #19975, 3.999999999999999112, 0.9599310885968813656 ) ;
#21050 = CARTESIAN_POINT ( 'NONE',  ( -12.00000000000000711, 206.9523078486584780, 50.49886208192143044 ) ) ;
#21051 = CARTESIAN_POINT ( 'NONE',  ( 0.05014649552828275014, 196.4853777576173002, 55.74886208192143755 ) ) ;
#21052 = CARTESIAN_POINT ( 'NONE',  ( -9.736236675707914401, 199.9851607334237542, 96.20113791807858661 ) ) ;
#21053 = CARTESIAN_POINT ( 'NONE',  ( -67.50001199999999812, 167.8075758004701754, -11.23405475987242497 ) ) ;
#21054 = CARTESIAN_POINT ( 'NONE',  ( -0.05014649552810635652, 196.4853777576173002, 14.75113791807856245 ) ) ;
#21055 = ADVANCED_FACE ( 'NONE', ( #3965, #27472 ), #21067, .T. ) ;
#21056 = PRODUCT_DEFINITION ( 'UNKNOWN', '', #16436, #3959 ) ;
#21057 = EDGE_CURVE ( 'NONE', #24113, #6185, #11802, .T. ) ;
#21058 = CARTESIAN_POINT ( 'NONE',  ( -3.135527875058982783, 216.4958274776886924, 75.09886208192143897 ) ) ;
#21059 = ORIENTED_EDGE ( 'NONE', *, *, #2945, .F. ) ;
#21060 = CARTESIAN_POINT ( 'NONE',  ( 6.139770520408368348, 198.4640165459539674, 95.45113791807855819 ) ) ;
#21061 = ORIENTED_EDGE ( 'NONE', *, *, #27422, .F. ) ;
#21062 = CARTESIAN_POINT ( 'NONE',  ( -6.444103211790928043, 202.2591342207265939, 65.19886208192143329 ) ) ;
#21063 = VECTOR ( 'NONE', #6378, 1000.000000000000000 ) ;
#21064 = ORIENTED_EDGE ( 'NONE', *, *, #17084, .T. ) ;
#21065 = CARTESIAN_POINT ( 'NONE',  ( 80.32499999726880446, 145.8408176439707802, 12.60653300113718345 ) ) ;
#21066 = CARTESIAN_POINT ( 'NONE',  ( -4.336808689942017736E-16, 7.505553499465137612, -0.8000000000000003775 ) ) ;
#21067 = PLANE ( 'NONE',  #21924 ) ;
#21068 = CARTESIAN_POINT ( 'NONE',  ( 68.22499999726881015, 149.9369285172503510, 15.58253174999999580 ) ) ;
#21069 = CARTESIAN_POINT ( 'NONE',  ( -0.05014649552807731031, 198.5883022060938572, 56.75113791807857666 ) ) ;
#21070 = CARTESIAN_POINT ( 'NONE',  ( 6.220909254589681581, 198.5229672870052582, 55.44886208192141908 ) ) ;
#21071 = CONICAL_SURFACE ( 'NONE', #407, 7.500000000000001776, 0.8594454914424796144 ) ;
#21072 = FACE_OUTER_BOUND ( 'NONE', #32451, .T. ) ;
#21073 = CARTESIAN_POINT ( 'NONE',  ( 7.897850199329715437, -1.533397866934079312, -7.634054012537967893 ) ) ;
#21074 = CARTESIAN_POINT ( 'NONE',  ( -8.000000000000008882, 206.9523078486584780, 32.49886208192143044 ) ) ;
#21075 = CARTESIAN_POINT ( 'NONE',  ( 6.139770520408368348, 198.4640165459539674, 83.45113791807858661 ) ) ;
#21076 = FACE_BOUND ( 'NONE', #16490, .T. ) ;
#21077 = CARTESIAN_POINT ( 'NONE',  ( 9.984503880673470277, 203.7031108863295401, 59.15113791807858235 ) ) ;
#21078 = CARTESIAN_POINT ( 'NONE',  ( 10.00000000000000711, 206.9523078486586201, 29.00113791807856956 ) ) ;
#21079 = CARTESIAN_POINT ( 'NONE',  ( -8.000000000000008882, 207.0476921513413515, 15.50113791807856600 ) ) ;
#21080 = CARTESIAN_POINT ( 'NONE',  ( 108.1100194822685836, 155.0000000000000000, 0.000000000000000000 ) ) ;
#21081 = CARTESIAN_POINT ( 'NONE',  ( 94.70964751525852421, 155.0000000000000000, 0.000000000000000000 ) ) ;
#21082 = CARTESIAN_POINT ( 'NONE',  ( 45.22499999726881015, 160.0630714827496206, -15.58253175000000823 ) ) ;
#21083 = CARTESIAN_POINT ( 'NONE',  ( 3.753561863808689836, 218.3979405102790565, 34.40113791807856813 ) ) ;
#21084 = CARTESIAN_POINT ( 'NONE',  ( 7.500000000000000000, 1.572594658376109011, -7.069792055233639516 ) ) ;
#21085 = AXIS2_PLACEMENT_3D ( 'NONE', #25341, #6451, #9671 ) ;
#21086 = CARTESIAN_POINT ( 'NONE',  ( 3.135527875058820690, 216.4958274776887492, 88.40113791807857524 ) ) ;
#21087 = CARTESIAN_POINT ( 'NONE',  ( -9.984503880673475606, 210.2968891136704315, 60.65113791807856813 ) ) ;
#21088 = AXIS2_PLACEMENT_3D ( 'NONE', #27717, #20558, #6935 ) ;
#21089 = STYLED_ITEM ( 'NONE', ( #16288 ), #1296 ) ;
#21090 = CARTESIAN_POINT ( 'NONE',  ( -9.680171189290716072, 199.9079932115567146, 26.19886208192144039 ) ) ;
#21091 = CARTESIAN_POINT ( 'NONE',  ( -8.062137200540822946, 201.0835637161416400, 26.19886208192143684 ) ) ;
#21092 = CARTESIAN_POINT ( 'NONE',  ( 77.39999999453762314, 141.2096805137202580, 4.480746418436733158 ) ) ;
#21093 = CARTESIAN_POINT ( 'NONE',  ( 11.98450388067348271, 203.0532714938637753, 65.15113791807856103 ) ) ;
#21094 = CARTESIAN_POINT ( 'NONE',  ( -0.05014649552807731031, 198.5883022060938572, 92.75113791807858377 ) ) ;
#21095 = AXIS2_PLACEMENT_3D ( 'NONE', #22201, #11980, #14198 ) ;
#21096 = CARTESIAN_POINT ( 'NONE',  ( 3.135527875058981895, 197.5041725223112792, 49.59886208192143897 ) ) ;
#21097 = DIRECTION ( 'NONE',  ( 1.000000000000000000, 0.000000000000000000, 0.000000000000000000 ) ) ;
#21098 = AXIS2_PLACEMENT_3D ( 'NONE', #2753, #25, #345 ) ;
#21099 = EDGE_LOOP ( 'NONE', ( #12010, #33558, #25420, #12181 ) ) ;
#21100 = CARTESIAN_POINT ( 'NONE',  ( -9.680171189290716072, 199.9079932115567146, 53.19886208192144039 ) ) ;
#21101 = ORIENTED_EDGE ( 'NONE', *, *, #22599, .F. ) ;
#21102 = ORIENTED_EDGE ( 'NONE', *, *, #4602, .F. ) ;
#21103 = CARTESIAN_POINT ( 'NONE',  ( 87.18867513459483121, 169.2658477444273331, -4.635254915624224203 ) ) ;
#21104 = CARTESIAN_POINT ( 'NONE',  ( 78.00000000000001421, 4.052968581778165278E-16, -3.309499999999999886 ) ) ;
#21105 = CARTESIAN_POINT ( 'NONE',  ( -8.000000000000008882, 207.0476921513413515, 42.50113791807857666 ) ) ;
#21106 = CIRCLE ( 'NONE', #24366, 27.50000000000000355 ) ;
#21107 = CARTESIAN_POINT ( 'NONE',  ( -3.999999999999999112, 4.898587196589411843E-16, 3.469446951953614189E-15 ) ) ;
#21108 = AXIS2_PLACEMENT_3D ( 'NONE', #4345, #1781, #32957 ) ;
#21109 = CARTESIAN_POINT ( 'NONE',  ( 9.984503880673420539, 210.2968891136705167, 24.84886208192143897 ) ) ;
#21110 = CARTESIAN_POINT ( 'NONE',  ( 64.47499999726881015, 149.9369285172503510, 15.58253174999999580 ) ) ;
#21111 = ORIENTED_EDGE ( 'NONE', *, *, #28609, .T. ) ;
#21112 = CARTESIAN_POINT ( 'NONE',  ( 41.08867513459482979, 167.7597621252805880, -9.270509831248443078 ) ) ;
#21113 = SHAPE_REPRESENTATION_RELATIONSHIP ( 'NONE' , 'NONE' ,  #32415, #32336 ) ;
#21114 = CARTESIAN_POINT ( 'NONE',  ( 115.4999999999999858, 257.3881375866408803, -27.43481878086871717 ) ) ;
#21115 = CARTESIAN_POINT ( 'NONE',  ( -0.05014649552828365914, 215.4116977939061144, 3.248862081921435330 ) ) ;
#21116 = CARTESIAN_POINT ( 'NONE',  ( 8.118202686958039038, 212.8392687619912635, 49.70113791807857240 ) ) ;
#21117 =( LENGTH_UNIT ( ) NAMED_UNIT ( * ) SI_UNIT ( .MILLI., .METRE. ) );
#21118 = CARTESIAN_POINT ( 'NONE',  ( -10.01549611932653860, 203.7984951890123284, 27.35113791807856742 ) ) ;
#21119 = CARTESIAN_POINT ( 'NONE',  ( 86.27499999726880731, 160.0630714827496206, 15.58253174999999402 ) ) ;
#21120 = VECTOR ( 'NONE', #12242, 1000.000000000000000 ) ;
#21121 = ITEM_DEFINED_TRANSFORMATION ( 'NONE', 'NONE', #11556,  #2404 ) ;
#21122 = CARTESIAN_POINT ( 'NONE',  ( 4.903702542908435547, 213.8346818373419751, 93.54886208192142760 ) ) ;
#21123 = CARTESIAN_POINT ( 'NONE',  ( 37.62499999726880162, 171.3844434931184253, -7.942151717890132712E-15 ) ) ;
#21124 = CARTESIAN_POINT ( 'NONE',  ( 0.000000000000000000, 0.000000000000000000, -18.00000000000000000 ) ) ;
#21125 = CARTESIAN_POINT ( 'NONE',  ( -7.375838497908182134, 217.2372850707499765, 6.951137918078566180 ) ) ;
#21126 = CARTESIAN_POINT ( 'NONE',  ( 117.5000000000000000, 155.0000000000000000, -100.0000000000000000 ) ) ;
#21127 = CARTESIAN_POINT ( 'NONE',  ( 57.67499999726880588, 168.2552932293087906, -9.630534252274385310 ) ) ;
#21128 = CARTESIAN_POINT ( 'NONE',  ( 3.044812012440130555, 197.4746971517856764, 59.60113791807857808 ) ) ;
#21129 = CARTESIAN_POINT ( 'NONE',  ( -10.01549611932653860, 203.7984951890123000, 33.35113791807857098 ) ) ;
#21130 = CARTESIAN_POINT ( 'NONE',  ( -7.500000000000001776, 0.000000000000000000, 0.000000000000000000 ) ) ;
#21131 = DIRECTION ( 'NONE',  ( 1.000000000000000000, 0.000000000000000000, 0.000000000000000000 ) ) ;
#21132 = CARTESIAN_POINT ( 'NONE',  ( 63.49999999453763166, 139.7537977485451393, -4.138211985947621020E-15 ) ) ;
#21133 = EDGE_LOOP ( 'NONE', ( #33607, #12985, #18662, #29898, #4557, #5919, #3710, #7370 ) ) ;
#21134 = CARTESIAN_POINT ( 'NONE',  ( 7.456977232089302632, 217.1783343296989131, 34.55113791807856671 ) ) ;
#21135 = CARTESIAN_POINT ( 'NONE',  ( 36.88867513459483405, 159.8737954434939752, -14.99999999999974420 ) ) ;
#21136 = CARTESIAN_POINT ( 'NONE',  ( -8.118202686958138514, 212.8392687619910930, 23.79886208192143471 ) ) ;
#21137 = AXIS2_PLACEMENT_3D ( 'NONE', #5065, #20225, #13069 ) ;
#21138 = ORIENTED_EDGE ( 'NONE', *, *, #8713, .T. ) ;
#21139 = UNCERTAINTY_MEASURE_WITH_UNIT (LENGTH_MEASURE( 1.000000000000000082E-05 ), #12744, 'distance_accuracy_value', 'NONE');
#21140 = CARTESIAN_POINT ( 'NONE',  ( -3.135527875058821579, 197.5041725223112223, 68.90113791807857524 ) ) ;
#21141 = EDGE_LOOP ( 'NONE', ( #27339, #3652, #13337, #18873 ) ) ;
#21142 = ADVANCED_FACE ( 'NONE', ( #14364 ), #4128, .F. ) ;
#21143 = VECTOR ( 'NONE', #527, 1000.000000000000000 ) ;
#21144 = CARTESIAN_POINT ( 'NONE',  ( 4.000000000000000000, -3.518949890710769246, 3.686287386450715076E-15 ) ) ;
#21145 = CARTESIAN_POINT ( 'NONE',  ( 80.28867513459483973, 139.2280666364260071, -4.041636747397287284E-15 ) ) ;
#21146 = ORIENTED_EDGE ( 'NONE', *, *, #25531, .T. ) ;
#21147 = CARTESIAN_POINT ( 'NONE',  ( 7.984503880673485376, 204.3529502787953902, 11.15113791807856636 ) ) ;
#21148 = CARTESIAN_POINT ( 'NONE',  ( 12.00000000000000711, 207.0476921513415220, 96.99886208192143044 ) ) ;
#21149 = CARTESIAN_POINT ( 'NONE',  ( 40.67499999726880588, 141.7447067706911810, 9.630534252274376428 ) ) ;
#21150 = ORIENTED_EDGE ( 'NONE', *, *, #21202, .T. ) ;
#21151 = CARTESIAN_POINT ( 'NONE',  ( 53.92499999726881299, 164.1591823560292198, 12.60653300113718167 ) ) ;
#21152 = DIRECTION ( 'NONE',  ( 1.000000000000000000, -0.000000000000000000, -0.000000000000000000 ) ) ;
#21153 = CARTESIAN_POINT ( 'NONE',  ( 8.118202686958039038, 212.8392687619912635, 10.70113791807856529 ) ) ;
#21154 = VECTOR ( 'NONE', #3308, 1000.000000000000000 ) ;
#21155 = CARTESIAN_POINT ( 'NONE',  ( -10.00000000000000711, 206.9523078486584495, 80.49886208192143044 ) ) ;
#21156 = CARTESIAN_POINT ( 'NONE',  ( 54.47499999726880304, 149.9369285172503510, 15.58253174999999580 ) ) ;
#21157 = CARTESIAN_POINT ( 'NONE',  ( 105.9028607166213192, 155.0000000000000000, 32.10452846326769816 ) ) ;
#21158 = CARTESIAN_POINT ( 'NONE',  ( 10.00000000000000711, 206.9523078486586201, 23.00113791807856600 ) ) ;
#21159 = LINE ( 'NONE', #13001, #26286 ) ;
#21160 = CARTESIAN_POINT ( 'NONE',  ( 75.80000000000001137, 142.6655632788954620, 8.961492836873471646 ) ) ;
#21161 = CARTESIAN_POINT ( 'NONE',  ( 10.01549611932653860, 210.2015048109876716, 97.85113791807857808 ) ) ;
#21162 = CARTESIAN_POINT ( 'NONE',  ( 27.50000000000000355, 15.87713240271474291, -2.456200930618646971 ) ) ;
#21163 = CARTESIAN_POINT ( 'NONE',  ( 6.139770520408368348, 198.4640165459539674, 89.45113791807857240 ) ) ;
#21164 = LINE ( 'NONE', #15722, #14016 ) ;
#21165 = CARTESIAN_POINT ( 'NONE',  ( 40.57499999726881157, 145.8408176439707802, 12.60653300113718345 ) ) ;
#21166 = CARTESIAN_POINT ( 'NONE',  ( -3.753561863808878130, 218.3979405102790281, 96.09886208192143897 ) ) ;
#21167 = APPLICATION_CONTEXT ( 'automotive_design' ) ;
#21168 = AXIS2_PLACEMENT_3D ( 'NONE', #20469, #7018, #17402 ) ;
#21169 = CARTESIAN_POINT ( 'NONE',  ( 70.82499999726883289, 141.7447067706911810, -9.630534252274385310 ) ) ;
#21170 = ORIENTED_EDGE ( 'NONE', *, *, #12098, .F. ) ;
#21171 = DIRECTION ( 'NONE',  ( 0.000000000000000000, -0.000000000000000000, 1.000000000000000000 ) ) ;
#21172 = CARTESIAN_POINT ( 'NONE',  ( 40.69999999453762030, 167.3344367211045096, 8.961492836873468093 ) ) ;
#21173 = EDGE_CURVE ( 'NONE', #29217, #19467, #31187, .T. ) ;
#21174 = CARTESIAN_POINT ( 'NONE',  ( 39.71132485994280614, 155.0000000000000000, -15.00000000000002487 ) ) ;
#21175 = CARTESIAN_POINT ( 'NONE',  ( 0.2791032213812723040, -8.821394357840571132, -7.929128246061910801 ) ) ;
#21176 = EDGE_LOOP ( 'NONE', ( #2169, #5548, #33392, #5349 ) ) ;
#21177 = CARTESIAN_POINT ( 'NONE',  ( -8.118202686958138514, 212.8392687619910930, 95.79886208192144181 ) ) ;
#21178 = CARTESIAN_POINT ( 'NONE',  ( 7.456977232089471386, 196.8216656703012006, 28.44886208192142973 ) ) ;
#21179 = CARTESIAN_POINT ( 'NONE',  ( 6.500000000000000888, -2.534234941938116936, -0.3584823952106179212 ) ) ;
#21180 = TOROIDAL_SURFACE ( 'NONE', #8136, 6.500000000000000888, 1.500000000000000000 ) ;
#21181 = CARTESIAN_POINT ( 'NONE',  ( -6.220909254589537696, 198.5229672870051161, 42.05113791807857382 ) ) ;
#21182 = EDGE_LOOP ( 'NONE', ( #30617, #2803, #24705, #10325, #24243 ) ) ;
#21183 = CARTESIAN_POINT ( 'NONE',  ( -2.426778023690076225, 199.3768101843759553, 4.898862081921435241 ) ) ;
#21184 = EDGE_CURVE ( 'NONE', #11757, #32368, #8866, .T. ) ;
#21185 = CARTESIAN_POINT ( 'NONE',  ( 74.51132485994280330, 163.8167787843871110, 12.13525491562421621 ) ) ;
#21186 = ORIENTED_EDGE ( 'NONE', *, *, #11249, .T. ) ;
#21187 = CARTESIAN_POINT ( 'NONE',  ( -6.444103211790928043, 202.2591342207265939, 89.19886208192144750 ) ) ;
#21188 = CARTESIAN_POINT ( 'NONE',  ( -7.984503880673488041, 209.6470497212046098, 30.65113791807856458 ) ) ;
#21189 = CARTESIAN_POINT ( 'NONE',  ( 95.59906517536109050, 155.0000000000000000, 0.000000000000000000 ) ) ;
#21190 = ORIENTED_EDGE ( 'NONE', *, *, #27285, .F. ) ;
#21191 = CARTESIAN_POINT ( 'NONE',  ( 0.6169862416622686752, 8.783631307150953305, -7.913704048099833521 ) ) ;
#21192 = ADVANCED_FACE ( 'NONE', ( #31468 ), #27142, .T. ) ;
#21193 =( BOUNDED_CURVE ( )  B_SPLINE_CURVE ( 2, ( #16246, #257, #2648, #20865, #31425, #31586, #15908, #16075, #24077, #5359, #13031 ),
 .UNSPECIFIED., .F., .F. ) 
 B_SPLINE_CURVE_WITH_KNOTS ( ( 3, 2, 2, 2, 2, 3 ),
 ( 0.3928571428571428492, 0.3964285714285714080, 0.4000000000000000222, 0.4035714285714285809, 0.4071428571428571397, 0.4107142857142856984 ),
 .UNSPECIFIED. ) 
 CURVE ( )  GEOMETRIC_REPRESENTATION_ITEM ( )  RATIONAL_B_SPLINE_CURVE ( ( 1.000000000000000000, 0.9510565162951534202, 1.000000000000000000, 0.9510565162951534202, 1.000000000000000000, 0.9510565162951534202, 1.000000000000000000, 0.9510565162951534202, 1.000000000000000000, 0.9510565162951534202, 1.000000000000000000 ) ) 
 REPRESENTATION_ITEM ( '' )  );
#21194 = CARTESIAN_POINT ( 'NONE',  ( 86.12499999726881583, 155.0000000000000000, 15.58253174999999402 ) ) ;
#21195 = DIRECTION ( 'NONE',  ( 1.000000000000000000, 0.000000000000000000, 0.000000000000000000 ) ) ;
#21196 = CARTESIAN_POINT ( 'NONE',  ( -2.517493886308901807, 199.4062855549015012, 89.90113791807857524 ) ) ;
#21197 = DIRECTION ( 'NONE',  ( -1.000000000000000000, 7.939222169223397018E-18, 6.869460786763197348E-19 ) ) ;
#21198 = CARTESIAN_POINT ( 'NONE',  ( 47.99999999999999289, 139.7537977485451393, -4.138211985947621020E-15 ) ) ;
#21199 = CARTESIAN_POINT ( 'NONE',  ( -6.500168698208244500, 211.6636982574061676, 77.79886208192142760 ) ) ;
#21200 = VECTOR ( 'NONE', #12077, 1000.000000000000000 ) ;
#21201 = CARTESIAN_POINT ( 'NONE',  ( 84.21132485994282035, 170.7719333635740497, -7.904646289410545231E-15 ) ) ;
#21202 = EDGE_CURVE ( 'NONE', #8400, #30073, #7258, .T. ) ;
#21203 = CARTESIAN_POINT ( 'NONE',  ( 51.42499999726879878, 168.2552932293087906, -9.630534252274385310 ) ) ;
#21205 = ORIENTED_EDGE ( 'NONE', *, *, #3537, .F. ) ;
#21204 = CARTESIAN_POINT ( 'NONE',  ( -6.139770520408368348, 215.5359834540460042, 6.951137918078566180 ) ) ;
#21206 = DIRECTION ( 'NONE',  ( 1.000000000000000000, -0.000000000000000000, -0.000000000000000000 ) ) ;
#21207 = CARTESIAN_POINT ( 'NONE',  ( 66.82499999726881867, 141.7447067706911810, -9.630534252274387086 ) ) ;
#21208 = CARTESIAN_POINT ( 'NONE',  ( 76.07499999726879025, 168.2552932293087906, 9.630534252274372875 ) ) ;
#21209 = CARTESIAN_POINT ( 'NONE',  ( -9.680171189290831535, 214.0920067884431148, 81.80113791807858092 ) ) ;
#21210 = CARTESIAN_POINT ( 'NONE',  ( -6.500000000000000000, -3.752776749732572803, -6.064240316920399998 ) ) ;
#21211 = EDGE_CURVE ( 'NONE', #11454, #5515, #30653, .T. ) ;
#21212 = CARTESIAN_POINT ( 'NONE',  ( 10.00000000000000711, 206.9523078486586201, 98.00113791807856956 ) ) ;
#21213 = DIRECTION ( 'NONE',  ( 0.000000000000000000, 1.000000000000000000, 0.000000000000000000 ) ) ;
#21214 = EDGE_LOOP ( 'NONE', ( #20980, #26707, #18762, #5024 ) ) ;
#21215 = CARTESIAN_POINT ( 'NONE',  ( 3.753561863808876797, 195.6020594897209719, 52.59886208192143897 ) ) ;
#21216 = CARTESIAN_POINT ( 'NONE',  ( -10.01549611932659545, 210.2015048109875011, 71.64886208192143613 ) ) ;
#21217 = CARTESIAN_POINT ( 'NONE',  ( -3.753561863808691168, 195.6020594897209435, 101.9011379180785895 ) ) ;
#21218 = LINE ( 'NONE', #442, #22436 ) ;
#21219 = CARTESIAN_POINT ( 'NONE',  ( 6.220909254589536808, 215.4770327129947702, 13.55113791807856849 ) ) ;
#21220 = CARTESIAN_POINT ( 'NONE',  ( 9.984503880673420539, 210.2968891136705167, 81.84886208192143897 ) ) ;
#21221 = ORIENTED_EDGE ( 'NONE', *, *, #9834, .F. ) ;
#21222 = CARTESIAN_POINT ( 'NONE',  ( -10.01549611932653860, 203.7984951890123284, 102.3511379180785781 ) ) ;
#21223 = EDGE_LOOP ( 'NONE', ( #4005, #18998 ) ) ;
#21224 = DIRECTION ( 'NONE',  ( 0.000000000000000000, 0.000000000000000000, -1.000000000000000000 ) ) ;
#21225 = CARTESIAN_POINT ( 'NONE',  ( -0.05014649552828365914, 215.4116977939061144, 60.24886208192144466 ) ) ;
#21226 = ORIENTED_EDGE ( 'NONE', *, *, #744, .F. ) ;
#21227 = PRODUCT_DEFINITION_SHAPE ( 'NONE', 'NONE',  #33720 ) ;
#21228 = CARTESIAN_POINT ( 'NONE',  ( 76.62499999726880162, 138.6155565068815747, -3.929120461958505118E-15 ) ) ;
#21229 = DIRECTION ( 'NONE',  ( -0.000000000000000000, -0.000000000000000000, -1.000000000000000000 ) ) ;
#21230 = CARTESIAN_POINT ( 'NONE',  ( 117.5000000000000000, 246.7986928011511907, 52.99999999999882760 ) ) ;
#21231 = UNCERTAINTY_MEASURE_WITH_UNIT (LENGTH_MEASURE( 1.000000000000000082E-05 ), #6018, 'distance_accuracy_value', 'NONE');
#21232 = CARTESIAN_POINT ( 'NONE',  ( 67.32499999726881867, 164.1591823560292198, -12.60653300113719766 ) ) ;
#21233 = CARTESIAN_POINT ( 'NONE',  ( 8.015496119326531499, 209.5516654185219636, 55.85113791807856387 ) ) ;
#21234 = EDGE_CURVE ( 'NONE', #19918, #16399, #15949, .T. ) ;
#21235 = EDGE_CURVE ( 'NONE', #10430, #7925, #19768, .T. ) ;
#21236 = CARTESIAN_POINT ( 'NONE',  ( -9.254041968259778983, 206.2987758111210894, 104.1628994045829870 ) ) ;
#21237 =( NAMED_UNIT ( * ) SI_UNIT ( $, .STERADIAN. ) SOLID_ANGLE_UNIT ( ) );
#21238 = CARTESIAN_POINT ( 'NONE',  ( -64.50000000000000000, 155.0000000000000000, 40.00000000000001421 ) ) ;
#21239 = CARTESIAN_POINT ( 'NONE',  ( -2.426778023690076225, 199.3768101843759553, 31.89886208192144323 ) ) ;
#21240 = CARTESIAN_POINT ( 'NONE',  ( -8.062137200540920645, 212.9164362838581894, 84.80113791807856671 ) ) ;
#21241 = CARTESIAN_POINT ( 'NONE',  ( 10.12668159690567649, 0.000000000000000000, -9.999999999999998224 ) ) ;
#21242 = ADVANCED_FACE ( 'NONE', ( #18682 ), #29543, .T. ) ;
#21243 = CARTESIAN_POINT ( 'NONE',  ( 3.044812012440130555, 197.4746971517856764, 68.60113791807857808 ) ) ;
#21244 = DIRECTION ( 'NONE',  ( 1.000000000000000000, 0.000000000000000000, 0.000000000000000000 ) ) ;
#21245 = CARTESIAN_POINT ( 'NONE',  ( 6.500168698208129925, 211.6636982574063381, 16.70113791807856529 ) ) ;
#21246 = CARTESIAN_POINT ( 'NONE',  ( 3.093157300003884558, 6.874418838041288282, 2.127746763502802452E-15 ) ) ;
#21247 = CARTESIAN_POINT ( 'NONE',  ( -3.499999999999999112, -1.355464348821715959, -0.1381584212714501159 ) ) ;
#21248 = CARTESIAN_POINT ( 'NONE',  ( 42.22499999726880304, 149.9369285172503510, 15.58253174999999580 ) ) ;
#21249 = CARTESIAN_POINT ( 'NONE',  ( 12.00000000000000711, 206.9523078486586485, 44.00113791807856956 ) ) ;
#21250 = CARTESIAN_POINT ( 'NONE',  ( 7.499999999998625100, 3.882635837268474166, -7.781684861371460649 ) ) ;
#21251 = ADVANCED_FACE ( 'NONE', ( #617 ), #25759, .T. ) ;
#21252 = CARTESIAN_POINT ( 'NONE',  ( -3.044812012440131443, 216.5253028482142952, 94.10113791807857808 ) ) ;
#21253 = CARTESIAN_POINT ( 'NONE',  ( -9.984503880673475606, 210.2968891136704315, 54.65113791807858235 ) ) ;
#21254 = CARTESIAN_POINT ( 'NONE',  ( 3.753561863808876797, 195.6020594897209719, 25.59886208192143897 ) ) ;
#21255 = CARTESIAN_POINT ( 'NONE',  ( -9.984503880673420539, 203.7031108863293980, 35.34886208192143187 ) ) ;
#21256 = CARTESIAN_POINT ( 'NONE',  ( 76.79999999453762882, 163.5228861582408797, 11.73074641843673049 ) ) ;
#21257 = CARTESIAN_POINT ( 'NONE',  ( -9.680171189290831535, 214.0920067884431148, 63.80113791807858092 ) ) ;
#21258 = CARTESIAN_POINT ( 'NONE',  ( 2.426778023690261410, 199.3768101843759837, 92.60113791807857808 ) ) ;
#21259 = CARTESIAN_POINT ( 'NONE',  ( -10.01549611932659722, 210.2015048109875011, 47.64886208192142192 ) ) ;
#21260 = DIRECTION ( 'NONE',  ( 1.000000000000000000, 0.000000000000000000, 0.000000000000000000 ) ) ;
#21261 = VECTOR ( 'NONE', #28633, 1000.000000000000000 ) ;
#21262 = VERTEX_POINT ( 'NONE', #6528 ) ;
#21263 = CARTESIAN_POINT ( 'NONE',  ( 9.680171189290716072, 214.0920067884432854, 51.69886208192144039 ) ) ;
#21264 = AXIS2_PLACEMENT_3D ( 'NONE', #16326, #13774, #16663 ) ;
#21265 = ORIENTED_EDGE ( 'NONE', *, *, #30492, .T. ) ;
#21266 = ORIENTED_EDGE ( 'NONE', *, *, #15216, .T. ) ;
#21267 = CARTESIAN_POINT ( 'NONE',  ( 76.57499999726881867, 145.8408176439707802, 12.60653300113718345 ) ) ;
#21268 = CARTESIAN_POINT ( 'NONE',  ( 87.08867513459483689, 167.7597621252805880, -9.270509831248443078 ) ) ;
#21269 = CARTESIAN_POINT ( 'NONE',  ( 59.78867513459481842, 155.0000000000000000, 15.00000000000001243 ) ) ;
#21270 = CARTESIAN_POINT ( 'NONE',  ( -0.05014649552807731031, 198.5883022060938572, 38.75113791807856956 ) ) ;
#21271 = DIRECTION ( 'NONE',  ( -0.1045284632676468234, 1.217938055844715641E-16, -0.9945218953682740670 ) ) ;
#21272 = CARTESIAN_POINT ( 'NONE',  ( 9.984503880673420539, 210.2968891136705167, 27.84886208192143187 ) ) ;
#21273 = CARTESIAN_POINT ( 'NONE',  ( 66.07499999726881867, 168.2552932293087906, 9.630534252274372875 ) ) ;
#21274 = ORIENTED_EDGE ( 'NONE', *, *, #12286, .F. ) ;
#21275 = CARTESIAN_POINT ( 'NONE',  ( 35.91132485994280898, 163.8167787843871110, -12.13525491562423397 ) ) ;
#21276 = UNCERTAINTY_MEASURE_WITH_UNIT (LENGTH_MEASURE( 1.000000000000000082E-05 ), #26679, 'distance_accuracy_value', 'NONE');
#21277 =( NAMED_UNIT ( * ) PLANE_ANGLE_UNIT ( ) SI_UNIT ( $, .RADIAN. ) );
#21278 = DIRECTION ( 'NONE',  ( 1.000000000000000000, 0.000000000000000000, 0.000000000000000000 ) ) ;
#21279 = CARTESIAN_POINT ( 'NONE',  ( -6.444103211790928043, 202.2591342207265939, 2.198862081921435063 ) ) ;
#21280 = CARTESIAN_POINT ( 'NONE',  ( -8.062137200540920645, 212.9164362838581894, 51.80113791807857382 ) ) ;
#21281 = CARTESIAN_POINT ( 'NONE',  ( 3.288228914120474133, -7.217643567644815406, -7.591235721156641247 ) ) ;
#21282 = CARTESIAN_POINT ( 'NONE',  ( -8.118202686958039038, 201.1607312380087080, 39.20113791807857240 ) ) ;
#21283 = CARTESIAN_POINT ( 'NONE',  ( 87.27499999726880731, 149.9369285172503510, -15.58253175000000823 ) ) ;
#21284 = SHAPE_DEFINITION_REPRESENTATION ( #10293, #13706 ) ;
#21285 = CARTESIAN_POINT ( 'NONE',  ( -6.500168698208244500, 211.6636982574061676, 95.79886208192144181 ) ) ;
#21286 = CARTESIAN_POINT ( 'NONE',  ( 40.22499999726880304, 149.9369285172503510, 15.58253174999999580 ) ) ;
#21287 = LINE ( 'NONE', #29456, #31773 ) ;
#21288 = CYLINDRICAL_SURFACE ( 'NONE', #31611, 15.00000000000001776 ) ;
#21289 = CARTESIAN_POINT ( 'NONE',  ( 3.753561863808689836, 218.3979405102790565, 10.40113791807856636 ) ) ;
#21290 = CARTESIAN_POINT ( 'NONE',  ( 0.000000000000000000, 0.000000000000000000, 0.000000000000000000 ) ) ;
#21291 = CARTESIAN_POINT ( 'NONE',  ( 57.57499999726881157, 164.1591823560292198, -12.60653300113719766 ) ) ;
#21292 = CARTESIAN_POINT ( 'NONE',  ( 10.01549611932653860, 210.2015048109876716, 52.85113791807854966 ) ) ;
#21293 = CARTESIAN_POINT ( 'NONE',  ( -9.984503880673475606, 210.2968891136704315, 27.65113791807856458 ) ) ;
#21294 = DIRECTION ( 'NONE',  ( -1.000000000000000000, 0.000000000000000000, 0.000000000000000000 ) ) ;
#21295 = CARTESIAN_POINT ( 'NONE',  ( -13.16654248868335664, 24.15255795529144933, -18.00000000000000711 ) ) ;
#21296 = CARTESIAN_POINT ( 'NONE',  ( 6.220909254589680693, 198.5229672870052582, 13.44886208192143329 ) ) ;
#21297 = CARTESIAN_POINT ( 'NONE',  ( 60.39999999453763024, 168.7903194862797420, -4.480746418436745593 ) ) ;
#21298 = VERTEX_POINT ( 'NONE', #6350 ) ;
#21299 = CARTESIAN_POINT ( 'NONE',  ( -9.736236675707914401, 199.9851607334237542, 39.20113791807857240 ) ) ;
#21300 = DIRECTION ( 'NONE',  ( -1.000000000000000000, 0.000000000000000000, -0.000000000000000000 ) ) ;
#21301 = CARTESIAN_POINT ( 'NONE',  ( -6.139770520408224463, 198.4640165459539389, 26.04886208192143471 ) ) ;
#21302 = CARTESIAN_POINT ( 'NONE',  ( 71.38867513459481984, 169.2658477444273331, 4.635254915624208216 ) ) ;
#21303 = ORIENTED_EDGE ( 'NONE', *, *, #23557, .T. ) ;
#21304 = CARTESIAN_POINT ( 'NONE',  ( 9.984503880673470277, 203.7031108863295401, 77.15113791807857524 ) ) ;
#21305 = ORIENTED_EDGE ( 'NONE', *, *, #22463, .T. ) ;
#21306 = DIRECTION ( 'NONE',  ( 1.000000000000000000, 0.000000000000000000, 0.000000000000000000 ) ) ;
#21307 = DIRECTION ( 'NONE',  ( 0.000000000000000000, 0.000000000000000000, 1.000000000000000000 ) ) ;
#21308 = VECTOR ( 'NONE', #16214, 1000.000000000000000 ) ;
#21309 = ORIENTED_EDGE ( 'NONE', *, *, #14591, .T. ) ;
#21310 = CARTESIAN_POINT ( 'NONE',  ( 2.426778023690261410, 199.3768101843759837, 14.60113791807856742 ) ) ;
#21311 = DIRECTION ( 'NONE',  ( 1.000000000000000000, 0.000000000000000000, 0.000000000000000000 ) ) ;
#21312 = CARTESIAN_POINT ( 'NONE',  ( 12.01549611932659367, 203.1486557965466773, 100.1488620819214646 ) ) ;
#21313 = CARTESIAN_POINT ( 'NONE',  ( 46.07499999726881157, 168.2552932293087906, 9.630534252274372875 ) ) ;
#21314 = ORIENTED_EDGE ( 'NONE', *, *, #5845, .F. ) ;
#21315 = CARTESIAN_POINT ( 'NONE',  ( 48.02499999726879309, 160.0630714827496206, 15.58253174999999402 ) ) ;
#21316 = LINE ( 'NONE', #26933, #29515 ) ;
#21317 = DIRECTION ( 'NONE',  ( -0.000000000000000000, -0.000000000000000000, 1.000000000000000000 ) ) ;
#21318 = CARTESIAN_POINT ( 'NONE',  ( -10.00000000000000711, 206.9523078486584495, 83.49886208192143044 ) ) ;
#21319 = CARTESIAN_POINT ( 'NONE',  ( 56.37499999726880873, 155.0000000000000000, 15.58253174999999402 ) ) ;
#21320 = CARTESIAN_POINT ( 'NONE',  ( -0.05014649552810635652, 196.4853777576173002, 20.75113791807855890 ) ) ;
#21321 = CARTESIAN_POINT ( 'NONE',  ( 32.50000000000000000, 155.0000000000000000, 15.00000000000001243 ) ) ;
#21322 = CARTESIAN_POINT ( 'NONE',  ( 73.20000000000001705, 167.3344367211045096, 8.961492836873468093 ) ) ;
#21323 = CARTESIAN_POINT ( 'NONE',  ( 4.000000000000000000, -1.759474945355381958, 3.047500000000001208 ) ) ;
#21324 = CARTESIAN_POINT ( 'NONE',  ( -63.49999999999884892, 215.0000000000003979, 0.000000000000000000 ) ) ;
#21325 = CARTESIAN_POINT ( 'NONE',  ( -10.00000000000000711, 207.0476921513413515, 87.50113791807858377 ) ) ;
#21326 = CARTESIAN_POINT ( 'NONE',  ( -10.00000000000019362, 205.9534653805592654, 104.4507591396482127 ) ) ;
#21327 = CARTESIAN_POINT ( 'NONE',  ( 41.27499999726880731, 149.9369285172503510, -15.58253175000000823 ) ) ;
#21328 = CARTESIAN_POINT ( 'NONE',  ( -7.456977232089471386, 217.1783343296987709, 98.94886208192143329 ) ) ;
#21329 = ADVANCED_FACE ( 'NONE', ( #16741 ), #16908, .F. ) ;
#21330 = CARTESIAN_POINT ( 'NONE',  ( 78.12499999726883004, 155.0000000000000000, 15.58253174999999402 ) ) ;
#21331 = VERTEX_POINT ( 'NONE', #9415 ) ;
#21332 = CARTESIAN_POINT ( 'NONE',  ( -4.927659837809095222, 206.3103720916592465, -5.504302862921502282 ) ) ;
#21333 = CARTESIAN_POINT ( 'NONE',  ( 43.49999999453763166, 139.7537977485451393, -4.138211985947621020E-15 ) ) ;
#21334 =( BOUNDED_SURFACE ( )  B_SPLINE_SURFACE ( 1, 2, ( 
 ( #2278, #28173, #5002, #30558, #30906, #25273, #15222, #4831, #12500, #15390, #12327, #33111, #22889, #9948, #7220, #20335, #29171, #13170, #10628, #31887, #23565, #2954, #24052, #13659, #721, #11125, #8070, #8397, #559, #11283, #26608, #7903, #16054, #21500, #5822, #29005, #8554, #21003, #18783, #18948, #388, #16217, #26443, #5332, #3436, #21667, #234, #5666, #18455, #18284, #13833, #15723, #3271, #2790, #29344, #5991, #26122, #28673, #10952, #16379, #31401, #26771, #28842, #5498, #13497, #15887, #31724, #26281, #13333, #24223, #23725, #10791, #21165, #31562, #886, #8229, #18618, #3108, #23891, #21327, #24736, #11617, #25066, #27612, #9391, #1558, #22337, #19282, #27283, #22006, #11778, #6157, #4106, #14498, #14672, #32556, #11954, #30010, #14169, #32221, #1390, #32389, #9230, #9053, #32724, #19787, #32061, #16552, #12120, #30182, #29849, #6326, #3605, #6839, #16719, #19445, #1720, #8886, #19620, #1062, #8723, #19113, #16886, #6672, #17225, #6508, #3940, #29674, #17059, #14340, #29503, #27121, #3782, #4281, #26946, #27452, #13999, #11451, #24396, #21830, #24562, #24897, #1219, #22168, #25740, #22677, #23016, #15181, #25908, #7529, #22511, #30696, #15350, #10088, #9908, #4962, #1898, #33414, #2411, #15009, #20465, #7359, #19950, #18077, #2581, #14836, #20290, #33064, #32898, #28473, #30349, #30865, #17398, #17915, #12796, #7012, #9558, #25574, #23187, #27784, #28306, #12285, #9734, #28127, #4448, #12622, #25235, #20122, #20636, #7181, #30516, #25398, #17565, #33581, #27958, #4627, #10260, #2070, #12458, #2239, #22850, #15517, #5129, #31035, #7694, #33242, #17738, #4788, #26237, #26406, #20795, #18743, #29129, #29297, #13454, #16172, #10914, #28806, #13129, #16014, #13293, #23847, #2908, #13618, #679, #12967, #31196, #26733, #24015, #10747, #20965, #18247, #3232, #31359, #23685, #5949, #23522, #522, #15684, #23363, #26, #31526, #21291, #21127, #10423, #5291, #28964, #8195, #346, #31684, #26086, #5622, #2754, #3065, #18580, #8355, #5777, #190, #26562, #11081, #21462, #31844, #10588, #8508, #18902, #16339, #8028, #18413, #7862, #28636, #5462, #15848, #6111, #27861, #8679, #32640, #20035, #9640, #30435, #7095, #3565, #4364, #30259, #7267, #22588, #3394, #12028, #17476, #25140, #24985, #4533, #16508, #14747, #14926, #30088, #1804, #22416, #846, #33158, #17650, #29460, #1636, #13955, #13789, #9821, #11234, #12201, #32015, #32974, #25314, #21621, #24184, #6921, #1978, #19071, #12369, #26907, #24346, #9473, #1471, #27702, #11866, #22253, #22765, #9303, #19695, #6753, #17141, #20202, #27527, #4188, #30602, #14584, #32806, #17312, #19861, #21042, #23607, #5375, #31282, #18324, #15262, #23269, #7611, #7774, #2156, #103, #10505, #10666, #28559, #7942, #25995, #10161, #28214, #31112, #28386, #5207, #17995, #28719, #15763, #28038, #12539, #8113, #26158, #25829, #2321, #33324, #2824, #12708, #5043, #31445, #4873, #15593, #30773, #4699, #15089, #12876, #2665, #2493, #25482, #20544, #17816, #13208, #22929, #25654, #13048, #23104, #9994, #20712, #15433, #20381, #271, #7435, #33492, #30946, #33664, #10340, #18165, #23438, #20884, #24257, #927, #1102, #18993, #21709, #16421, #595, #18657, #21536, #18818, #29383, #31766, #19151, #6202, #18495, #2989, #32265, #29548, #16261, #26483, #23766, #8763, #3152, #29212, #11495, #29047, #6029, #21208, #28880, #5536, #3311, #26817, #26647, #15926, #10833, #762, #13695, #8432, #3481, #31602, #11161, #16591, #24095, #5864, #16089, #13872, #31926, #21873, #5701, #13539, #26983, #3647, #11325, #431, #8269, #14042, #23933, #10991, #32100, #24438, #26324, #13369, #21370, #8597, #1603, #12333, #27662, #8933, #17111, #1767, #30228, #30053, #25106, #22047, #19832, #22559, #1433, #6883, #27495, #6374, #4496, #22730, #1270, #6720, #9097, #19323, #14887, #16765, #17273, #3819, #4329, #12167, #27163, #29712, #11994, #32944, #14211, #14713, #32430, #19493, #14547, #24608, #32769, #11663, #29893, #7060, #27325, #6547, #9605, #16930, #4150, #20000, #30399, #24946, #17442, #3990, #27826, #25280, #11829, #1944, #22380, #14387, #24777, #22215, #32604, #9442, #9269, #19663, #28678, #7227, #7740, #28004, #10307, #2630, #30564, #33118, #25794, #23407, #9783, #18125, #22895, #9955, #5007, #4670, #23232, #13176, #20167, #31246, #17781, #17617, #25618 ),
 ( #15730, #12669, #10129, #15054, #10470, #25449, #17963, #33288, #5339, #20509, #2124, #12840, #7400, #2285, #18289, #13015, #12507, #5172, #23065, #15229, #28181, #26127, #7577, #20342, #33628, #20683, #15396, #2795, #30741, #28353, #33457, #4839, #30912, #28523, #2459, #15558, #70, #31081, #25953, #20844, #7908, #26614, #8076, #6163, #23572, #393, #16224, #19119, #8235, #31892, #26952, #18623, #3113, #21505, #8728, #23730, #241, #5828, #15892, #24228, #3441, #5671, #3276, #13504, #13663, #21008, #29349, #21172, #23897, #10797, #29178, #18461, #24058, #3611, #10633, #21675, #29011, #31406, #16060, #13339, #891, #28848, #31567, #729, #26449, #5503, #11130, #564, #16557, #29509, #11288, #26777, #13839, #10957, #18789, #21333, #8560, #26287, #5997, #16384, #2960, #18955, #32068, #31730, #8402, #14176, #17066, #14347, #24902, #27290, #14677, #1725, #14004, #32228, #27789, #25071, #11785, #22012, #19287, #4288, #32395, #24742, #7019, #24569, #1565, #16724, #24403, #1068, #32564, #11958, #22173, #11456, #6333, #30016, #9235, #3947, #22342, #27127, #6679, #12125, #19625, #1396, #11626, #32729, #27457, #17403, #1227, #9059, #22518, #32905, #9398, #29679, #3788, #9563, #19452, #29856, #30188, #19795, #6844, #17232, #6514, #14504, #4112, #21835, #27617, #8891, #19957, #30354, #16893, #25580, #20644, #17571, #15356, #18083, #30701, #25745, #12627, #1905, #33, #7868, #30521, #2245, #4632, #4453, #10429, #12291, #12801, #33070, #2417, #7700, #22684, #14842, #30872, #28480, #25240, #23193, #27964, #9742, #28312, #18252, #20127, #2587, #22856, #7186, #7364, #15015, #15522, #25405, #2076, #4968, #12464, #33247, #7536, #17743, #31203, #20801, #25914, #5135, #12974, #9913, #33419, #28134, #17923, #20296, #10266, #31041, #4794, #33587, #23370, #15189, #23022, #10093, #20470, #28971, #5784, #8201, #29304, #16345, #28641, #13136, #8687, #5956, #26413, #2916, #198, #18910, #13300, #5631, #21630, #28811, #16180, #31367, #5297, #15688, #13462, #26569, #3074, #26091, #20972, #10921, #23853, #18586, #3238, #8035, #21297, #26739, #528, #16022, #26245, #13625, #31691, #32023, #5468, #23692, #3401, #13797, #24022, #10596, #18419, #24191, #15854, #354, #11088, #685, #21468, #31852, #10754, #29136, #8361, #2759, #8517, #23529, #18752, #853, #11245, #21132, #31531, #32187, #29978, #32686, #11578, #6635, #27247, #16515, #14638, #22471, #11418, #6471, #19247, #19079, #25035, #26914, #27415, #13961, #17021, #22305, #3572, #29467, #11744, #9353, #6119, #4075, #8847, #29642, #24699, #9194, #32862, #24356, #17190, #3743, #1023, #21968, #6289, #30146, #21795, #16683, #19584, #27080, #14132, #22131, #32356, #12080, #1687, #6803, #19749, #27575, #24527, #14297, #9021, #32521, #1182, #24860, #1523, #19410, #14463, #4241, #11919, #29812, #16854, #3901, #1356, #20430, #22816, #10218, #31002, #9524, #27751, #23323, #20600, #7325, #17530, #14800, #33542, #27918, #20253, #2544, #9696, #30823, #12250, #19911, #30311, #28089, #7490, #17701, #6978, #1861, #25536, #4752, #33207, #17874, #22638, #2204, #7658, #15143, #30658, #7146, #28269, #9871, #12928, #20088, #4590, #18042, #28435, #4924, #25193, #33026, #5092, #30483, #14976, #25702, #15311, #2375, #12764, #25363, #10053, #12586, #17365, #23154, #4415, #22979, #15487, #25878, #33379, #2035, #12422, #10881, #13588, #26204, #21256, #8161, #31157, #29261, #3359, #26048, #21092, #151, #9203, #5912, #7825, #8316, #28604, #31650, #3200, #18213, #10387, #26372, #23981, #20760, #18710, #23486, #10555, #5585, #5255, #13417, #15649, #5744, #16136, #16307, #484, #643, #29096, #15810, #20934, #3032, #312, #26529, #13257, #11040, #21423, #2718, #13095, #13749, #31809, #31494, #7992, #31326, #8474, #18378, #10711, #26696, #28770, #18863, #5425, #2871, #23653, #18543, #28926, #15980, #23812, #16469, #6427, #32314, #14087, #1318, #26869, #16808, #1480, #21918, #1143, #21753, #22091, #24481, #17148, #24304, #8804, #22261, #24817, #11706, #29425, #3526, #14424, #6074, #19201, #6589, #29935, #16972, #27368, #975, #24652, #27204, #27534, #9145, #24145, #8980, #4035, #32476, #11536, #11876, #13919, #19542, #32648, #16637, #9310, #19367, #21580, #19703, #4196, #11374, #29761, #32142, #811, #30096, #31975, #6763, #19036, #11201, #8645, #29600, #6250, #3860, #27033 ) ),
 .UNSPECIFIED., .F., .F., .T. ) 
 B_SPLINE_SURFACE_WITH_KNOTS ( ( 2, 2 ),
 ( 3, 2, 2, 2, 2, 2, 2, 2, 2, 2, 2, 2, 2, 2, 2, 2, 2, 2, 2, 2, 2, 2, 2, 2, 2, 2, 2, 2, 2, 2, 2, 2, 2, 2, 2, 2, 2, 2, 2, 2, 2, 2, 2, 2, 2, 2, 2, 2, 2, 2, 2, 2, 2, 2, 2, 2, 2, 2, 2, 2, 2, 2, 2, 2, 2, 2, 2, 2, 2, 2, 2, 2, 2, 2, 2, 2, 2, 2, 2, 2, 2, 2, 2, 2, 2, 2, 2, 2, 2, 2, 2, 2, 2, 2, 2, 2, 2, 2, 2, 2, 2, 2, 2, 2, 2, 2, 2, 2, 2, 2, 2, 2, 2, 2, 2, 2, 2, 2, 2, 2, 2, 2, 2, 2, 2, 2, 2, 2, 2, 2, 2, 2, 2, 2, 2, 2, 2, 2, 2, 2, 2, 2, 2, 2, 2, 2, 2, 2, 2, 2, 2, 2, 2, 2, 2, 2, 2, 2, 2, 2, 2, 2, 2, 2, 2, 2, 2, 2, 2, 2, 2, 2, 2, 2, 2, 2, 2, 2, 2, 2, 2, 2, 2, 2, 2, 2, 2, 2, 2, 2, 2, 2, 2, 2, 2, 2, 2, 2, 2, 2, 2, 2, 2, 2, 2, 2, 2, 2, 2, 2, 2, 2, 2, 2, 2, 2, 2, 2, 2, 2, 2, 2, 2, 2, 2, 2, 2, 2, 2, 2, 2, 2, 2, 2, 2, 2, 2, 2, 2, 2, 2, 2, 2, 2, 2, 2, 2, 2, 2, 2, 2, 2, 2, 2, 2, 2, 2, 2, 2, 2, 2, 2, 2, 2, 2, 2, 2, 2, 2, 2, 2, 2, 2, 2, 2, 3 ),
 ( 0.000000000000000000, 1.000000000000000000 ),
 ( 0.000000000000000000, 0.003571428571428571317, 0.007142857142857142634, 0.01071428571428571438, 0.01428571428571428527, 0.01785714285714285615, 0.02142857142857142877, 0.02500000000000000139, 0.02857142857142857054, 0.03214285714285713969, 0.03571428571428571230, 0.03928571428571428492, 0.04285714285714285754, 0.04642857142857143016, 0.05000000000000000278, 0.05357142857142856845, 0.05714285714285714107, 0.06071428571428571369, 0.06428571428571427937, 0.06785714285714285199, 0.07142857142857142461, 0.07499999999999999722, 0.07857142857142856984, 0.08214285714285714246, 0.08571428571428571508, 0.08928571428571428770, 0.09285714285714286031, 0.09642857142857143293, 0.1000000000000000056, 0.1035714285714285782, 0.1071428571428571369, 0.1107142857142857095, 0.1142857142857142821, 0.1178571428571428548, 0.1214285714285714274, 0.1250000000000000000, 0.1285714285714285587, 0.1321428571428571452, 0.1357142857142857040, 0.1392857142857142905, 0.1428571428571428492, 0.1464285714285714357, 0.1499999999999999944, 0.1535714285714285809, 0.1571428571428571397, 0.1607142857142857262, 0.1642857142857142849, 0.1678571428571428437, 0.1714285714285714302, 0.1749999999999999889, 0.1785714285714285754, 0.1821428571428571341, 0.1857142857142857206, 0.1892857142857142794, 0.1928571428571428659, 0.1964285714285714246, 0.2000000000000000111, 0.2035714285714285698, 0.2071428571428571563, 0.2107142857142857151, 0.2142857142857142738, 0.2178571428571428603, 0.2214285714285714191, 0.2250000000000000056, 0.2285714285714285643, 0.2321428571428571508, 0.2357142857142857095, 0.2392857142857142960, 0.2428571428571428548, 0.2464285714285714413, 0.2500000000000000000, 0.2535714285714285587, 0.2571428571428571175, 0.2607142857142857317, 0.2642857142857142905, 0.2678571428571428492, 0.2714285714285714080, 0.2750000000000000222, 0.2785714285714285809, 0.2821428571428571397, 0.2857142857142856984, 0.2892857142857143127, 0.2928571428571428714, 0.2964285714285714302, 0.2999999999999999889, 0.3035714285714285476, 0.3071428571428571619, 0.3107142857142857206, 0.3142857142857142794, 0.3178571428571428381, 0.3214285714285714524, 0.3250000000000000111, 0.3285714285714285698, 0.3321428571428571286, 0.3357142857142856873, 0.3392857142857143016, 0.3428571428571428603, 0.3464285714285714191, 0.3499999999999999778, 0.3535714285714285920, 0.3571428571428571508, 0.3607142857142857095, 0.3642857142857142683, 0.3678571428571428825, 0.3714285714285714413, 0.3750000000000000000, 0.3785714285714285587, 0.3821428571428571175, 0.3857142857142857317, 0.3892857142857142905, 0.3928571428571428492, 0.3964285714285714080, 0.4000000000000000222, 0.4035714285714285809, 0.4071428571428571397, 0.4107142857142856984, 0.4142857142857143127, 0.4178571428571428714, 0.4214285714285714302, 0.4249999999999999889, 0.4285714285714285476, 0.4321428571428571619, 0.4357142857142857206, 0.4392857142857142794, 0.4428571428571428381, 0.4464285714285714524, 0.4500000000000000111, 0.4535714285714285698, 0.4571428571428571286, 0.4607142857142856873, 0.4642857142857143016, 0.4678571428571428603, 0.4714285714285714191, 0.4749999999999999778, 0.4785714285714285920, 0.4821428571428571508, 0.4857142857142857095, 0.4892857142857142683, 0.4928571428571428825, 0.4964285714285714413, 0.5000000000000000000, 0.5035714285714285587, 0.5071428571428571175, 0.5107142857142856762, 0.5142857142857142350, 0.5178571428571429047, 0.5214285714285714635, 0.5250000000000000222, 0.5285714285714285809, 0.5321428571428571397, 0.5357142857142856984, 0.5392857142857142572, 0.5428571428571428159, 0.5464285714285713746, 0.5500000000000000444, 0.5535714285714286031, 0.5571428571428571619, 0.5607142857142857206, 0.5642857142857142794, 0.5678571428571428381, 0.5714285714285713969, 0.5749999999999999556, 0.5785714285714286254, 0.5821428571428571841, 0.5857142857142857428, 0.5892857142857143016, 0.5928571428571428603, 0.5964285714285714191, 0.5999999999999999778, 0.6035714285714285365, 0.6071428571428570953, 0.6107142857142857650, 0.6142857142857143238, 0.6178571428571428825, 0.6214285714285714413, 0.6250000000000000000, 0.6285714285714285587, 0.6321428571428571175, 0.6357142857142856762, 0.6392857142857142350, 0.6428571428571429047, 0.6464285714285714635, 0.6500000000000000222, 0.6535714285714285809, 0.6571428571428571397, 0.6607142857142856984, 0.6642857142857142572, 0.6678571428571428159, 0.6714285714285713746, 0.6750000000000000444, 0.6785714285714286031, 0.6821428571428571619, 0.6857142857142857206, 0.6892857142857142794, 0.6928571428571428381, 0.6964285714285713969, 0.6999999999999999556, 0.7035714285714286254, 0.7071428571428571841, 0.7107142857142857428, 0.7142857142857143016, 0.7178571428571428603, 0.7214285714285714191, 0.7249999999999999778, 0.7285714285714285365, 0.7321428571428570953, 0.7357142857142857650, 0.7392857142857143238, 0.7428571428571428825, 0.7464285714285714413, 0.7500000000000000000, 0.7535714285714285587, 0.7571428571428571175, 0.7607142857142856762, 0.7642857142857142350, 0.7678571428571429047, 0.7714285714285714635, 0.7750000000000000222, 0.7785714285714285809, 0.7821428571428571397, 0.7857142857142856984, 0.7892857142857142572, 0.7928571428571428159, 0.7964285714285713746, 0.8000000000000000444, 0.8035714285714286031, 0.8071428571428571619, 0.8107142857142857206, 0.8142857142857142794, 0.8178571428571428381, 0.8214285714285713969, 0.8249999999999999556, 0.8285714285714286254, 0.8321428571428571841, 0.8357142857142857428, 0.8392857142857143016, 0.8428571428571428603, 0.8464285714285714191, 0.8499999999999999778, 0.8535714285714285365, 0.8571428571428570953, 0.8607142857142857650, 0.8642857142857143238, 0.8678571428571428825, 0.8714285714285714413, 0.8750000000000000000, 0.8785714285714285587, 0.8821428571428571175, 0.8857142857142856762, 0.8892857142857142350, 0.8928571428571429047, 0.8964285714285714635, 0.9000000000000000222, 0.9035714285714285809, 0.9071428571428571397, 0.9107142857142856984, 0.9142857142857142572, 0.9178571428571428159, 0.9214285714285713746, 0.9250000000000000444, 0.9285714285714286031, 0.9321428571428571619, 0.9357142857142857206, 0.9392857142857142794, 0.9428571428571428381, 0.9464285714285713969, 0.9499999999999999556, 0.9535714285714286254, 0.9571428571428571841, 0.9607142857142857428, 0.9642857142857143016, 0.9678571428571428603, 0.9714285714285714191, 0.9749999999999999778, 0.9785714285714285365, 0.9821428571428570953 ),
 .UNSPECIFIED. ) 
 GEOMETRIC_REPRESENTATION_ITEM ( )  RATIONAL_B_SPLINE_SURFACE ( (
 ( 1.000000000000000000, 0.9510565162951535312, 1.000000000000000000, 0.9510565162951535312, 1.000000000000000000, 0.9510565162951535312, 1.000000000000000000, 0.9510565162951535312, 1.000000000000000000, 0.9510565162951535312, 1.000000000000000000, 0.9510565162951535312, 1.000000000000000000, 0.9510565162951535312, 1.000000000000000000, 0.9510565162951535312, 1.000000000000000000, 0.9510565162951535312, 1.000000000000000000, 0.9510565162951535312, 1.000000000000000000, 0.9510565162951535312, 1.000000000000000000, 0.9510565162951535312, 1.000000000000000000, 0.9510565162951535312, 1.000000000000000000, 0.9510565162951535312, 1.000000000000000000, 0.9510565162951535312, 1.000000000000000000, 0.9510565162951535312, 1.000000000000000000, 0.9510565162951535312, 1.000000000000000000, 0.9510565162951535312, 1.000000000000000000, 0.9510565162951535312, 1.000000000000000000, 0.9510565162951535312, 1.000000000000000000, 0.9510565162951535312, 1.000000000000000000, 0.9510565162951535312, 1.000000000000000000, 0.9510565162951535312, 1.000000000000000000, 0.9510565162951535312, 1.000000000000000000, 0.9510565162951535312, 1.000000000000000000, 0.9510565162951535312, 1.000000000000000000, 0.9510565162951535312, 1.000000000000000000, 0.9510565162951535312, 1.000000000000000000, 0.9510565162951535312, 1.000000000000000000, 0.9510565162951535312, 1.000000000000000000, 0.9510565162951535312, 1.000000000000000000, 0.9510565162951535312, 1.000000000000000000, 0.9510565162951535312, 1.000000000000000000, 0.9510565162951535312, 1.000000000000000000, 0.9510565162951535312, 1.000000000000000000, 0.9510565162951535312, 1.000000000000000000, 0.9510565162951535312, 1.000000000000000000, 0.9510565162951535312, 1.000000000000000000, 0.9510565162951535312, 1.000000000000000000, 0.9510565162951535312, 1.000000000000000000, 0.9510565162951535312, 1.000000000000000000, 0.9510565162951535312, 1.000000000000000000, 0.9510565162951535312, 1.000000000000000000, 0.9510565162951535312, 1.000000000000000000, 0.9510565162951535312, 1.000000000000000000, 0.9510565162951535312, 1.000000000000000000, 0.9510565162951535312, 1.000000000000000000, 0.9510565162951535312, 1.000000000000000000, 0.9510565162951535312, 1.000000000000000000, 0.9510565162951535312, 1.000000000000000000, 0.9510565162951535312, 1.000000000000000000, 0.9510565162951535312, 1.000000000000000000, 0.9510565162951535312, 1.000000000000000000, 0.9510565162951535312, 1.000000000000000000, 0.9510565162951535312, 1.000000000000000000, 0.9510565162951535312, 1.000000000000000000, 0.9510565162951535312, 1.000000000000000000, 0.9510565162951535312, 1.000000000000000000, 0.9510565162951535312, 1.000000000000000000, 0.9510565162951535312, 1.000000000000000000, 0.9510565162951535312, 1.000000000000000000, 0.9510565162951535312, 1.000000000000000000, 0.9510565162951535312, 1.000000000000000000, 0.9510565162951535312, 1.000000000000000000, 0.9510565162951535312, 1.000000000000000000, 0.9510565162951535312, 1.000000000000000000, 0.9510565162951535312, 1.000000000000000000, 0.9510565162951535312, 1.000000000000000000, 0.9510565162951535312, 1.000000000000000000, 0.9510565162951535312, 1.000000000000000000, 0.9510565162951535312, 1.000000000000000000, 0.9510565162951535312, 1.000000000000000000, 0.9510565162951535312, 1.000000000000000000, 0.9510565162951535312, 1.000000000000000000, 0.9510565162951535312, 1.000000000000000000, 0.9510565162951535312, 1.000000000000000000, 0.9510565162951535312, 1.000000000000000000, 0.9510565162951535312, 1.000000000000000000, 0.9510565162951535312, 1.000000000000000000, 0.9510565162951535312, 1.000000000000000000, 0.9510565162951535312, 1.000000000000000000, 0.9510565162951535312, 1.000000000000000000, 0.9510565162951535312, 1.000000000000000000, 0.9510565162951535312, 1.000000000000000000, 0.9510565162951535312, 1.000000000000000000, 0.9510565162951535312, 1.000000000000000000, 0.9510565162951535312, 1.000000000000000000, 0.9510565162951535312, 1.000000000000000000, 0.9510565162951535312, 1.000000000000000000, 0.9510565162951535312, 1.000000000000000000, 0.9510565162951535312, 1.000000000000000000, 0.9510565162951535312, 1.000000000000000000, 0.9510565162951535312, 1.000000000000000000, 0.9510565162951535312, 1.000000000000000000, 0.9510565162951535312, 1.000000000000000000, 0.9510565162951535312, 1.000000000000000000, 0.9510565162951535312, 1.000000000000000000, 0.9510565162951535312, 1.000000000000000000, 0.9510565162951535312, 1.000000000000000000, 0.9510565162951535312, 1.000000000000000000, 0.9510565162951535312, 1.000000000000000000, 0.9510565162951535312, 1.000000000000000000, 0.9510565162951535312, 1.000000000000000000, 0.9510565162951535312, 1.000000000000000000, 0.9510565162951535312, 1.000000000000000000, 0.9510565162951535312, 1.000000000000000000, 0.9510565162951535312, 1.000000000000000000, 0.9510565162951535312, 1.000000000000000000, 0.9510565162951535312, 1.000000000000000000, 0.9510565162951535312, 1.000000000000000000, 0.9510565162951535312, 1.000000000000000000, 0.9510565162951535312, 1.000000000000000000, 0.9510565162951535312, 1.000000000000000000, 0.9510565162951535312, 1.000000000000000000, 0.9510565162951535312, 1.000000000000000000, 0.9510565162951535312, 1.000000000000000000, 0.9510565162951535312, 1.000000000000000000, 0.9510565162951535312, 1.000000000000000000, 0.9510565162951535312, 1.000000000000000000, 0.9510565162951535312, 1.000000000000000000, 0.9510565162951535312, 1.000000000000000000, 0.9510565162951535312, 1.000000000000000000, 0.9510565162951535312, 1.000000000000000000, 0.9510565162951535312, 1.000000000000000000, 0.9510565162951535312, 1.000000000000000000, 0.9510565162951535312, 1.000000000000000000, 0.9510565162951535312, 1.000000000000000000, 0.9510565162951535312, 1.000000000000000000, 0.9510565162951535312, 1.000000000000000000, 0.9510565162951535312, 1.000000000000000000, 0.9510565162951535312, 1.000000000000000000, 0.9510565162951535312, 1.000000000000000000, 0.9510565162951535312, 1.000000000000000000, 0.9510565162951535312, 1.000000000000000000, 0.9510565162951535312, 1.000000000000000000, 0.9510565162951535312, 1.000000000000000000, 0.9510565162951535312, 1.000000000000000000, 0.9510565162951535312, 1.000000000000000000, 0.9510565162951535312, 1.000000000000000000, 0.9510565162951535312, 1.000000000000000000, 0.9510565162951535312, 1.000000000000000000, 0.9510565162951535312, 1.000000000000000000, 0.9510565162951535312, 1.000000000000000000, 0.9510565162951535312, 1.000000000000000000, 0.9510565162951535312, 1.000000000000000000, 0.9510565162951535312, 1.000000000000000000, 0.9510565162951535312, 1.000000000000000000, 0.9510565162951535312, 1.000000000000000000, 0.9510565162951535312, 1.000000000000000000, 0.9510565162951535312, 1.000000000000000000, 0.9510565162951535312, 1.000000000000000000, 0.9510565162951535312, 1.000000000000000000, 0.9510565162951535312, 1.000000000000000000, 0.9510565162951535312, 1.000000000000000000, 0.9510565162951535312, 1.000000000000000000, 0.9510565162951535312, 1.000000000000000000, 0.9510565162951535312, 1.000000000000000000, 0.9510565162951535312, 1.000000000000000000, 0.9510565162951535312, 1.000000000000000000, 0.9510565162951535312, 1.000000000000000000, 0.9510565162951535312, 1.000000000000000000, 0.9510565162951535312, 1.000000000000000000, 0.9510565162951535312, 1.000000000000000000, 0.9510565162951535312, 1.000000000000000000, 0.9510565162951535312, 1.000000000000000000, 0.9510565162951535312, 1.000000000000000000, 0.9510565162951535312, 1.000000000000000000, 0.9510565162951535312, 1.000000000000000000, 0.9510565162951535312, 1.000000000000000000, 0.9510565162951535312, 1.000000000000000000, 0.9510565162951535312, 1.000000000000000000, 0.9510565162951535312, 1.000000000000000000, 0.9510565162951535312, 1.000000000000000000, 0.9510565162951535312, 1.000000000000000000, 0.9510565162951535312, 1.000000000000000000, 0.9510565162951535312, 1.000000000000000000, 0.9510565162951535312, 1.000000000000000000, 0.9510565162951535312, 1.000000000000000000, 0.9510565162951535312, 1.000000000000000000, 0.9510565162951535312, 1.000000000000000000, 0.9510565162951535312, 1.000000000000000000, 0.9510565162951535312, 1.000000000000000000, 0.9510565162951535312, 1.000000000000000000, 0.9510565162951535312, 1.000000000000000000, 0.9510565162951535312, 1.000000000000000000, 0.9510565162951535312, 1.000000000000000000, 0.9510565162951535312, 1.000000000000000000, 0.9510565162951535312, 1.000000000000000000, 0.9510565162951535312, 1.000000000000000000, 0.9510565162951535312, 1.000000000000000000, 0.9510565162951535312, 1.000000000000000000, 0.9510565162951535312, 1.000000000000000000, 0.9510565162951535312, 1.000000000000000000, 0.9510565162951535312, 1.000000000000000000, 0.9510565162951535312, 1.000000000000000000, 0.9510565162951535312, 1.000000000000000000, 0.9510565162951535312, 1.000000000000000000, 0.9510565162951535312, 1.000000000000000000, 0.9510565162951535312, 1.000000000000000000, 0.9510565162951535312, 1.000000000000000000, 0.9510565162951535312, 1.000000000000000000, 0.9510565162951535312, 1.000000000000000000, 0.9510565162951535312, 1.000000000000000000, 0.9510565162951535312, 1.000000000000000000, 0.9510565162951535312, 1.000000000000000000, 0.9510565162951535312, 1.000000000000000000, 0.9510565162951535312, 1.000000000000000000, 0.9510565162951535312, 1.000000000000000000, 0.9510565162951535312, 1.000000000000000000, 0.9510565162951535312, 1.000000000000000000, 0.9510565162951535312, 1.000000000000000000, 0.9510565162951535312, 1.000000000000000000, 0.9510565162951535312, 1.000000000000000000, 0.9510565162951535312, 1.000000000000000000, 0.9510565162951535312, 1.000000000000000000, 0.9510565162951535312, 1.000000000000000000, 0.9510565162951535312, 1.000000000000000000, 0.9510565162951535312, 1.000000000000000000, 0.9510565162951535312, 1.000000000000000000, 0.9510565162951535312, 1.000000000000000000, 0.9510565162951535312, 1.000000000000000000, 0.9510565162951535312, 1.000000000000000000, 0.9510565162951535312, 1.000000000000000000, 0.9510565162951535312, 1.000000000000000000, 0.9510565162951535312, 1.000000000000000000, 0.9510565162951535312, 1.000000000000000000, 0.9510565162951535312, 1.000000000000000000, 0.9510565162951535312, 1.000000000000000000, 0.9510565162951535312, 1.000000000000000000, 0.9510565162951535312, 1.000000000000000000, 0.9510565162951535312, 1.000000000000000000, 0.9510565162951535312, 1.000000000000000000, 0.9510565162951535312, 1.000000000000000000, 0.9510565162951535312, 1.000000000000000000, 0.9510565162951535312, 1.000000000000000000, 0.9510565162951535312, 1.000000000000000000, 0.9510565162951535312, 1.000000000000000000, 0.9510565162951535312, 1.000000000000000000, 0.9510565162951535312, 1.000000000000000000, 0.9510565162951535312, 1.000000000000000000, 0.9510565162951535312, 1.000000000000000000, 0.9510565162951535312, 1.000000000000000000, 0.9510565162951535312, 1.000000000000000000, 0.9510565162951535312, 1.000000000000000000, 0.9510565162951535312, 1.000000000000000000, 0.9510565162951535312, 1.000000000000000000, 0.9510565162951535312, 1.000000000000000000, 0.9510565162951535312, 1.000000000000000000, 0.9510565162951535312, 1.000000000000000000, 0.9510565162951535312, 1.000000000000000000, 0.9510565162951535312, 1.000000000000000000, 0.9510565162951535312, 1.000000000000000000, 0.9510565162951535312, 1.000000000000000000, 0.9510565162951535312, 1.000000000000000000, 0.9510565162951535312, 1.000000000000000000, 0.9510565162951535312, 1.000000000000000000, 0.9510565162951535312, 1.000000000000000000, 0.9510565162951535312, 1.000000000000000000, 0.9510565162951535312, 1.000000000000000000, 0.9510565162951535312, 1.000000000000000000, 0.9510565162951535312, 1.000000000000000000, 0.9510565162951535312, 1.000000000000000000, 0.9510565162951535312, 1.000000000000000000, 0.9510565162951535312, 1.000000000000000000, 0.9510565162951535312, 1.000000000000000000, 0.9510565162951535312, 1.000000000000000000, 0.9510565162951535312, 1.000000000000000000, 0.9510565162951535312, 1.000000000000000000, 0.9510565162951535312, 1.000000000000000000, 0.9510565162951535312, 1.000000000000000000, 0.9510565162951535312, 1.000000000000000000, 0.9510565162951535312, 1.000000000000000000, 0.9510565162951535312, 1.000000000000000000, 0.9510565162951535312, 1.000000000000000000, 0.9510565162951535312, 1.000000000000000000),
 ( 1.000000000000000000, 0.9510565162951535312, 1.000000000000000000, 0.9510565162951535312, 1.000000000000000000, 0.9510565162951535312, 1.000000000000000000, 0.9510565162951535312, 1.000000000000000000, 0.9510565162951535312, 1.000000000000000000, 0.9510565162951535312, 1.000000000000000000, 0.9510565162951535312, 1.000000000000000000, 0.9510565162951535312, 1.000000000000000000, 0.9510565162951535312, 1.000000000000000000, 0.9510565162951535312, 1.000000000000000000, 0.9510565162951535312, 1.000000000000000000, 0.9510565162951535312, 1.000000000000000000, 0.9510565162951535312, 1.000000000000000000, 0.9510565162951535312, 1.000000000000000000, 0.9510565162951535312, 1.000000000000000000, 0.9510565162951535312, 1.000000000000000000, 0.9510565162951535312, 1.000000000000000000, 0.9510565162951535312, 1.000000000000000000, 0.9510565162951535312, 1.000000000000000000, 0.9510565162951535312, 1.000000000000000000, 0.9510565162951535312, 1.000000000000000000, 0.9510565162951535312, 1.000000000000000000, 0.9510565162951535312, 1.000000000000000000, 0.9510565162951535312, 1.000000000000000000, 0.9510565162951535312, 1.000000000000000000, 0.9510565162951535312, 1.000000000000000000, 0.9510565162951535312, 1.000000000000000000, 0.9510565162951535312, 1.000000000000000000, 0.9510565162951535312, 1.000000000000000000, 0.9510565162951535312, 1.000000000000000000, 0.9510565162951535312, 1.000000000000000000, 0.9510565162951535312, 1.000000000000000000, 0.9510565162951535312, 1.000000000000000000, 0.9510565162951535312, 1.000000000000000000, 0.9510565162951535312, 1.000000000000000000, 0.9510565162951535312, 1.000000000000000000, 0.9510565162951535312, 1.000000000000000000, 0.9510565162951535312, 1.000000000000000000, 0.9510565162951535312, 1.000000000000000000, 0.9510565162951535312, 1.000000000000000000, 0.9510565162951535312, 1.000000000000000000, 0.9510565162951535312, 1.000000000000000000, 0.9510565162951535312, 1.000000000000000000, 0.9510565162951535312, 1.000000000000000000, 0.9510565162951535312, 1.000000000000000000, 0.9510565162951535312, 1.000000000000000000, 0.9510565162951535312, 1.000000000000000000, 0.9510565162951535312, 1.000000000000000000, 0.9510565162951535312, 1.000000000000000000, 0.9510565162951535312, 1.000000000000000000, 0.9510565162951535312, 1.000000000000000000, 0.9510565162951535312, 1.000000000000000000, 0.9510565162951535312, 1.000000000000000000, 0.9510565162951535312, 1.000000000000000000, 0.9510565162951535312, 1.000000000000000000, 0.9510565162951535312, 1.000000000000000000, 0.9510565162951535312, 1.000000000000000000, 0.9510565162951535312, 1.000000000000000000, 0.9510565162951535312, 1.000000000000000000, 0.9510565162951535312, 1.000000000000000000, 0.9510565162951535312, 1.000000000000000000, 0.9510565162951535312, 1.000000000000000000, 0.9510565162951535312, 1.000000000000000000, 0.9510565162951535312, 1.000000000000000000, 0.9510565162951535312, 1.000000000000000000, 0.9510565162951535312, 1.000000000000000000, 0.9510565162951535312, 1.000000000000000000, 0.9510565162951535312, 1.000000000000000000, 0.9510565162951535312, 1.000000000000000000, 0.9510565162951535312, 1.000000000000000000, 0.9510565162951535312, 1.000000000000000000, 0.9510565162951535312, 1.000000000000000000, 0.9510565162951535312, 1.000000000000000000, 0.9510565162951535312, 1.000000000000000000, 0.9510565162951535312, 1.000000000000000000, 0.9510565162951535312, 1.000000000000000000, 0.9510565162951535312, 1.000000000000000000, 0.9510565162951535312, 1.000000000000000000, 0.9510565162951535312, 1.000000000000000000, 0.9510565162951535312, 1.000000000000000000, 0.9510565162951535312, 1.000000000000000000, 0.9510565162951535312, 1.000000000000000000, 0.9510565162951535312, 1.000000000000000000, 0.9510565162951535312, 1.000000000000000000, 0.9510565162951535312, 1.000000000000000000, 0.9510565162951535312, 1.000000000000000000, 0.9510565162951535312, 1.000000000000000000, 0.9510565162951535312, 1.000000000000000000, 0.9510565162951535312, 1.000000000000000000, 0.9510565162951535312, 1.000000000000000000, 0.9510565162951535312, 1.000000000000000000, 0.9510565162951535312, 1.000000000000000000, 0.9510565162951535312, 1.000000000000000000, 0.9510565162951535312, 1.000000000000000000, 0.9510565162951535312, 1.000000000000000000, 0.9510565162951535312, 1.000000000000000000, 0.9510565162951535312, 1.000000000000000000, 0.9510565162951535312, 1.000000000000000000, 0.9510565162951535312, 1.000000000000000000, 0.9510565162951535312, 1.000000000000000000, 0.9510565162951535312, 1.000000000000000000, 0.9510565162951535312, 1.000000000000000000, 0.9510565162951535312, 1.000000000000000000, 0.9510565162951535312, 1.000000000000000000, 0.9510565162951535312, 1.000000000000000000, 0.9510565162951535312, 1.000000000000000000, 0.9510565162951535312, 1.000000000000000000, 0.9510565162951535312, 1.000000000000000000, 0.9510565162951535312, 1.000000000000000000, 0.9510565162951535312, 1.000000000000000000, 0.9510565162951535312, 1.000000000000000000, 0.9510565162951535312, 1.000000000000000000, 0.9510565162951535312, 1.000000000000000000, 0.9510565162951535312, 1.000000000000000000, 0.9510565162951535312, 1.000000000000000000, 0.9510565162951535312, 1.000000000000000000, 0.9510565162951535312, 1.000000000000000000, 0.9510565162951535312, 1.000000000000000000, 0.9510565162951535312, 1.000000000000000000, 0.9510565162951535312, 1.000000000000000000, 0.9510565162951535312, 1.000000000000000000, 0.9510565162951535312, 1.000000000000000000, 0.9510565162951535312, 1.000000000000000000, 0.9510565162951535312, 1.000000000000000000, 0.9510565162951535312, 1.000000000000000000, 0.9510565162951535312, 1.000000000000000000, 0.9510565162951535312, 1.000000000000000000, 0.9510565162951535312, 1.000000000000000000, 0.9510565162951535312, 1.000000000000000000, 0.9510565162951535312, 1.000000000000000000, 0.9510565162951535312, 1.000000000000000000, 0.9510565162951535312, 1.000000000000000000, 0.9510565162951535312, 1.000000000000000000, 0.9510565162951535312, 1.000000000000000000, 0.9510565162951535312, 1.000000000000000000, 0.9510565162951535312, 1.000000000000000000, 0.9510565162951535312, 1.000000000000000000, 0.9510565162951535312, 1.000000000000000000, 0.9510565162951535312, 1.000000000000000000, 0.9510565162951535312, 1.000000000000000000, 0.9510565162951535312, 1.000000000000000000, 0.9510565162951535312, 1.000000000000000000, 0.9510565162951535312, 1.000000000000000000, 0.9510565162951535312, 1.000000000000000000, 0.9510565162951535312, 1.000000000000000000, 0.9510565162951535312, 1.000000000000000000, 0.9510565162951535312, 1.000000000000000000, 0.9510565162951535312, 1.000000000000000000, 0.9510565162951535312, 1.000000000000000000, 0.9510565162951535312, 1.000000000000000000, 0.9510565162951535312, 1.000000000000000000, 0.9510565162951535312, 1.000000000000000000, 0.9510565162951535312, 1.000000000000000000, 0.9510565162951535312, 1.000000000000000000, 0.9510565162951535312, 1.000000000000000000, 0.9510565162951535312, 1.000000000000000000, 0.9510565162951535312, 1.000000000000000000, 0.9510565162951535312, 1.000000000000000000, 0.9510565162951535312, 1.000000000000000000, 0.9510565162951535312, 1.000000000000000000, 0.9510565162951535312, 1.000000000000000000, 0.9510565162951535312, 1.000000000000000000, 0.9510565162951535312, 1.000000000000000000, 0.9510565162951535312, 1.000000000000000000, 0.9510565162951535312, 1.000000000000000000, 0.9510565162951535312, 1.000000000000000000, 0.9510565162951535312, 1.000000000000000000, 0.9510565162951535312, 1.000000000000000000, 0.9510565162951535312, 1.000000000000000000, 0.9510565162951535312, 1.000000000000000000, 0.9510565162951535312, 1.000000000000000000, 0.9510565162951535312, 1.000000000000000000, 0.9510565162951535312, 1.000000000000000000, 0.9510565162951535312, 1.000000000000000000, 0.9510565162951535312, 1.000000000000000000, 0.9510565162951535312, 1.000000000000000000, 0.9510565162951535312, 1.000000000000000000, 0.9510565162951535312, 1.000000000000000000, 0.9510565162951535312, 1.000000000000000000, 0.9510565162951535312, 1.000000000000000000, 0.9510565162951535312, 1.000000000000000000, 0.9510565162951535312, 1.000000000000000000, 0.9510565162951535312, 1.000000000000000000, 0.9510565162951535312, 1.000000000000000000, 0.9510565162951535312, 1.000000000000000000, 0.9510565162951535312, 1.000000000000000000, 0.9510565162951535312, 1.000000000000000000, 0.9510565162951535312, 1.000000000000000000, 0.9510565162951535312, 1.000000000000000000, 0.9510565162951535312, 1.000000000000000000, 0.9510565162951535312, 1.000000000000000000, 0.9510565162951535312, 1.000000000000000000, 0.9510565162951535312, 1.000000000000000000, 0.9510565162951535312, 1.000000000000000000, 0.9510565162951535312, 1.000000000000000000, 0.9510565162951535312, 1.000000000000000000, 0.9510565162951535312, 1.000000000000000000, 0.9510565162951535312, 1.000000000000000000, 0.9510565162951535312, 1.000000000000000000, 0.9510565162951535312, 1.000000000000000000, 0.9510565162951535312, 1.000000000000000000, 0.9510565162951535312, 1.000000000000000000, 0.9510565162951535312, 1.000000000000000000, 0.9510565162951535312, 1.000000000000000000, 0.9510565162951535312, 1.000000000000000000, 0.9510565162951535312, 1.000000000000000000, 0.9510565162951535312, 1.000000000000000000, 0.9510565162951535312, 1.000000000000000000, 0.9510565162951535312, 1.000000000000000000, 0.9510565162951535312, 1.000000000000000000, 0.9510565162951535312, 1.000000000000000000, 0.9510565162951535312, 1.000000000000000000, 0.9510565162951535312, 1.000000000000000000, 0.9510565162951535312, 1.000000000000000000, 0.9510565162951535312, 1.000000000000000000, 0.9510565162951535312, 1.000000000000000000, 0.9510565162951535312, 1.000000000000000000, 0.9510565162951535312, 1.000000000000000000, 0.9510565162951535312, 1.000000000000000000, 0.9510565162951535312, 1.000000000000000000, 0.9510565162951535312, 1.000000000000000000, 0.9510565162951535312, 1.000000000000000000, 0.9510565162951535312, 1.000000000000000000, 0.9510565162951535312, 1.000000000000000000, 0.9510565162951535312, 1.000000000000000000, 0.9510565162951535312, 1.000000000000000000, 0.9510565162951535312, 1.000000000000000000, 0.9510565162951535312, 1.000000000000000000, 0.9510565162951535312, 1.000000000000000000, 0.9510565162951535312, 1.000000000000000000, 0.9510565162951535312, 1.000000000000000000, 0.9510565162951535312, 1.000000000000000000, 0.9510565162951535312, 1.000000000000000000, 0.9510565162951535312, 1.000000000000000000, 0.9510565162951535312, 1.000000000000000000, 0.9510565162951535312, 1.000000000000000000, 0.9510565162951535312, 1.000000000000000000, 0.9510565162951535312, 1.000000000000000000, 0.9510565162951535312, 1.000000000000000000, 0.9510565162951535312, 1.000000000000000000, 0.9510565162951535312, 1.000000000000000000, 0.9510565162951535312, 1.000000000000000000, 0.9510565162951535312, 1.000000000000000000, 0.9510565162951535312, 1.000000000000000000, 0.9510565162951535312, 1.000000000000000000, 0.9510565162951535312, 1.000000000000000000, 0.9510565162951535312, 1.000000000000000000, 0.9510565162951535312, 1.000000000000000000, 0.9510565162951535312, 1.000000000000000000, 0.9510565162951535312, 1.000000000000000000, 0.9510565162951535312, 1.000000000000000000, 0.9510565162951535312, 1.000000000000000000, 0.9510565162951535312, 1.000000000000000000, 0.9510565162951535312, 1.000000000000000000, 0.9510565162951535312, 1.000000000000000000, 0.9510565162951535312, 1.000000000000000000, 0.9510565162951535312, 1.000000000000000000, 0.9510565162951535312, 1.000000000000000000, 0.9510565162951535312, 1.000000000000000000, 0.9510565162951535312, 1.000000000000000000, 0.9510565162951535312, 1.000000000000000000, 0.9510565162951535312, 1.000000000000000000, 0.9510565162951535312, 1.000000000000000000, 0.9510565162951535312, 1.000000000000000000, 0.9510565162951535312, 1.000000000000000000, 0.9510565162951535312, 1.000000000000000000, 0.9510565162951535312, 1.000000000000000000, 0.9510565162951535312, 1.000000000000000000, 0.9510565162951535312, 1.000000000000000000, 0.9510565162951535312, 1.000000000000000000, 0.9510565162951535312, 1.000000000000000000, 0.9510565162951535312, 1.000000000000000000, 0.9510565162951535312, 1.000000000000000000, 0.9510565162951535312, 1.000000000000000000, 0.9510565162951535312, 1.000000000000000000) ) ) 
 REPRESENTATION_ITEM ( '' )  SURFACE ( )  );
#21335 = CARTESIAN_POINT ( 'NONE',  ( -3.499999999999999556, -3.004629197474309385E-15, -2.899999999999999911 ) ) ;
#21336 = CARTESIAN_POINT ( 'NONE',  ( -6.658902113226115027, -5.287118297636088649, -7.776713651266535798 ) ) ;
#21337 = ORIENTED_EDGE ( 'NONE', *, *, #15407, .F. ) ;
#21338 = CARTESIAN_POINT ( 'NONE',  ( -3.044812012439970683, 197.4746971517856196, 97.89886208192145034 ) ) ;
#21339 = AXIS2_PLACEMENT_3D ( 'NONE', #29751, #31961, #21741 ) ;
#21340 = CARTESIAN_POINT ( 'NONE',  ( -0.05014649552828442242, 219.6175466908591716, 36.24886208192142334 ) ) ;
#21341 = CYLINDRICAL_SURFACE ( 'NONE', #23574, 15.00000000000001776 ) ;
#21342 = CARTESIAN_POINT ( 'NONE',  ( -0.05014649552810635652, 196.4853777576173002, 47.75113791807855534 ) ) ;
#21343 = ORIENTED_EDGE ( 'NONE', *, *, #11189, .T. ) ;
#21344 = VECTOR ( 'NONE', #15098, 1000.000000000000000 ) ;
#21345 = CARTESIAN_POINT ( 'NONE',  ( 2.517493886309087436, 199.4062855549015865, 4.598862081921435419 ) ) ;
#21346 = CARTESIAN_POINT ( 'NONE',  ( 0.000000000000000000, 0.8865213383406687075, -1.535500000000000975 ) ) ;
#21347 = ORIENTED_EDGE ( 'NONE', *, *, #22652, .F. ) ;
#21348 = CARTESIAN_POINT ( 'NONE',  ( -2.517493886309087880, 214.5937144450984135, 87.09886208192143897 ) ) ;
#21349 = EDGE_CURVE ( 'NONE', #19912, #6342, #13729, .T. ) ;
#21350 = CARTESIAN_POINT ( 'NONE',  ( -8.015496119326531499, 204.4483345814780364, 27.35113791807856742 ) ) ;
#21351 = CARTESIAN_POINT ( 'NONE',  ( 117.5000000000000000, 155.0000000000000000, -6.938893903907228378E-15 ) ) ;
#21352 = ORIENTED_EDGE ( 'NONE', *, *, #20956, .T. ) ;
#21353 = DIRECTION ( 'NONE',  ( 1.000000000000000000, 0.000000000000000000, 0.000000000000000000 ) ) ;
#21354 = AXIS2_PLACEMENT_3D ( 'NONE', #31916, #8588, #18985 ) ;
#21355 = CARTESIAN_POINT ( 'NONE',  ( 34.97499999726881015, 140.1801316387863778, -4.815267126137194431 ) ) ;
#21356 = DIRECTION ( 'NONE',  ( -0.000000000000000000, -0.000000000000000000, 1.000000000000000000 ) ) ;
#21357 = CARTESIAN_POINT ( 'NONE',  ( -8.000000000000008882, 207.0476921513413515, 99.50113791807856956 ) ) ;
#21359 = VECTOR ( 'NONE', #15732, 1000.000000000000000 ) ;
#21358 = DIRECTION ( 'NONE',  ( 0.000000000000000000, 0.000000000000000000, 1.000000000000000000 ) ) ;
#21360 = CARTESIAN_POINT ( 'NONE',  ( 57.79999999999999716, 142.6655632788954620, 8.961492836873471646 ) ) ;
#21361 = CARTESIAN_POINT ( 'NONE',  ( -7.984503880673422316, 204.3529502787951628, 74.34886208192142476 ) ) ;
#21362 = CARTESIAN_POINT ( 'NONE',  ( 84.31132485994280046, 169.2658477444273331, 4.635254915624208216 ) ) ;
#21363 = VECTOR ( 'NONE', #16606, 1000.000000000000000 ) ;
#21364 = ADVANCED_FACE ( 'NONE', ( #12140, #30539 ), #25422, .T. ) ;
#21365 = CARTESIAN_POINT ( 'NONE',  ( 60.52499999726881441, 140.1801316387863778, 4.815267126137185549 ) ) ;
#21367 = VERTEX_POINT ( 'NONE', #22872 ) ;
#21366 = CARTESIAN_POINT ( 'NONE',  ( -8.118202686958039038, 201.1607312380087080, 12.20113791807856707 ) ) ;
#21368 = CARTESIAN_POINT ( 'NONE',  ( 36.71132485994280614, 155.0000000000000000, 15.00000000000001243 ) ) ;
#21369 = CARTESIAN_POINT ( 'NONE',  ( 64.42499999726879878, 141.7447067706911810, 9.630534252274376428 ) ) ;
#21370 = CARTESIAN_POINT ( 'NONE',  ( 79.57499999726881867, 164.1591823560292198, -12.60653300113719766 ) ) ;
#21371 = CARTESIAN_POINT ( 'NONE',  ( -7.375838497908182134, 217.2372850707499765, 75.95113791807857240 ) ) ;
#21372 = FACE_OUTER_BOUND ( 'NONE', #27421, .T. ) ;
#21373 = CARTESIAN_POINT ( 'NONE',  ( -3.135527875058821579, 197.5041725223112223, 98.90113791807857524 ) ) ;
#21374 = DIRECTION ( 'NONE',  ( 1.000000000000000000, -0.000000000000000000, -0.000000000000000000 ) ) ;
#21375 = ADVANCED_FACE ( 'NONE', ( #22356 ), #24658, .T. ) ;
#21376 = ORIENTED_EDGE ( 'NONE', *, *, #1992, .T. ) ;
#21377 = CARTESIAN_POINT ( 'NONE',  ( -3.662846001189865142, 195.5725841191952838, 61.89886208192143613 ) ) ;
#21378 = CONICAL_SURFACE ( 'NONE', #19757, 3.999999999999999112, 0.9599310885968813656 ) ;
#21379 = CARTESIAN_POINT ( 'NONE',  ( 10.01549611932659367, 203.7984951890124421, 67.14886208192143613 ) ) ;
#21380 = CARTESIAN_POINT ( 'NONE',  ( -12.01549611932659722, 210.8513442034533227, 8.648862081921436129 ) ) ;
#21381 = PLANE ( 'NONE',  #25159 ) ;
#21382 = CARTESIAN_POINT ( 'NONE',  ( -3.135527875058821579, 197.5041725223112223, 11.90113791807856636 ) ) ;
#21383 = CARTESIAN_POINT ( 'NONE',  ( 10.01549611932659545, 203.7984951890123853, 79.14886208192142192 ) ) ;
#21384 = ORIENTED_EDGE ( 'NONE', *, *, #31618, .T. ) ;
#21385 = CARTESIAN_POINT ( 'NONE',  ( -8.062137200540920645, 212.9164362838581894, 96.80113791807858092 ) ) ;
#21386 = AXIS2_PLACEMENT_3D ( 'NONE', #26436, #6501, #24725 ) ;
#21387 = ORIENTED_EDGE ( 'NONE', *, *, #21669, .T. ) ;
#21388 = CARTESIAN_POINT ( 'NONE',  ( 32.50000000000000000, 155.0000000000000000, -6.938893903907228378E-15 ) ) ;
#21389 =( BOUNDED_SURFACE ( )  B_SPLINE_SURFACE ( 3, 2, ( 
 ( #25089, #1418, #19648, #1747, #4476, #12146, #25261, #4652, #4135, #11810, #1586, #25428, #30037, #30723, #22541, #1927, #33097, #6702, #20319, #15036, #12313, #7208, #12489, #15210, #22709, #17594, #17762, #7383, #14527, #24928, #4816, #7558, #31551, #31387, #23390, #17945, #15875, #10112, #20491, #10778, #4991, #8219, #13322, #30894, #54, #18607, #25935, #28333, #2779, #15378, #20668, #31062, #28994, #219, #5653, #25601, #10289, #20824, #25770, #12996, #2267, #18272, #26270, #23713, #12822, #2938, #28661, #12649, #5155, #2610, #23214, #10450, #5487, #374, #8058, #7721, #2442, #5320, #21153, #31227, #33610, #18107, #28502, #23045, #15543, #33440, #7891, #15709, #26111, #13158, #23550, #10616, #20991, #18441, #28830, #19780, #7173, #4779, #12278, #22503, #27604, #17558, #27775, #19612, #11948, #25227, #12613, #33233, #4272, #22329, #22669, #30688, #17391, #30341, #17217, #27950, #9551, #2064, #14665, #30004, #9384, #17731, #12112, #1891, #27446, #28117, #17051, #12452, #32717, #25392, #22843, #9899, #30175, #6832, #4620, #19942, #1550, #6665, #4440, #20282, #15002, #7351, #25059, #1713, #7005, #15174, #25566, #33406, #32891, #33057, #2231, #14829, #24889, #9726, #20116, #30508, #23009, #4100, #14489, #2402, #336, #28299, #4952, #28955, #23179, #16006, #31516, #15339, #7854, #26398, #10413, #12789, #20957, #33570, #5119, #15509, #3056, #18403, #13444, #23838, #28463, #5280, #10251, #31185, #10079, #2746, #10736, #8186, #31028, #21118, #13119, #20457, #23354, #20786, #7684, #18238, #23677, #18570, #15838, #25900, #20626, #23512, #5614, #28627, #18067, #2570, #12958, #30855, #17, #7519, #17905, #180, #15674, #25732, #26076, #10579, #31350, #8017, #28796, #5452, #26227, #2898, #13285, #29287, #31836, #16667, #29626, #3726, #11226, #27063, #29121, #29451, #13946, #13779, #16837, #512, #11071, #26897, #29793, #18892, #8829, #3886, #837, #18735, #16162, #24510, #5939, #26722, #6275, #8501, #32340, #16498, #6457, #11402, #24175, #3556, #31676, #14116, #21611, #8346, #26553, #9005, #27232, #19394, #14280, #13610, #19231, #668, #21282, #5769, #10905, #1167, #32006, #11563, #16330, #3223, #24005, #21452, #3384, #24335, #8670, #19063, #6101, #21951, #1006, #21779, #32169, #27902, #24843, #17002, #22621, #25018, #6617, #24682, #32844, #17513, #12234, #12406, #14449, #27396, #25348, #27736, #4059, #19731, #1506, #11904, #9507, #1672, #22290, #9178, #7311, #30128, #19894, #9857, #4399, #14784, #32505, #22451, #9679, #22803, #6960, #20072, #30293, #33009, #25176, #32672, #17349, #19568, #1845, #4736, #11730, #33193, #9338, #29961, #17174, #6787, #2017, #27559, #30469, #7130, #4223, #20239, #14622, #4575, #12063, #14961, #30642, #1343, #17687, #28074, #22117, #28420, #28591, #7979, #17857, #15126, #15295, #5413, #33364, #10698, #2529, #12912, #13082, #2358, #18363, #13243, #15798, #30810, #25689, #23640, #10373, #2191, #25863, #23141, #20417, #26189, #33529, #23307, #8148, #12750, #2705, #300, #7809, #18027, #10202, #23472, #25516, #25522, #7472, #20746, #18530, #28755, #20584, #28254, #18200, #2858, #31142, #5242, #30988, #138, #7644, #21077, #10039, #31479, #15631, #26034, #10540, #5076, #28913, #12574, #22966, #4909, #15473, #20921, #31314, #26360, #16293, #13576, #10867, #29584, #23966, #26684, #32302, #5732, #26853, #24469, #31960, #8463, #630, #3514, #13734, #5571, #31636, #11188, #8964, #19188, #11027, #8303, #8629, #16625, #3344, #24132, #3185, #13906, #29247, #21740, #21409, #15965, #29084, #3680, #31796, #21567, #13404, #14072, #3019, #32130, #18694, #11358, #8792, #6237, #16122, #26516, #24290, #5898, #21243, #23799, #799, #27019, #960, #1130, #18850, #19024, #11524, #29412, #6062, #16454, #21905, #19355, #470, #30556, #29924, #14241, #12833, #1936, #4662, #15388, #9946, #20332, #3849, #27996, #15220, #17955, #12498, #25610, #15046, #4829, #30732, #6577, #2114, #24639, #7392, #10300, #16794, #28345, #14877, #1305, #22719, #19528, #7569, #9131, #28170, #12660, #16961, #30903, #11695, #2276, #22077, #23058, #27355, #29749, #32463, #4486, #25438, #9775, #17773, #33451, #25271, #6412, #20159, #12325, #33109, #10121, #20502, #22887, #23224, #7218, #33279, #17606, #5000, #25785, #2452, #33619, #27193, #23889, #31399, #13494, #15552, #15885, #386, #232, #3269, #20676, #31238, #13332, #16215, #5329, #29003, #24050, #21001, #5165, #2619, #10950, #26120, #13168, #26441, #18282, #18781, #2951, #26606, #31560, #10626, #23723, #18117, #3106, #8067, #28515, #13007, #29168, #13657, #5820, #719, #63, #5664, #20835, #7731, #25945, #31073, #557, #18453, #16051, #21325, #23400, #28671, #26279, #10461, #15721, #7901, #2788, #23562, #28840, #5496, #31722, #10788, #21163, #8394, #8227, #18616, #30008, #24221, #17057, #32553, #5989, #8884, #27450, #11449, #3434, #22004, #884, #6155, #16549, #4104, #19443, #14496, #24895, #29501, #6324, #11281, #32219, #11122, #3780, #11776, #9228, #32059, #1388, #14167, #21498, #24393, #21828, #8721, #19280, #24734, #22166, #16884, #26944, #21664, #24560, #19618, #29672, #19111, #3603, #13997, #31885, #1060, #6670, #8552, #1217, #16717, #27118, #11615, #32387, #18945, #9051, #29342, #16377, #29846, #26769, #6506, #13831, #27281, #3938, #14338, #33062, #15179, #25572, #7357, #7010, #25064, #4625, #2236, #20120, #22509, #12118, #17396, #22335, #32896, #12620, #32722, #25396, #25233, #19785, #9556, #2068, #12455 ),
 ( #9731, #12283, #19948, #33240, #1896, #17736, #30347, #11953, #1718, #33412, #27782, #17563, #9389, #10086, #30180, #28125, #4278, #4786, #23015, #20463, #4446, #27610, #9906, #22675, #17223, #1555, #30514, #30863, #22848, #7527, #14834, #14670, #17912, #15007, #7179, #27956, #20288, #30694, #28304, #4960, #15347, #6837, #8353, #31194, #188, #10912, #5460, #15846, #33579, #23520, #10745, #13452, #8026, #21125, #10586, #343, #26235, #2579, #31357, #20633, #2906, #5775, #12794, #23845, #10421, #10258, #18245, #15515, #3063, #5127, #23683, #8193, #25738, #25906, #16012, #31034, #21289, #13127, #20963, #31523, #12965, #28962, #519, #26404, #7692, #23361, #31683, #18411, #23185, #2752, #24, #18075, #18741, #20793, #28803, #29127, #7860, #13291, #2409, #18578, #28634, #5289, #5620, #28470, #15682, #26083, #21786, #9186, #29802, #24182, #18900, #8837, #27238, #13953, #26905, #13787, #14122, #6109, #32348, #11232, #26560, #5946, #14287, #8677, #32177, #24013, #24690, #13616, #9012, #29295, #21959, #19401, #6463, #16337, #8506, #24516, #16506, #31842, #16170, #24344, #16844, #3733, #3892, #26731, #3392, #1349, #19239, #844, #21619, #32013, #19069, #1013, #3563, #29458, #677, #32513, #11408, #29634, #11736, #6281, #16674, #11079, #27071, #1173, #22123, #11570, #19575, #29968, #3229, #21460, #17182, #12241, #1514, #30475, #20423, #27405, #4741, #25026, #14455, #32852, #30136, #17693, #19740, #4580, #22808, #27565, #7316, #11911, #25354, #22297, #33199, #4232, #6626, #24851, #14630, #1851, #19902, #20080, #9862, #9344, #2024, #25183, #14966, #7137, #1679, #22627, #32678, #17520, #17011, #4067, #15133, #12072, #6794, #9515, #22460, #28080, #30301, #12412, #20244, #6969, #25528, #17357, #30648, #27743, #2197, #4406, #14791, #33015, #9686, #27909, #12579, #22972, #33371, #10046, #30816, #30994, #21083, #15303, #26366, #18206, #28597, #28762, #18033, #306, #28919, #31487, #12756, #7651, #5579, #26041, #17864, #7816, #5083, #2366, #8154, #15479, #5248, #23805, #28428, #18370, #15972, #23478, #15717, #25870, #5419, #15637, #7480, #23147, #2712, #477, #10705, #2536, #33535, #145, #18537, #13089, #10546, #12919, #15804, #20752, #13250, #23315, #28262, #20593, #3025, #10379, #20927, #4916, #13411, #25695, #23646, #10208, #2865, #10874, #31149, #31320, #7986, #26197, #21574, #3193, #21249, #29418, #14080, #8798, #8970, #11034, #13582, #21911, #24298, #23973, #16300, #635, #31803, #6068, #31966, #21416, #5738, #3854, #26690, #16462, #6418, #966, #11367, #29090, #19030, #6243, #19360, #3520, #16129, #29755, #18702, #24475, #8469, #27027, #1136, #11530, #18857, #29253, #19195, #8637, #5905, #31643, #26861, #32308, #29592, #16801, #3351, #13741, #27198, #21746, #24138, #805, #11195, #13913, #32136, #16631, #3687, #26521, #14246, #24645, #1311, #8310, #25141, #1805, #19535, #9474, #30436, #33159, #27703, #7096, #30260, #20036, #12202, #22254, #17313, #6582, #22589, #25483, #32469, #9822, #30089, #29929, #4189, #1472, #22766, #24811, #9641, #27862, #32641, #12370, #16966, #17477, #27361, #4535, #9304, #11700, #4027, #19696, #6922, #24986, #32975, #14927, #14418, #22083, #11867, #1979, #6755, #7269, #32807, #19862, #25315, #17142, #20203, #30603, #17651, #27528, #14585, #28039, #4365, #9137, #22417, #1637, #12029, #4700, #14748, #15090, #28881, #2322, #23439, #21043, #28560, #5044, #10162, #104, #10341, #2157, #28215, #7775, #5537, #15764, #20545, #4874, #5208, #13209, #33665, #12877, #33493, #10506, #25830, #18325, #30947, #12540, #25655, #272, #28387, #18166, #28720, #7612, #22930, #20382, #23105, #31113, #15434, #15594, #5376, #15263, #33325, #12709, #26159, #30774, #31446, #23270, #20713, #20885, #17996, #2825, #10667, #23608, #17817, #2494, #8114, #25996, #9996, #2666, #13049, #7436, #18496, #31283, #7943, #15927, #26484, #13874, #11496, #18994, #29213, #596, #24258, #763, #26325, #18658, #31927, #19324, #6203, #10992, #29048, #29384, #3648, #24096, #3312, #23934, #928, #16262, #8764, #21371, #2990, #16090, #24439, #18819, #8598, #432, #1103, #23767, #19152, #5702, #32101, #29549, #16592, #3153, #13540, #11326, #26648, #8270, #13370, #11162, #26984, #21710, #14043, #31767, #8433, #21874, #6030, #5865, #13696, #21537, #16422, #26818, #3482, #32266, #10834, #8934, #29713, #6375, #21209, #31603, #30229, #24609, #14548, #1768, #4497, #32770, #12168, #1604, #25107, #6884, #27326, #22382, #11664, #17274, #30565, #3820, #14888, #1434, #1271, #9270, #6548, #27827, #29894, #14714, #32945, #3991, #17443, #22048, #22560, #32431, #7061, #9606, #22216, #16931, #19833, #25281, #11995, #14388, #24778, #32605, #14212, #11830, #1946, #9098, #27663, #6721, #19494, #19664, #4330, #20001, #9443, #9784, #30054, #30400, #17112, #12334, #27496, #4151, #22731, #33119, #20168, #24947, #16766, #27164, #2460, #20684, #20510, #23573, #7228, #17782, #33630, #2796, #25619, #15559, #10634, #7578, #25450, #22896, #31247, #12670, #33458, #13016, #4840, #5340, #23233, #13177, #18126, #30913, #10308, #4671, #23408, #17964, #15055, #33289, #15731, #242, #26128, #21010, #20343, #25954, #7401, #28005, #2125, #17618, #20845, #28354, #2631, #7909, #12508, #15230, #12841, #9956, #2286, #30742, #28182, #23066, #10130, #5008, #71, #15397, #25795, #18290, #31082, #7741, #28524, #5173, #10471, #28679, #26288, #29640, #4073, #32185, #24189, #9019, #11243, #26912, #3570, #14461, #6469 ),
 ( #6633, #24858, #17019, #1521, #21628, #16852, #32021, #18462, #5504, #27413, #11742, #19245, #27245, #22129, #11917, #6117, #3741, #31407, #13959, #2961, #8685, #19076, #13795, #8077, #3899, #6287, #851, #32519, #15893, #29465, #28849, #16513, #24354, #19582, #1021, #16681, #11416, #8845, #21793, #19408, #27078, #14130, #24524, #1180, #14295, #11576, #21966, #32354, #29810, #24697, #1354, #9192, #29975, #22977, #20428, #9522, #12584, #14974, #4922, #1859, #33024, #19909, #20086, #2202, #33377, #28087, #27749, #12078, #25361, #10051, #7143, #30309, #32860, #4412, #9351, #6976, #30821, #19747, #12420, #12248, #6801, #17363, #22814, #33205, #4588, #15308, #25033, #17528, #22636, #15141, #14798, #25191, #4750, #17699, #25534, #9694, #7488, #17188, #27916, #2033, #30481, #25700, #22303, #9868, #20251, #17872, #30656, #7323, #2373, #28267, #27573, #4239, #32683, #30144, #14636, #1685, #22469, #10879, #28768, #18708, #23651, #2716, #5423, #10215, #18541, #23483, #20598, #28433, #5583, #15485, #28923, #15978, #26370, #12925, #5090, #10709, #13093, #25876, #12762, #20932, #3030, #310, #482, #2542, #23321, #13415, #15808, #11360, #7823, #10385, #20757, #31324, #149, #31155, #31000, #29094, #18211, #7990, #31647, #26201, #2869, #7656, #10553, #31492, #21254, #13255, #8159, #18376, #21090, #23810, #28602, #8314, #18039, #5742, #26527, #33540, #16134, #5253, #15646, #26046, #23152, #14251, #16305, #1141, #19365, #24143, #3858, #8472, #21916, #31807, #29759, #809, #3198, #21421, #11199, #32140, #16467, #16635, #6425, #5910, #13586, #3356, #27202, #18861, #32474, #24302, #973, #11534, #21578, #16806, #1316, #24650, #29259, #13747, #11704, #8802, #23979, #13917, #31973, #26694, #22089, #8643, #11372, #29933, #19034, #24479, #9143, #29598, #6072, #29423, #32312, #21751, #640, #26867, #19199, #6587, #19540, #3524, #6248, #27031, #16970, #3695, #14085, #8978, #11038, #17319, #9828, #22421, #4033, #17146, #25490, #19868, #9645, #1478, #2161, #24815, #6761, #27532, #9308, #33330, #33164, #25145, #19700, #17656, #11874, #22259, #12544, #4194, #10002, #15094, #32646, #1810, #20386, #27709, #30094, #4541, #14594, #32812, #9478, #30779, #1985, #7440, #27366, #12034, #22593, #24991, #14752, #14422, #20042, #28043, #22935, #1642, #4705, #30441, #30264, #6926, #4370, #12206, #32981, #7273, #7101, #20208, #17481, #27866, #14931, #25319, #12375, #22772, #30608, #33671, #4879, #28391, #18502, #15267, #7949, #7779, #2327, #5048, #18332, #28725, #109, #10842, #20549, #2674, #31117, #10671, #12882, #15440, #276, #13213, #21050, #28565, #31451, #12715, #13054, #31288, #18170, #439, #17820, #25836, #10511, #13375, #2498, #26162, #21215, #5213, #23109, #33497, #8120, #23275, #10346, #23611, #20717, #15932, #20890, #23773, #5383, #15599, #15769, #25659, #28887, #26002, #10169, #30956, #26330, #31609, #2996, #28222, #7616, #2829, #18000, #23444, #5542, #16771, #21879, #29390, #26992, #32273, #22053, #16270, #13880, #24615, #3319, #13547, #1275, #8940, #26656, #10998, #933, #19330, #6037, #19000, #5871, #6209, #31933, #24444, #13703, #18663, #31771, #6383, #770, #24263, #16095, #27170, #5707, #1108, #21377, #14048, #11501, #29720, #8438, #602, #16598, #8603, #23940, #8277, #16428, #3825, #29555, #14217, #18825, #29219, #11670, #11331, #24102, #11167, #21543, #26824, #3488, #21716, #32106, #26490, #29054, #8769, #19159, #3158, #3654, #17280, #6552, #11999, #12171, #27831, #19836, #22563, #32774, #1771, #27667, #11835, #30232, #16935, #4335, #9789, #19500, #4501, #19667, #27331, #17115, #1440, #17448, #24784, #25110, #32948, #22220, #14891, #3995, #9609, #14392, #20005, #9273, #32437, #32610, #30059, #6888, #14553, #14718, #30405, #6724, #9104, #27499, #25284, #4156, #33122, #9446, #7066, #1950, #24951, #12338, #22735, #29899, #1609, #22385, #27277, #24388, #16211, #6150, #3429, #714, #19438, #13825, #16544, #22160, #29337, #16712, #14331, #21824, #32055, #24217, #27114, #3598, #29163, #21494, #1056, #29842, #880, #26940, #32548, #5984, #3776, #24727, #32215, #8717, #11277, #14162, #13992, #5815, #31879, #11445, #9223, #9046, #21660, #8547, #8878, #6502, #19275, #29668, #26765, #24557, #19108, #11609, #29496, #26601, #18941, #3934, #6318, #1213, #3264, #1382, #13653, #21998, #16372, #32383, #16880, #11770, #24046, #11117, #12308, #23039, #14860, #4986, #20485, #15373, #25084, #20314, #12141, #32746, #19811, #30888, #25596, #33092, #30718, #2262, #25765, #19973, #17589, #28328, #7037, #17249, #1742, #22536, #27637, #17940, #17757, #9761, #4306, #12644, #30204, #6861, #7553, #32921, #11972, #33435, #14692, #20144, #22357, #22703, #9580, #22873, #30375, #17419, #27804, #9416, #7378, #4471, #25256, #1922, #7203, #30540, #27980, #4647, #15031, #10107, #25423, #2097, #12484, #33264, #9931, #28154, #4811, #15205, #214, #16036, #26427, #8214, #7886, #25930, #5481, #3090, #20986, #23385, #12991, #18267, #23210, #49, #13479, #33605, #26265, #26106, #20663, #10445, #5802, #21148, #2436, #10611, #28989, #23708, #23872, #2604, #28497, #544, #15870, #18102, #31222, #5150, #20819, #31382, #2773, #28656, #31057, #18768, #5315, #8052, #21312, #2933, #13316, #10284, #18436, #31546, #10936, #28825, #18602, #369, #10772, #5648, #15704, #31708, #7716, #8380, #16198, #15538, #29151, #13153, #23545, #12817, #16360, #3920, #5972, #24544, #9035, #13813, #27263, #31868, #11596, #21484 ),
 ( #29830, #24716, #16870, #8533, #3417, #1372, #21811, #13641, #3587, #869, #18928, #14318, #11265, #13980, #19602, #26754, #14148, #11760, #19264, #29483, #21647, #1198, #1042, #26588, #29324, #32203, #29994, #6491, #32042, #24206, #29657, #22148, #24376, #11434, #8705, #21985, #16532, #19427, #19095, #3253, #6138, #32536, #26929, #8865, #703, #9212, #24035, #6651, #6306, #32371, #11105, #16701, #27101, #3763, #9714, #20270, #17206, #17545, #20105, #20446, #2052, #17039, #25214, #9887, #4609, #4768, #6821, #9372, #17720, #30498, #32705, #12100, #19767, #27593, #1880, #17381, #4260, #1539, #33397, #22492, #12265, #2219, #7161, #27938, #24876, #14817, #12440, #15162, #33045, #22831, #22657, #25381, #14992, #14654, #33223, #11936, #30676, #30845, #4089, #25555, #1703, #22319, #9539, #25050, #28107, #30163, #7341, #12603, #32879, #22998, #19930, #10069, #30328, #27433, #6995, #14479, #27765, #4429, #2737, #20776, #20947, #326, #10241, #7509, #7675, #31508, #25721, #3047, #28619, #5271, #5444, #28452, #10727, #5603, #8176, #23171, #18057, #15996, #13111, #28287, #18229, #15502, #12780, #18561, #25892, #15665, #501, #5111, #28787, #26388, #169, #10403, #2561, #15829, #26067, #17893, #33562, #23502, #10895, #21109, #12949, #20619, #10569, #28946, #31341, #8009, #23344, #26219, #31173, #23666, #8, #4941, #31018, #13432, #7844, #18394, #15327, #23830, #2393, #21272, #2887, #13274, #24500, #3717, #29279, #29783, #13937, #3878, #8819, #21600, #24325, #29111, #14105, #5930, #31996, #8996, #828, #24671, #6448, #1335, #11062, #6266, #31826, #18727, #5760, #16829, #11552, #19052, #16657, #21940, #11722, #16322, #3545, #14271, #26713, #3215, #21444, #8492, #13601, #31668, #1159, #29442, #23997, #32330, #16153, #26544, #27223, #18884, #8336, #19385, #659, #6090, #3375, #8661, #13769, #19221, #24166, #11218, #16488, #26887, #27054, #996, #11393, #21770, #32159, #29618, #9500, #28066, #14776, #22793, #20230, #9329, #12397, #25168, #4727, #1663, #32835, #19721, #19886, #2008, #33185, #27891, #27551, #11896, #1836, #9848, #6950, #30118, #32664, #4214, #9167, #6780, #30632, #19560, #12226, #12055, #6608, #17165, #22614, #33001, #4390, #15117, #24835, #17341, #22444, #14953, #14614, #25010, #4565, #17504, #25339, #30284, #7300, #16992, #27729, #9669, #20062, #25512, #22108, #30461, #7121, #17678, #2181, #32495, #29952, #27387, #4051, #14442, #1499, #22281, #5069, #26183, #2851, #18353, #18020, #2350, #15622, #13236, #31135, #33518, #23131, #28411, #33354, #10193, #23632, #10028, #2697, #2519, #30801, #20575, #13074, #23464, #28583, #6016, #15287, #7800, #25856, #5406, #7637, #30978, #28747, #7969, #15790, #23299, #293, #7463, #18190, #26025, #12904, #29371, #12566, #15463, #5233, #8584, #28782, #20911, #16407, #10365, #17845, #28245, #10689, #20739, #130, #21070, #10531, #31912, #31306, #18978, #26801, #22958, #20408, #4901, #25682, #12740, #3807, #14528, #6356, #30210, #11978, #6867, #16578, #11811, #3631, #24245, #11311, #22363, #17094, #24592, #22199, #27479, #17256, #11479, #9081, #19817, #32249, #8749, #26969, #14025, #19138, #9423, #9255, #1252, #29533, #4136, #21696, #32087, #32752, #24424, #3464, #24929, #6189, #11649, #13860, #14196, #1088, #14371, #21857, #8917, #19309, #912, #32589, #29698, #16747, #27149, #32416, #22033, #19477, #29877, #6534, #1588, #16914, #27310, #3971, #24764, #1419, #19649, #30039, #6704, #25429, #22710, #9586, #4477, #2104, #27987, #27810, #12147, #10290, #33098, #12490, #12824, #7384, #17764, #1748, #22879, #12650, #15379, #9938, #23048, #33270, #2268, #28161, #14866, #20322, #22543, #4818, #7722, #14698, #25773, #12315, #32927, #20149, #17426, #4992, #7043, #25602, #10113, #25263, #28335, #19980, #33442, #30382, #20492, #1928, #27644, #9767, #30547, #30724, #7209, #15211, #30895, #17596, #4313, #4653, #17946, #15037, #23215, #7560, #2444, #33611, #20669, #31064, #25090, #8386, #55, #28662, #16206, #13323, #5156, #28831, #26112, #23391, #18774, #2780, #5488, #11113, #18273, #5655, #3260, #10779, #20992, #13160, #16042, #26271, #18108, #10451, #23714, #21491, #31714, #23551, #20825, #21155, #29157, #15877, #2940, #15711, #26433, #8059, #550, #221, #28504, #7892, #26596, #10617, #376, #25936, #13649, #15544, #10943, #31229, #23879, #21318, #5810, #5321, #18609, #31552, #31875, #3097, #2611, #8220, #24042, #13486, #710, #31389, #18443, #12997, #28995, #24213, #8712, #876, #14485, #14326, #6314, #11273, #32544, #26762, #3425, #27441, #21654, #24885, #30000, #13821, #16708, #1546, #8874, #32050, #19434, #19103, #3594, #13988, #11944, #16876, #22325, #8541, #26936, #3772, #29492, #29664, #18936, #1207, #9219, #6658, #6146, #19608, #11604, #29332, #21819, #19271, #16540, #27110, #22156, #17046, #24722, #24384, #1050, #21994, #4095, #14156, #11441, #32210, #24552, #5979, #32379, #16368, #9042, #29838, #6498, #27271, #3928, #1378, #11766, #14998, #25728, #1709, #17553, #12272, #25561, #27771, #30336, #15169, #28113, #2226, #9721, #12609, #27600, #27946, #12447, #22664, #15335, #32713, #9546, #25386, #28294, #17388, #7347, #2400, #33052, #17212, #14661, #23005, #4436, #25222, #4774, #7002, #30851, #2059, #4947, #9895, #20112, #22837, #30170, #33403, #14824, #30504, #10075, #1887, #12786, #7516, #9380, #12107, #17727, #32886, #19774, #6827, #17900, #20453, #7169, #4268, #25055, #22499, #4616, #33229, #19937, #20277 ),
 ( #30684, #2893, #14, #28794, #18062, #13280, #3220, #10248, #21279, #7850, #31024, #15671, #12956, #509, #2567, #21115, #5610, #10409, #23835, #28458, #8182, #5116, #16002, #20781, #23176, #7681, #31180, #18400, #2743, #23672, #26394, #25897, #33567, #23351, #13439, #15507, #18732, #10575, #20953, #31514, #18235, #3052, #31673, #10901, #28624, #5276, #8342, #5448, #20624, #176, #26073, #13117, #29117, #23508, #31347, #16158, #8014, #10732, #5765, #15835, #26224, #332, #18567, #28952, #26549, #5935, #19228, #6615, #27230, #21607, #16327, #6272, #24678, #11399, #24332, #11223, #11560, #3551, #29789, #8667, #24002, #3381, #11728, #6098, #29624, #21449, #22115, #11067, #6455, #26719, #19392, #16835, #3884, #13775, #14114, #16664, #17000, #32338, #13606, #21777, #14278, #1165, #1341, #24171, #834, #32502, #27060, #29284, #19058, #32002, #29448, #3724, #19566, #24507, #13944, #21948, #31832, #9175, #16495, #1004, #29959, #26894, #27393, #665, #8498, #32166, #9002, #8827, #18888, #11901, #12571, #17684, #25174, #22799, #28071, #17853, #12061, #9675, #20413, #32842, #9336, #17171, #4220, #19729, #10034, #9854, #1842, #30125, #4734, #22287, #32670, #22963, #27557, #30807, #25519, #6785, #12232, #7469, #4395, #14620, #14958, #25015, #9505, #19892, #4056, #12402, #14447, #24841, #22449, #33007, #1669, #22619, #1504, #30467, #15123, #2187, #30290, #33361, #7127, #6956, #17347, #14781, #27734, #20070, #17509, #27898, #20236, #4571, #25345, #2014, #33190, #30638, #7306, #5073, #10370, #15291, #15469, #28910, #25686, #18360, #18196, #12746, #25860, #28751, #5410, #10537, #21239, #30985, #13079, #7805, #21074, #23303, #2524, #10695, #23637, #31475, #5239, #8144, #23136, #23469, #7976, #28588, #10864, #28251, #12908, #20916, #23796, #26602, #2855, #31633, #15627, #33525, #10199, #18527, #20743, #31139, #296, #26029, #26357, #466, #31311, #5568, #3016, #2702, #15962, #15795, #8300, #135, #26186, #13240, #13400, #4906, #2355, #20580, #7641, #18024, #28416, #8961, #3512, #5895, #29245, #797, #5729, #16291, #19352, #16119, #8790, #8626, #3181, #26681, #19186, #29581, #958, #11694, #21407, #13904, #31958, #11522, #13730, #3342, #1128, #14069, #21903, #29410, #32300, #13573, #24288, #32128, #19022, #1304, #18691, #24129, #11355, #14239, #11186, #27017, #22075, #6060, #23964, #627, #29746, #21565, #16452, #24467, #26850, #16791, #21738, #24637, #6233, #16622, #3678, #26512, #6410, #27191, #3847, #32461, #29081, #11025, #31794, #8461, #18848, #17470, #9296, #29922, #16960, #17644, #22760, #30253, #27855, #33152, #22924, #17136, #14741, #25478, #4182, #14413, #22244, #19690, #24806, #15083, #14918, #6915, #1463, #9816, #27354, #4021, #28031, #32634, #2150, #30596, #11860, #17307, #12534, #9468, #30082, #20030, #6747, #14577, #24977, #9129, #4527, #19526, #6576, #27522, #4357, #1630, #27693, #20195, #12022, #25308, #22409, #1972, #32800, #19856, #25133, #1796, #12196, #22583, #32968, #12363, #9634, #30429, #7088, #7260, #4693, #28870, #20705, #31105, #31276, #20536, #2818, #31435, #23601, #15255, #10153, #8105, #28553, #20374, #10333, #7604, #4866, #266, #17987, #7767, #26316, #33485, #20877, #18487, #25987, #2486, #28379, #7936, #18158, #33317, #25648, #5199, #2983, #13201, #5036, #2315, #2658, #10660, #15584, #13041, #30941, #18316, #23262, #15755, #15426, #9987, #23096, #5528, #25822, #23432, #7426, #15918, #30767, #26151, #12700, #5368, #21034, #13363, #12868, #96, #10497, #17811, #28709, #28209, #33656, #16584, #11317, #11486, #13532, #16083, #24431, #26808, #5694, #18811, #26475, #588, #31918, #24087, #23923, #8260, #6362, #29204, #8590, #8924, #3472, #13865, #31594, #21529, #8755, #21864, #6022, #19143, #18987, #32093, #24251, #10983, #29377, #18650, #918, #3812, #10825, #32257, #8425, #29041, #16255, #21361, #1095, #3144, #21702, #6195, #31758, #5856, #26641, #26974, #29539, #3637, #755, #14033, #3303, #16413, #19315, #13687, #16757, #23758, #11155, #29704, #27156, #423, #21199, #18070, #14536, #32422, #29886, #4956, #19655, #6711, #19989, #11818, #12791, #30219, #20630, #25097, #4143, #6875, #11656, #30390, #22207, #24938, #25734, #17103, #7688, #23181, #28466, #27317, #22551, #14379, #1261, #22039, #33575, #28301, #1596, #32936, #15342, #14203, #32596, #19824, #31030, #9262, #19485, #3981, #24770, #6540, #24600, #7523, #11985, #16920, #2405, #9087, #1426, #10254, #30045, #27488, #22371, #32760, #9432, #17263, #27653, #4320, #1758, #14705, #12157, #9596, #17908, #13448, #11075, #8503, #23515, #339, #5285, #26230, #21456, #31519, #5771, #3225, #26079, #29124, #8189, #31838, #18407, #15842, #2749, #2902, #18738, #16167, #10908, #10582, #28630, #18574, #26556, #23679, #13123, #15678, #20960, #25903, #184, #13613, #2575, #28958, #28799, #23357, #31353, #5616, #16008, #21122, #18896, #7856, #10741, #5455, #31679, #26400, #3059, #5123, #18241, #23842, #13288, #8349, #8022, #515, #21285, #24009, #671, #15511, #12962, #20, #10417, #20788, #31190, #11908, #29291, #6104, #21954, #24847, #13949, #3888, #32675, #29630, #13783, #11228, #19571, #1009, #21782, #1345, #26901, #27401, #11565, #1511, #6459, #19235, #32344, #26727, #11732, #3559, #6277, #6622, #32173, #22293, #4063, #9341, #8673, #14282, #29454, #16333, #3387, #14452, #9182, #16670, #24686, #29964, #5942, #24340, #1170, #24179, #11404, #840, #19065, #16502, #21615, #32010, #22119 ),
 ( #32510, #8832, #27067, #3729, #24512, #14118, #9008, #19397, #29798, #17006, #16840, #27234, #10042, #12410, #2361, #33011, #30471, #17354, #17517, #33367, #20419, #25525, #25179, #9511, #22805, #30812, #4577, #6965, #30297, #1847, #6790, #27739, #7475, #17178, #9859, #9682, #4228, #4402, #20241, #7313, #27905, #19735, #12068, #25351, #12752, #17860, #14787, #22455, #33195, #28258, #14963, #7133, #12237, #17690, #20076, #2194, #22623, #30132, #19898, #4912, #2021, #30644, #27562, #15299, #14626, #12576, #32848, #22969, #25691, #23143, #28077, #4739, #15130, #33531, #25022, #1675, #18366, #3021, #31483, #31638, #20066, #2532, #10870, #13245, #25866, #5244, #12915, #20748, #28758, #10542, #10375, #28424, #26518, #15633, #5415, #29086, #23642, #302, #18029, #7982, #28915, #8306, #26193, #5575, #15800, #18533, #10701, #31145, #2861, #5078, #21079, #23969, #30990, #18697, #28594, #15475, #2707, #7811, #21245, #23311, #8150, #26362, #18202, #5734, #26037, #15967, #13085, #13407, #23474, #10204, #141, #20923, #23801, #31316, #473, #16125, #3189, #20589, #13578, #7647, #31799, #3683, #8633, #19026, #962, #26686, #8794, #16627, #29587, #18853, #16295, #27023, #6064, #11030, #29414, #3347, #8465, #6239, #13737, #31962, #24471, #24134, #24294, #14076, #26855, #11191, #801, #29249, #16458, #1132, #3516, #5901, #11362, #21570, #13909, #21742, #632, #32132, #21411, #19191, #15746, #26304, #31265, #18478, #3294, #23747, #31746, #29194, #18306, #21350, #412, #13678, #10649, #8094, #28698, #28861, #10973, #8416, #3134, #2809, #20864, #10815, #18802, #15907, #5358, #7926, #13190, #18145, #26141, #5846, #28543, #21188, #21024, #15574, #23589, #31585, #8250, #13354, #24076, #86, #2975, #31424, #23914, #256, #5517, #13521, #26465, #578, #18638, #16245, #25972, #29030, #5685, #16074, #745, #31096, #26632, #11145, #7755, #5189, #2647, #13030, #23422, #10485, #3459, #11803, #26965, #14020, #27305, #19134, #19643, #3803, #27473, #32409, #11475, #14192, #18973, #3966, #29528, #21853, #32581, #24419, #14521, #30032, #24922, #907, #29870, #21691, #8580, #29367, #6697, #1413, #8911, #6529, #22192, #1581, #6183, #27143, #4130, #16574, #26796, #11306, #32083, #13856, #21520, #14365, #19304, #24241, #9249, #6012, #16402, #17087, #8745, #31907, #3626, #1083, #24759, #32244, #29694, #6351, #22028, #24587, #16742, #16909, #1246, #11644, #9075, #19470, #24719, #27768, #4264, #1543, #4432, #9542, #17042, #14657, #19933, #9718, #3923, #11939, #12268, #1375, #1202, #9039, #29835, #11601, #1883, #1706, #27436, #21989, #30331, #14152, #24548, #14820, #19431, #22660, #17384, #32375, #4092, #33048, #29997, #6494, #6824, #16873, #11763, #22151, #29661, #25053, #6310, #16705, #14322, #24879, #27266, #14482, #27106, #22322, #6999, #25218, #32540, #3767, #32708, #9215, #19605, #6654, #9375, #19771, #30166, #17209, #12103, #27596, #22496, #32882, #10860, #4944, #7344, #30680, #2222, #7164, #17723, #21233, #17548, #10687, #10072, #4612, #28110, #21069, #31471, #2849, #13569, #22834, #15330, #33401, #13393, #15166, #4771, #3012, #15954, #23792, #30848, #461, #14995, #26180, #292, #20449, #3178, #20108, #25558, #13234, #16113, #12606, #28906, #23959, #7512, #25384, #2055, #31629, #23001, #17896, #26351, #28290, #18684, #23630, #26508, #8297, #12444, #8138, #621, #18523, #33226, #5562, #9890, #29074, #5724, #30501, #27942, #20273, #14410, #29406, #6228, #11182, #32122, #16955, #3673, #11690, #9125, #31953, #1299, #14066, #27350, #24280, #21734, #8622, #8786, #24634, #22072, #16787, #16448, #793, #24463, #32455, #29576, #19018, #21560, #26844, #31789, #6056, #19522, #8456, #1125, #953, #29239, #3508, #11518, #21899, #27012, #4016, #13723, #16617, #11351, #3843, #13900, #19181, #27188, #6405, #14235, #32296, #29918, #5890, #8957, #19347, #29740, #24803, #11021, #6571, #21400, #18844, #16287, #26676, #3338, #24123, #19685, #17133, #25473, #6910, #27690, #7256, #32795, #33312, #17466, #7422, #12359, #25128, #27851, #32630, #17640, #9465, #1791, #12531, #4353, #28204, #9982, #4863, #14573, #30250, #20370, #9812, #7084, #30764, #15077, #22580, #20191, #2146, #15251, #19853, #4523, #17807, #17303, #6743, #24973, #1627, #27519, #1459, #28026, #32965, #4177, #22920, #30079, #12017, #11855, #22403, #22241, #9291, #14738, #14913, #12192, #9628, #20025, #30426, #25304, #1968, #22755, #4691, #33148, #30590, #15914, #10150, #20531, #10821, #5032, #31591, #13360, #30937, #23429, #8256, #25981, #17983, #2815, #15422, #20702, #31101, #18645, #262, #29038, #5691, #10330, #20872, #25819, #13036, #25644, #18313, #26312, #23755, #12865, #2981, #28704, #2310, #5195, #2653, #23256, #92, #5523, #419, #31431, #7762, #2482, #5365, #21196, #10492, #33650, #18154, #28549, #12696, #15580, #23092, #33482, #15752, #31271, #7601, #7932, #26147, #13197, #23597, #28375, #10657, #21031, #8101, #18484, #28867, #13685, #32252, #11482, #19312, #26804, #8921, #10979, #11314, #29536, #29374, #32419, #16080, #26638, #8753, #11653, #752, #24427, #19480, #16410, #585, #31753, #6359, #21526, #8587, #21861, #24083, #14199, #32090, #29701, #16750, #27152, #3810, #16252, #16581, #19141, #29880, #1091, #26472, #24248, #24595, #3634, #1256, #21357, #22036, #9084, #6193, #8422, #11151, #18808, #3300, #31915, #18982, #6019, #3142, #3468, #13528, #23920, #26972, #13863, #29201, #915, #14028, #5853, #21699, #33273 ),
 ( #2107, #24932, #14869, #9941, #6871, #24767, #22202, #30550, #11981, #32755, #12318, #4139, #7212, #20152, #22366, #22546, #30214, #32930, #3975, #22713, #14531, #17259, #17599, #9426, #20325, #15040, #6537, #19652, #1591, #4656, #25266, #12150, #25432, #27990, #27647, #1931, #12493, #16917, #19820, #9589, #22882, #4316, #11814, #30042, #6707, #32592, #27313, #33102, #14701, #9258, #14376, #1422, #17099, #27483, #25093, #1751, #19984, #30385, #7046, #17429, #27813, #4480, #9770, #10116, #25776, #2447, #2943, #5324, #13326, #379, #15382, #25939, #30898, #18111, #23718, #23394, #31392, #28834, #17949, #20995, #58, #10782, #10292, #7725, #28339, #28507, #10621, #8062, #2783, #12827, #20495, #10454, #18446, #15547, #2614, #20828, #20672, #30727, #7386, #7563, #31233, #26274, #23218, #15714, #17767, #31067, #15214, #12653, #5491, #33614, #5159, #13163, #4995, #15880, #28164, #13000, #7895, #18276, #28665, #4821, #23554, #26115, #225, #25606, #2271, #23051, #33445, #14158, #552, #16209, #19273, #29494, #26764, #29666, #1052, #8543, #6148, #11443, #1211, #29159, #3427, #3774, #26598, #26435, #10945, #21320, #3100, #27112, #26938, #18938, #13488, #21822, #5657, #16044, #6316, #31716, #24554, #8876, #23881, #29335, #21158, #21493, #8388, #32052, #18776, #3262, #13651, #31555, #16542, #8222, #18611, #5812, #16370, #24044, #5981, #28997, #13823, #32212, #16710, #712, #11115, #24215, #31877, #878, #11275, #21656, #8715, #19105, #3596, #13990, #24386, #1380, #14663, #1889, #30172, #32546, #22158, #27444, #32381, #9221, #12274, #9044, #1711, #1548, #29840, #19610, #12110, #22501, #27602, #4618, #14329, #6830, #24887, #4438, #6661, #30002, #27773, #7004, #14827, #22327, #25224, #6500, #22666, #17048, #33055, #16878, #30338, #27273, #9723, #4097, #11606, #3931, #14487, #17214, #11946, #25057, #20114, #24724, #21996, #11768, #30506, #32715, #7171, #9382, #19776, #9548, #4270, #17556, #27948, #15000, #32888, #19940, #25388, #17390, #19436, #12787, #10077, #7349, #26074, #20455, #23177, #28795, #2228, #23352, #20954, #28460, #4950, #30853, #15, #10249, #2061, #28115, #7682, #5449, #15672, #7518, #4776, #5117, #13118, #33568, #20625, #33405, #10410, #25730, #18236, #17902, #12450, #25564, #178, #28296, #18064, #9897, #2744, #17729, #15336, #28625, #7851, #5278, #23509, #12611, #2568, #15508, #15836, #20783, #22839, #31025, #10577, #31183, #31348, #20280, #8016, #18401, #25898, #15171, #2401, #23008, #12957, #33231, #30686, #26395, #10734, #8828, #31674, #666, #11400, #5936, #16328, #333, #24003, #11224, #13945, #8499, #21609, #11069, #835, #26720, #3054, #31833, #21116, #3382, #6273, #13281, #24334, #10902, #31515, #18733, #16003, #3553, #5612, #24173, #18890, #21778, #21280, #32003, #29625, #26550, #8183, #18568, #16496, #8344, #29118, #8668, #23836, #26895, #6099, #5766, #29285, #16160, #13777, #23674, #19059, #510, #3221, #1005, #13607, #19230, #32167, #26225, #13441, #21450, #2895, #29449, #28953, #25175, #30291, #4057, #1671, #6958, #30468, #24680, #22289, #33008, #11729, #21950, #29792, #16836, #32339, #22620, #22450, #14448, #9003, #17348, #1166, #11561, #1844, #6456, #9677, #4397, #19393, #24842, #20071, #17001, #27231, #27558, #3885, #22116, #32503, #16666, #25016, #27062, #3725, #1342, #11902, #14279, #1505, #14115, #9337, #27735, #14783, #9177, #12233, #19730, #24508, #29960, #27395, #19567, #32671, #6616, #30127, #32843, #6786, #17172, #4222, #14621, #12062, #9506, #19893, #22964, #27900, #17685, #7806, #4573, #30986, #30808, #25346, #28072, #7642, #18025, #23138, #136, #9855, #25687, #20415, #26061, #2188, #4735, #23305, #2526, #10371, #17855, #20744, #2015, #2356, #20582, #7470, #23470, #7128, #15124, #10538, #7309, #28417, #26032, #33527, #10036, #25520, #5074, #15292, #17510, #33191, #12748, #20918, #31140, #12572, #20237, #10200, #18198, #4907, #28252, #33362, #15471, #25861, #28589, #12910, #14959, #30639, #5240, #15628, #2703, #12404, #13080, #22800, #26358, #13731, #3343, #24131, #798, #31477, #31795, #23965, #959, #16292, #31312, #5730, #11187, #18849, #8628, #15796, #21566, #31959, #628, #13241, #3017, #23638, #8145, #16120, #31634, #18528, #26187, #13905, #13401, #26513, #16453, #11026, #21408, #5411, #29082, #26682, #19023, #13574, #29411, #3183, #5897, #8462, #28911, #29246, #2856, #6061, #11357, #18361, #26851, #15963, #297, #23797, #21075, #3513, #10696, #24289, #7977, #5569, #28752, #468, #10865, #21240, #8301, #18692, #21739, #6234, #8962, #17432, #1756, #1934, #15044, #24468, #32129, #21904, #12496, #16624, #17771, #9593, #19987, #20156, #19353, #25436, #20330, #22885, #3679, #32301, #30730, #27816, #8791, #32934, #29748, #27018, #33277, #6411, #30388, #19187, #12323, #12155, #14071, #16793, #22717, #33107, #4484, #15218, #1129, #7051, #22549, #2112, #27192, #3848, #4660, #17603, #9944, #14875, #7390, #11523, #25269, #9773, #30554, #4827, #29582, #14240, #7216, #28168, #24638, #27994, #25609, #2274, #30901, #28343, #2949, #18115, #5163, #18451, #10298, #13330, #26278, #28513, #28669, #2617, #5327, #10119, #28838, #20674, #13005, #23721, #15550, #5661, #21161, #16049, #25783, #7729, #10786, #20999, #18280, #31558, #384, #61, #31397, #8225, #26439, #31071, #15719, #29001, #25943, #17953, #2450, #12830, #4998, #18614, #5494, #10458, #15386, #12658, #7567, #23222, #23056, #33617, #33448, #20500, #23398, #20833 ) ),
 .UNSPECIFIED., .T., .F., .T. ) 
 B_SPLINE_SURFACE_WITH_KNOTS ( ( 4, 3, 4 ),
 ( 3, 2, 2, 2, 2, 2, 2, 2, 2, 2, 2, 2, 2, 2, 2, 2, 2, 2, 2, 2, 2, 2, 2, 2, 2, 2, 2, 2, 2, 2, 2, 2, 2, 2, 2, 2, 2, 2, 2, 2, 2, 2, 2, 2, 2, 2, 2, 2, 2, 2, 2, 2, 2, 2, 2, 2, 2, 2, 2, 2, 2, 2, 2, 2, 2, 2, 2, 2, 2, 2, 2, 2, 2, 2, 2, 2, 2, 2, 2, 2, 2, 2, 2, 2, 2, 2, 2, 2, 2, 2, 2, 2, 2, 2, 2, 2, 2, 2, 2, 2, 2, 2, 2, 2, 2, 2, 2, 2, 2, 2, 2, 2, 2, 2, 2, 2, 2, 2, 2, 2, 2, 2, 2, 2, 2, 2, 2, 2, 2, 2, 2, 2, 2, 2, 2, 2, 2, 2, 2, 2, 2, 2, 2, 2, 2, 2, 2, 2, 2, 2, 2, 2, 2, 2, 2, 2, 2, 2, 2, 2, 2, 2, 2, 2, 2, 2, 2, 2, 2, 2, 2, 2, 2, 2, 2, 2, 2, 2, 2, 2, 2, 2, 2, 2, 2, 2, 2, 2, 2, 2, 2, 2, 2, 2, 2, 2, 2, 2, 2, 2, 2, 2, 2, 2, 2, 2, 2, 2, 2, 2, 2, 2, 2, 2, 2, 2, 2, 2, 2, 2, 2, 2, 2, 2, 2, 2, 2, 2, 2, 2, 2, 2, 2, 2, 2, 2, 2, 2, 2, 2, 2, 2, 2, 2, 2, 2, 2, 2, 2, 2, 2, 2, 2, 2, 2, 2, 2, 2, 2, 2, 2, 2, 2, 2, 2, 2, 2, 2, 2, 2, 2, 2, 2, 2, 2, 2, 2, 2, 2, 2, 2, 2, 2, 2, 2, 2, 2, 2, 2, 2, 2, 2, 2, 2, 2, 2, 2, 2, 2, 2, 2, 2, 2, 2, 2, 2, 2, 2, 2, 2, 2, 2, 2, 2, 2, 2, 2, 2, 2, 2, 2, 2, 2, 2, 2, 2, 2, 2, 2, 2, 2, 2, 2, 2, 2, 2, 2, 2, 2, 2, 2, 2, 2, 2, 2, 2, 3 ),
 ( 0.000000000000000000, 0.5000000000000000000, 1.000000000000000000 ),
 ( 0.000000000000000000, 0.002857142857142857140, 0.005714285714285714281, 0.008571428571428571855, 0.01142857142857142856, 0.01428571428571428527, 0.01714285714285714371, 0.02000000000000000042, 0.02285714285714285712, 0.02571428571428571383, 0.02857142857142857054, 0.03142857142857143071, 0.03428571428571428742, 0.03714285714285714413, 0.04000000000000000083, 0.04285714285714285754, 0.04571428571428571425, 0.04857142857142857095, 0.05142857142857142766, 0.05428571428571428437, 0.05714285714285714107, 0.05999999999999999778, 0.06285714285714286143, 0.06571428571428571119, 0.06857142857142857484, 0.07142857142857142461, 0.07428571428571428825, 0.07714285714285713802, 0.08000000000000000167, 0.08285714285714285143, 0.08571428571428571508, 0.08857142857142856485, 0.09142857142857142849, 0.09428571428571429214, 0.09714285714285714191, 0.1000000000000000056, 0.1028571428571428553, 0.1057142857142857190, 0.1085714285714285687, 0.1114285714285714324, 0.1142857142857142821, 0.1171428571428571458, 0.1199999999999999956, 0.1228571428571428592, 0.1257142857142857229, 0.1285714285714285587, 0.1314285714285714224, 0.1342857142857142860, 0.1371428571428571497, 0.1400000000000000133, 0.1428571428571428492, 0.1457142857142857129, 0.1485714285714285765, 0.1514285714285714401, 0.1542857142857142760, 0.1571428571428571397, 0.1600000000000000033, 0.1628571428571428670, 0.1657142857142857029, 0.1685714285714285665, 0.1714285714285714302, 0.1742857142857142938, 0.1771428571428571297, 0.1799999999999999933, 0.1828571428571428570, 0.1857142857142857206, 0.1885714285714285843, 0.1914285714285714202, 0.1942857142857142838, 0.1971428571428571475, 0.2000000000000000111, 0.2028571428571428470, 0.2057142857142857106, 0.2085714285714285743, 0.2114285714285714379, 0.2142857142857142738, 0.2171428571428571375, 0.2200000000000000011, 0.2228571428571428648, 0.2257142857142857006, 0.2285714285714285643, 0.2314285714285714279, 0.2342857142857142916, 0.2371428571428571552, 0.2399999999999999911, 0.2428571428571428548, 0.2457142857142857184, 0.2485714285714285821, 0.2514285714285714457, 0.2542857142857142816, 0.2571428571428571175, 0.2600000000000000089, 0.2628571428571428448, 0.2657142857142857362, 0.2685714285714285721, 0.2714285714285714080, 0.2742857142857142994, 0.2771428571428571352, 0.2800000000000000266, 0.2828571428571428625, 0.2857142857142856984, 0.2885714285714285898, 0.2914285714285714257, 0.2942857142857142616, 0.2971428571428571530, 0.2999999999999999889, 0.3028571428571428803, 0.3057142857142857162, 0.3085714285714285521, 0.3114285714285714435, 0.3142857142857142794, 0.3171428571428571153, 0.3200000000000000067, 0.3228571428571428426, 0.3257142857142857340, 0.3285714285714285698, 0.3314285714285714057, 0.3342857142857142971, 0.3371428571428571330, 0.3400000000000000244, 0.3428571428571428603, 0.3457142857142856962, 0.3485714285714285876, 0.3514285714285714235, 0.3542857142857142594, 0.3571428571428571508, 0.3599999999999999867, 0.3628571428571428781, 0.3657142857142857140, 0.3685714285714285499, 0.3714285714285714413, 0.3742857142857142771, 0.3771428571428571686, 0.3800000000000000044, 0.3828571428571428403, 0.3857142857142857317, 0.3885714285714285676, 0.3914285714285714035, 0.3942857142857142949, 0.3971428571428571308, 0.4000000000000000222, 0.4028571428571428581, 0.4057142857142856940, 0.4085714285714285854, 0.4114285714285714213, 0.4142857142857143127, 0.4171428571428571486, 0.4199999999999999845, 0.4228571428571428759, 0.4257142857142857117, 0.4285714285714285476, 0.4314285714285714390, 0.4342857142857142749, 0.4371428571428571663, 0.4400000000000000022, 0.4428571428571428381, 0.4457142857142857295, 0.4485714285714285654, 0.4514285714285714013, 0.4542857142857142927, 0.4571428571428571286, 0.4600000000000000200, 0.4628571428571428559, 0.4657142857142856918, 0.4685714285714285832, 0.4714285714285714191, 0.4742857142857143105, 0.4771428571428571463, 0.4799999999999999822, 0.4828571428571428736, 0.4857142857142857095, 0.4885714285714285454, 0.4914285714285714368, 0.4942857142857142727, 0.4971428571428571641, 0.5000000000000000000, 0.5028571428571428914, 0.5057142857142856718, 0.5085714285714285632, 0.5114285714285714546, 0.5142857142857142350, 0.5171428571428571264, 0.5200000000000000178, 0.5228571428571429092, 0.5257142857142856895, 0.5285714285714285809, 0.5314285714285714723, 0.5342857142857142527, 0.5371428571428571441, 0.5400000000000000355, 0.5428571428571428159, 0.5457142857142857073, 0.5485714285714285987, 0.5514285714285713791, 0.5542857142857142705, 0.5571428571428571619, 0.5600000000000000533, 0.5628571428571428337, 0.5657142857142857251, 0.5685714285714286165, 0.5714285714285713969, 0.5742857142857142883, 0.5771428571428571797, 0.5799999999999999600, 0.5828571428571428514, 0.5857142857142857428, 0.5885714285714285232, 0.5914285714285714146, 0.5942857142857143060, 0.5971428571428571974, 0.5999999999999999778, 0.6028571428571428692, 0.6057142857142857606, 0.6085714285714285410, 0.6114285714285714324, 0.6142857142857143238, 0.6171428571428571042, 0.6199999999999999956, 0.6228571428571428870, 0.6257142857142856673, 0.6285714285714285587, 0.6314285714285714501, 0.6342857142857142305, 0.6371428571428571219, 0.6400000000000000133, 0.6428571428571429047, 0.6457142857142856851, 0.6485714285714285765, 0.6514285714285714679, 0.6542857142857142483, 0.6571428571428571397, 0.6600000000000000311, 0.6628571428571428115, 0.6657142857142857029, 0.6685714285714285943, 0.6714285714285713746, 0.6742857142857142660, 0.6771428571428571574, 0.6800000000000000488, 0.6828571428571428292, 0.6857142857142857206, 0.6885714285714286120, 0.6914285714285713924, 0.6942857142857142838, 0.6971428571428571752, 0.6999999999999999556, 0.7028571428571428470, 0.7057142857142857384, 0.7085714285714285188, 0.7114285714285714102, 0.7142857142857143016, 0.7171428571428571930, 0.7199999999999999734, 0.7228571428571428648, 0.7257142857142857562, 0.7285714285714285365, 0.7314285714285714279, 0.7342857142857143193, 0.7371428571428570997, 0.7399999999999999911, 0.7428571428571428825, 0.7457142857142856629, 0.7485714285714285543, 0.7514285714285714457, 0.7542857142857143371, 0.7571428571428571175, 0.7600000000000000089, 0.7628571428571429003, 0.7657142857142856807, 0.7685714285714285721, 0.7714285714285714635, 0.7742857142857142438, 0.7771428571428571352, 0.7800000000000000266, 0.7828571428571428070, 0.7857142857142856984, 0.7885714285714285898, 0.7914285714285714812, 0.7942857142857142616, 0.7971428571428571530, 0.8000000000000000444, 0.8028571428571428248, 0.8057142857142857162, 0.8085714285714286076, 0.8114285714285713880, 0.8142857142857142794, 0.8171428571428571708, 0.8199999999999999512, 0.8228571428571428426, 0.8257142857142857340, 0.8285714285714286254, 0.8314285714285714057, 0.8342857142857142971, 0.8371428571428571885, 0.8399999999999999689, 0.8428571428571428603, 0.8457142857142857517, 0.8485714285714285321, 0.8514285714285714235, 0.8542857142857143149, 0.8571428571428570953, 0.8599999999999999867, 0.8628571428571428781, 0.8657142857142857695, 0.8685714285714285499, 0.8714285714285714413, 0.8742857142857143327, 0.8771428571428571130, 0.8800000000000000044, 0.8828571428571428958, 0.8857142857142856762, 0.8885714285714285676, 0.8914285714285714590, 0.8942857142857142394, 0.8971428571428571308, 0.9000000000000000222, 0.9028571428571428026, 0.9057142857142856940, 0.9085714285714285854, 0.9114285714285714768, 0.9142857142857142572, 0.9171428571428571486, 0.9200000000000000400, 0.9228571428571428203, 0.9257142857142857117, 0.9285714285714286031, 0.9314285714285713835, 0.9342857142857142749, 0.9371428571428571663, 0.9399999999999999467, 0.9428571428571428381, 0.9457142857142857295, 0.9485714285714286209, 0.9514285714285714013, 0.9542857142857142927, 0.9571428571428571841, 0.9599999999999999645, 0.9628571428571428559, 0.9657142857142857473, 0.9685714285714285277, 0.9714285714285714191, 0.9742857142857143105, 0.9771428571428570908, 0.9799999999999999822, 0.9828571428571428736, 0.9857142857142857650, 0.9955714285714286627 ),
 .UNSPECIFIED. ) 
 GEOMETRIC_REPRESENTATION_ITEM ( )  RATIONAL_B_SPLINE_SURFACE ( (
 ( 1.000000000000000000, 0.9510565162951535312, 1.000000000000000000, 0.9510565162951535312, 1.000000000000000000, 0.9510565162951535312, 1.000000000000000000, 0.9510565162951535312, 1.000000000000000000, 0.9510565162951535312, 1.000000000000000000, 0.9510565162951535312, 1.000000000000000000, 0.9510565162951535312, 1.000000000000000000, 0.9510565162951535312, 1.000000000000000000, 0.9510565162951535312, 1.000000000000000000, 0.9510565162951535312, 1.000000000000000000, 0.9510565162951535312, 1.000000000000000000, 0.9510565162951535312, 1.000000000000000000, 0.9510565162951535312, 1.000000000000000000, 0.9510565162951535312, 1.000000000000000000, 0.9510565162951535312, 1.000000000000000000, 0.9510565162951535312, 1.000000000000000000, 0.9510565162951535312, 1.000000000000000000, 0.9510565162951535312, 1.000000000000000000, 0.9510565162951535312, 1.000000000000000000, 0.9510565162951535312, 1.000000000000000000, 0.9510565162951535312, 1.000000000000000000, 0.9510565162951535312, 1.000000000000000000, 0.9510565162951535312, 1.000000000000000000, 0.9510565162951535312, 1.000000000000000000, 0.9510565162951535312, 1.000000000000000000, 0.9510565162951535312, 1.000000000000000000, 0.9510565162951535312, 1.000000000000000000, 0.9510565162951535312, 1.000000000000000000, 0.9510565162951535312, 1.000000000000000000, 0.9510565162951535312, 1.000000000000000000, 0.9510565162951535312, 1.000000000000000000, 0.9510565162951535312, 1.000000000000000000, 0.9510565162951535312, 1.000000000000000000, 0.9510565162951535312, 1.000000000000000000, 0.9510565162951535312, 1.000000000000000000, 0.9510565162951535312, 1.000000000000000000, 0.9510565162951535312, 1.000000000000000000, 0.9510565162951535312, 1.000000000000000000, 0.9510565162951535312, 1.000000000000000000, 0.9510565162951535312, 1.000000000000000000, 0.9510565162951535312, 1.000000000000000000, 0.9510565162951535312, 1.000000000000000000, 0.9510565162951535312, 1.000000000000000000, 0.9510565162951535312, 1.000000000000000000, 0.9510565162951535312, 1.000000000000000000, 0.9510565162951535312, 1.000000000000000000, 0.9510565162951535312, 1.000000000000000000, 0.9510565162951535312, 1.000000000000000000, 0.9510565162951535312, 1.000000000000000000, 0.9510565162951535312, 1.000000000000000000, 0.9510565162951535312, 1.000000000000000000, 0.9510565162951535312, 1.000000000000000000, 0.9510565162951535312, 1.000000000000000000, 0.9510565162951535312, 1.000000000000000000, 0.9510565162951535312, 1.000000000000000000, 0.9510565162951535312, 1.000000000000000000, 0.9510565162951535312, 1.000000000000000000, 0.9510565162951535312, 1.000000000000000000, 0.9510565162951535312, 1.000000000000000000, 0.9510565162951535312, 1.000000000000000000, 0.9510565162951535312, 1.000000000000000000, 0.9510565162951535312, 1.000000000000000000, 0.9510565162951535312, 1.000000000000000000, 0.9510565162951535312, 1.000000000000000000, 0.9510565162951535312, 1.000000000000000000, 0.9510565162951535312, 1.000000000000000000, 0.9510565162951535312, 1.000000000000000000, 0.9510565162951535312, 1.000000000000000000, 0.9510565162951535312, 1.000000000000000000, 0.9510565162951535312, 1.000000000000000000, 0.9510565162951535312, 1.000000000000000000, 0.9510565162951535312, 1.000000000000000000, 0.9510565162951535312, 1.000000000000000000, 0.9510565162951535312, 1.000000000000000000, 0.9510565162951535312, 1.000000000000000000, 0.9510565162951535312, 1.000000000000000000, 0.9510565162951535312, 1.000000000000000000, 0.9510565162951535312, 1.000000000000000000, 0.9510565162951535312, 1.000000000000000000, 0.9510565162951535312, 1.000000000000000000, 0.9510565162951535312, 1.000000000000000000, 0.9510565162951535312, 1.000000000000000000, 0.9510565162951535312, 1.000000000000000000, 0.9510565162951535312, 1.000000000000000000, 0.9510565162951535312, 1.000000000000000000, 0.9510565162951535312, 1.000000000000000000, 0.9510565162951535312, 1.000000000000000000, 0.9510565162951535312, 1.000000000000000000, 0.9510565162951535312, 1.000000000000000000, 0.9510565162951535312, 1.000000000000000000, 0.9510565162951535312, 1.000000000000000000, 0.9510565162951535312, 1.000000000000000000, 0.9510565162951535312, 1.000000000000000000, 0.9510565162951535312, 1.000000000000000000, 0.9510565162951535312, 1.000000000000000000, 0.9510565162951535312, 1.000000000000000000, 0.9510565162951535312, 1.000000000000000000, 0.9510565162951535312, 1.000000000000000000, 0.9510565162951535312, 1.000000000000000000, 0.9510565162951535312, 1.000000000000000000, 0.9510565162951535312, 1.000000000000000000, 0.9510565162951535312, 1.000000000000000000, 0.9510565162951535312, 1.000000000000000000, 0.9510565162951535312, 1.000000000000000000, 0.9510565162951535312, 1.000000000000000000, 0.9510565162951535312, 1.000000000000000000, 0.9510565162951535312, 1.000000000000000000, 0.9510565162951535312, 1.000000000000000000, 0.9510565162951535312, 1.000000000000000000, 0.9510565162951535312, 1.000000000000000000, 0.9510565162951535312, 1.000000000000000000, 0.9510565162951535312, 1.000000000000000000, 0.9510565162951535312, 1.000000000000000000, 0.9510565162951535312, 1.000000000000000000, 0.9510565162951535312, 1.000000000000000000, 0.9510565162951535312, 1.000000000000000000, 0.9510565162951535312, 1.000000000000000000, 0.9510565162951535312, 1.000000000000000000, 0.9510565162951535312, 1.000000000000000000, 0.9510565162951535312, 1.000000000000000000, 0.9510565162951535312, 1.000000000000000000, 0.9510565162951535312, 1.000000000000000000, 0.9510565162951535312, 1.000000000000000000, 0.9510565162951535312, 1.000000000000000000, 0.9510565162951535312, 1.000000000000000000, 0.9510565162951535312, 1.000000000000000000, 0.9510565162951535312, 1.000000000000000000, 0.9510565162951535312, 1.000000000000000000, 0.9510565162951535312, 1.000000000000000000, 0.9510565162951535312, 1.000000000000000000, 0.9510565162951535312, 1.000000000000000000, 0.9510565162951535312, 1.000000000000000000, 0.9510565162951535312, 1.000000000000000000, 0.9510565162951535312, 1.000000000000000000, 0.9510565162951535312, 1.000000000000000000, 0.9510565162951535312, 1.000000000000000000, 0.9510565162951535312, 1.000000000000000000, 0.9510565162951535312, 1.000000000000000000, 0.9510565162951535312, 1.000000000000000000, 0.9510565162951535312, 1.000000000000000000, 0.9510565162951535312, 1.000000000000000000, 0.9510565162951535312, 1.000000000000000000, 0.9510565162951535312, 1.000000000000000000, 0.9510565162951535312, 1.000000000000000000, 0.9510565162951535312, 1.000000000000000000, 0.9510565162951535312, 1.000000000000000000, 0.9510565162951535312, 1.000000000000000000, 0.9510565162951535312, 1.000000000000000000, 0.9510565162951535312, 1.000000000000000000, 0.9510565162951535312, 1.000000000000000000, 0.9510565162951535312, 1.000000000000000000, 0.9510565162951535312, 1.000000000000000000, 0.9510565162951535312, 1.000000000000000000, 0.9510565162951535312, 1.000000000000000000, 0.9510565162951535312, 1.000000000000000000, 0.9510565162951535312, 1.000000000000000000, 0.9510565162951535312, 1.000000000000000000, 0.9510565162951535312, 1.000000000000000000, 0.9510565162951535312, 1.000000000000000000, 0.9510565162951535312, 1.000000000000000000, 0.9510565162951535312, 1.000000000000000000, 0.9510565162951535312, 1.000000000000000000, 0.9510565162951535312, 1.000000000000000000, 0.9510565162951535312, 1.000000000000000000, 0.9510565162951535312, 1.000000000000000000, 0.9510565162951535312, 1.000000000000000000, 0.9510565162951535312, 1.000000000000000000, 0.9510565162951535312, 1.000000000000000000, 0.9510565162951535312, 1.000000000000000000, 0.9510565162951535312, 1.000000000000000000, 0.9510565162951535312, 1.000000000000000000, 0.9510565162951535312, 1.000000000000000000, 0.9510565162951535312, 1.000000000000000000, 0.9510565162951535312, 1.000000000000000000, 0.9510565162951535312, 1.000000000000000000, 0.9510565162951535312, 1.000000000000000000, 0.9510565162951535312, 1.000000000000000000, 0.9510565162951535312, 1.000000000000000000, 0.9510565162951535312, 1.000000000000000000, 0.9510565162951535312, 1.000000000000000000, 0.9510565162951535312, 1.000000000000000000, 0.9510565162951535312, 1.000000000000000000, 0.9510565162951535312, 1.000000000000000000, 0.9510565162951535312, 1.000000000000000000, 0.9510565162951535312, 1.000000000000000000, 0.9510565162951535312, 1.000000000000000000, 0.9510565162951535312, 1.000000000000000000, 0.9510565162951535312, 1.000000000000000000, 0.9510565162951535312, 1.000000000000000000, 0.9510565162951535312, 1.000000000000000000, 0.9510565162951535312, 1.000000000000000000, 0.9510565162951535312, 1.000000000000000000, 0.9510565162951535312, 1.000000000000000000, 0.9510565162951535312, 1.000000000000000000, 0.9510565162951535312, 1.000000000000000000, 0.9510565162951535312, 1.000000000000000000, 0.9510565162951535312, 1.000000000000000000, 0.9510565162951535312, 1.000000000000000000, 0.9510565162951535312, 1.000000000000000000, 0.9510565162951535312, 1.000000000000000000, 0.9510565162951535312, 1.000000000000000000, 0.9510565162951535312, 1.000000000000000000, 0.9510565162951535312, 1.000000000000000000, 0.9510565162951535312, 1.000000000000000000, 0.9510565162951535312, 1.000000000000000000, 0.9510565162951535312, 1.000000000000000000, 0.9510565162951535312, 1.000000000000000000, 0.9510565162951535312, 1.000000000000000000, 0.9510565162951535312, 1.000000000000000000, 0.9510565162951535312, 1.000000000000000000, 0.9510565162951535312, 1.000000000000000000, 0.9510565162951535312, 1.000000000000000000, 0.9510565162951535312, 1.000000000000000000, 0.9510565162951535312, 1.000000000000000000, 0.9510565162951535312, 1.000000000000000000, 0.9510565162951535312, 1.000000000000000000, 0.9510565162951535312, 1.000000000000000000, 0.9510565162951535312, 1.000000000000000000, 0.9510565162951535312, 1.000000000000000000, 0.9510565162951535312, 1.000000000000000000, 0.9510565162951535312, 1.000000000000000000, 0.9510565162951535312, 1.000000000000000000, 0.9510565162951535312, 1.000000000000000000, 0.9510565162951535312, 1.000000000000000000, 0.9510565162951535312, 1.000000000000000000, 0.9510565162951535312, 1.000000000000000000, 0.9510565162951535312, 1.000000000000000000, 0.9510565162951535312, 1.000000000000000000, 0.9510565162951535312, 1.000000000000000000, 0.9510565162951535312, 1.000000000000000000, 0.9510565162951535312, 1.000000000000000000, 0.9510565162951535312, 1.000000000000000000, 0.9510565162951535312, 1.000000000000000000, 0.9510565162951535312, 1.000000000000000000, 0.9510565162951535312, 1.000000000000000000, 0.9510565162951535312, 1.000000000000000000, 0.9510565162951535312, 1.000000000000000000, 0.9510565162951535312, 1.000000000000000000, 0.9510565162951535312, 1.000000000000000000, 0.9510565162951535312, 1.000000000000000000, 0.9510565162951535312, 1.000000000000000000, 0.9510565162951535312, 1.000000000000000000, 0.9510565162951535312, 1.000000000000000000, 0.9510565162951535312, 1.000000000000000000, 0.9510565162951535312, 1.000000000000000000, 0.9510565162951535312, 1.000000000000000000, 0.9510565162951535312, 1.000000000000000000, 0.9510565162951535312, 1.000000000000000000, 0.9510565162951535312, 1.000000000000000000, 0.9510565162951535312, 1.000000000000000000, 0.9510565162951535312, 1.000000000000000000, 0.9510565162951535312, 1.000000000000000000, 0.9510565162951535312, 1.000000000000000000, 0.9510565162951535312, 1.000000000000000000, 0.9510565162951535312, 1.000000000000000000, 0.9510565162951535312, 1.000000000000000000, 0.9510565162951535312, 1.000000000000000000, 0.9510565162951535312, 1.000000000000000000, 0.9510565162951535312, 1.000000000000000000, 0.9510565162951535312, 1.000000000000000000, 0.9510565162951535312, 1.000000000000000000, 0.9510565162951535312, 1.000000000000000000, 0.9510565162951535312, 1.000000000000000000, 0.9510565162951535312, 1.000000000000000000, 0.9510565162951535312, 1.000000000000000000, 0.9510565162951535312, 1.000000000000000000, 0.9510565162951535312, 1.000000000000000000, 0.9510565162951535312, 1.000000000000000000, 0.9510565162951535312, 1.000000000000000000, 0.9510565162951535312, 1.000000000000000000, 0.9510565162951535312, 1.000000000000000000, 0.9510565162951535312, 1.000000000000000000, 0.9510565162951535312, 1.000000000000000000, 0.9510565162951535312, 1.000000000000000000, 0.9510565162951535312, 1.000000000000000000, 0.9510565162951535312, 1.000000000000000000, 0.9510565162951535312, 1.000000000000000000, 0.9510565162951535312, 1.000000000000000000, 0.9510565162951535312, 1.000000000000000000, 0.9510565162951535312, 1.000000000000000000, 0.9510565162951535312, 1.000000000000000000, 0.9510565162951535312, 1.000000000000000000, 0.9510565162951535312, 1.000000000000000000, 0.9510565162951535312, 1.000000000000000000, 0.9510565162951535312, 1.000000000000000000, 0.9510565162951535312, 1.000000000000000000, 0.9510565162951535312, 1.000000000000000000, 0.9510565162951535312, 1.000000000000000000, 0.9510565162951535312, 1.000000000000000000, 0.9510565162951535312, 1.000000000000000000, 0.9510565162951535312, 1.000000000000000000, 0.9510565162951535312, 1.000000000000000000, 0.9510565162951535312, 1.000000000000000000, 0.9510565162951535312, 1.000000000000000000, 0.9510565162951535312, 1.000000000000000000, 0.9510565162951535312, 1.000000000000000000, 0.9510565162951535312, 1.000000000000000000, 0.9510565162951535312, 1.000000000000000000, 0.9510565162951535312, 1.000000000000000000, 0.9510565162951535312, 1.000000000000000000, 0.9510565162951535312, 1.000000000000000000, 0.9510565162951535312, 1.000000000000000000, 0.9510565162951535312, 1.000000000000000000, 0.9510565162951535312, 1.000000000000000000, 0.9510565162951535312, 1.000000000000000000, 0.9510565162951535312, 1.000000000000000000, 0.9510565162951535312, 1.000000000000000000, 0.9510565162951535312, 1.000000000000000000, 0.9510565162951535312, 1.000000000000000000, 0.9510565162951535312, 1.000000000000000000, 0.9510565162951535312, 1.000000000000000000, 0.9510565162951535312, 1.000000000000000000, 0.9510565162951535312, 1.000000000000000000, 0.9510565162951535312, 1.000000000000000000, 0.9510565162951535312, 1.000000000000000000, 0.9510565162951535312, 1.000000000000000000, 0.9510565162951535312, 1.000000000000000000, 0.9510565162951535312, 1.000000000000000000, 0.9510565162951535312, 1.000000000000000000, 0.9510565162951535312, 1.000000000000000000, 0.9510565162951535312, 1.000000000000000000, 0.9510565162951535312, 1.000000000000000000, 0.9510565162951535312, 1.000000000000000000, 0.9510565162951535312, 1.000000000000000000, 0.9510565162951535312, 1.000000000000000000, 0.9510565162951535312, 1.000000000000000000, 0.9510565162951535312, 1.000000000000000000, 0.9510565162951535312, 1.000000000000000000, 0.9510565162951535312, 1.000000000000000000, 0.9510565162951535312, 1.000000000000000000, 0.9510565162951535312, 1.000000000000000000, 0.9510565162951535312, 1.000000000000000000, 0.9510565162951535312, 1.000000000000000000, 0.9510565162951535312, 1.000000000000000000, 0.9510565162951535312, 1.000000000000000000, 0.9510565162951535312, 1.000000000000000000, 0.9510565162951535312, 1.000000000000000000, 0.9510565162951535312, 1.000000000000000000, 0.9510565162951535312, 1.000000000000000000, 0.9510565162951535312, 1.000000000000000000, 0.9510565162951535312, 1.000000000000000000, 0.9510565162951535312, 1.000000000000000000, 0.9510565162951535312, 1.000000000000000000, 0.9510565162951535312, 1.000000000000000000, 0.9510565162951535312, 1.000000000000000000, 1.000000000000000000, 1.000000000000000000),
 ( 0.3333333333333333703, 0.3170188387650512141, 0.3333333333333333703, 0.3170188387650512141, 0.3333333333333333703, 0.3170188387650512141, 0.3333333333333333703, 0.3170188387650512141, 0.3333333333333333703, 0.3170188387650512141, 0.3333333333333333703, 0.3170188387650512141, 0.3333333333333333703, 0.3170188387650512141, 0.3333333333333333703, 0.3170188387650512141, 0.3333333333333333703, 0.3170188387650512141, 0.3333333333333333703, 0.3170188387650512141, 0.3333333333333333703, 0.3170188387650512141, 0.3333333333333333703, 0.3170188387650512141, 0.3333333333333333703, 0.3170188387650512141, 0.3333333333333333703, 0.3170188387650512141, 0.3333333333333333703, 0.3170188387650512141, 0.3333333333333333703, 0.3170188387650512141, 0.3333333333333333703, 0.3170188387650512141, 0.3333333333333333703, 0.3170188387650512141, 0.3333333333333333703, 0.3170188387650512141, 0.3333333333333333703, 0.3170188387650512141, 0.3333333333333333703, 0.3170188387650512141, 0.3333333333333333703, 0.3170188387650512141, 0.3333333333333333703, 0.3170188387650512141, 0.3333333333333333703, 0.3170188387650512141, 0.3333333333333333703, 0.3170188387650512141, 0.3333333333333333703, 0.3170188387650512141, 0.3333333333333333703, 0.3170188387650512141, 0.3333333333333333703, 0.3170188387650512141, 0.3333333333333333703, 0.3170188387650512141, 0.3333333333333333703, 0.3170188387650512141, 0.3333333333333333703, 0.3170188387650512141, 0.3333333333333333703, 0.3170188387650512141, 0.3333333333333333703, 0.3170188387650512141, 0.3333333333333333703, 0.3170188387650512141, 0.3333333333333333703, 0.3170188387650512141, 0.3333333333333333703, 0.3170188387650512141, 0.3333333333333333703, 0.3170188387650512141, 0.3333333333333333703, 0.3170188387650512141, 0.3333333333333333703, 0.3170188387650512141, 0.3333333333333333703, 0.3170188387650512141, 0.3333333333333333703, 0.3170188387650512141, 0.3333333333333333703, 0.3170188387650512141, 0.3333333333333333703, 0.3170188387650512141, 0.3333333333333333703, 0.3170188387650512141, 0.3333333333333333703, 0.3170188387650512141, 0.3333333333333333703, 0.3170188387650512141, 0.3333333333333333703, 0.3170188387650512141, 0.3333333333333333703, 0.3170188387650512141, 0.3333333333333333703, 0.3170188387650512141, 0.3333333333333333703, 0.3170188387650512141, 0.3333333333333333703, 0.3170188387650512141, 0.3333333333333333703, 0.3170188387650512141, 0.3333333333333333703, 0.3170188387650512141, 0.3333333333333333703, 0.3170188387650512141, 0.3333333333333333703, 0.3170188387650512141, 0.3333333333333333703, 0.3170188387650512141, 0.3333333333333333703, 0.3170188387650512141, 0.3333333333333333703, 0.3170188387650512141, 0.3333333333333333703, 0.3170188387650512141, 0.3333333333333333703, 0.3170188387650512141, 0.3333333333333333703, 0.3170188387650512141, 0.3333333333333333703, 0.3170188387650512141, 0.3333333333333333703, 0.3170188387650512141, 0.3333333333333333703, 0.3170188387650512141, 0.3333333333333333703, 0.3170188387650512141, 0.3333333333333333703, 0.3170188387650512141, 0.3333333333333333703, 0.3170188387650512141, 0.3333333333333333703, 0.3170188387650512141, 0.3333333333333333703, 0.3170188387650512141, 0.3333333333333333703, 0.3170188387650512141, 0.3333333333333333703, 0.3170188387650512141, 0.3333333333333333703, 0.3170188387650512141, 0.3333333333333333703, 0.3170188387650512141, 0.3333333333333333703, 0.3170188387650512141, 0.3333333333333333703, 0.3170188387650512141, 0.3333333333333333703, 0.3170188387650512141, 0.3333333333333333703, 0.3170188387650512141, 0.3333333333333333703, 0.3170188387650512141, 0.3333333333333333703, 0.3170188387650512141, 0.3333333333333333703, 0.3170188387650512141, 0.3333333333333333703, 0.3170188387650512141, 0.3333333333333333703, 0.3170188387650512141, 0.3333333333333333703, 0.3170188387650512141, 0.3333333333333333703, 0.3170188387650512141, 0.3333333333333333703, 0.3170188387650512141, 0.3333333333333333703, 0.3170188387650512141, 0.3333333333333333703, 0.3170188387650512141, 0.3333333333333333703, 0.3170188387650512141, 0.3333333333333333703, 0.3170188387650512141, 0.3333333333333333703, 0.3170188387650512141, 0.3333333333333333703, 0.3170188387650512141, 0.3333333333333333703, 0.3170188387650512141, 0.3333333333333333703, 0.3170188387650512141, 0.3333333333333333703, 0.3170188387650512141, 0.3333333333333333703, 0.3170188387650512141, 0.3333333333333333703, 0.3170188387650512141, 0.3333333333333333703, 0.3170188387650512141, 0.3333333333333333703, 0.3170188387650512141, 0.3333333333333333703, 0.3170188387650512141, 0.3333333333333333703, 0.3170188387650512141, 0.3333333333333333703, 0.3170188387650512141, 0.3333333333333333703, 0.3170188387650512141, 0.3333333333333333703, 0.3170188387650512141, 0.3333333333333333703, 0.3170188387650512141, 0.3333333333333333703, 0.3170188387650512141, 0.3333333333333333703, 0.3170188387650512141, 0.3333333333333333703, 0.3170188387650512141, 0.3333333333333333703, 0.3170188387650512141, 0.3333333333333333703, 0.3170188387650512141, 0.3333333333333333703, 0.3170188387650512141, 0.3333333333333333703, 0.3170188387650512141, 0.3333333333333333703, 0.3170188387650512141, 0.3333333333333333703, 0.3170188387650512141, 0.3333333333333333703, 0.3170188387650512141, 0.3333333333333333703, 0.3170188387650512141, 0.3333333333333333703, 0.3170188387650512141, 0.3333333333333333703, 0.3170188387650512141, 0.3333333333333333703, 0.3170188387650512141, 0.3333333333333333703, 0.3170188387650512141, 0.3333333333333333703, 0.3170188387650512141, 0.3333333333333333703, 0.3170188387650512141, 0.3333333333333333703, 0.3170188387650512141, 0.3333333333333333703, 0.3170188387650512141, 0.3333333333333333703, 0.3170188387650512141, 0.3333333333333333703, 0.3170188387650512141, 0.3333333333333333703, 0.3170188387650512141, 0.3333333333333333703, 0.3170188387650512141, 0.3333333333333333703, 0.3170188387650512141, 0.3333333333333333703, 0.3170188387650512141, 0.3333333333333333703, 0.3170188387650512141, 0.3333333333333333703, 0.3170188387650512141, 0.3333333333333333703, 0.3170188387650512141, 0.3333333333333333703, 0.3170188387650512141, 0.3333333333333333703, 0.3170188387650512141, 0.3333333333333333703, 0.3170188387650512141, 0.3333333333333333703, 0.3170188387650512141, 0.3333333333333333703, 0.3170188387650512141, 0.3333333333333333703, 0.3170188387650512141, 0.3333333333333333703, 0.3170188387650512141, 0.3333333333333333703, 0.3170188387650512141, 0.3333333333333333703, 0.3170188387650512141, 0.3333333333333333703, 0.3170188387650512141, 0.3333333333333333703, 0.3170188387650512141, 0.3333333333333333703, 0.3170188387650512141, 0.3333333333333333703, 0.3170188387650512141, 0.3333333333333333703, 0.3170188387650512141, 0.3333333333333333703, 0.3170188387650512141, 0.3333333333333333703, 0.3170188387650512141, 0.3333333333333333703, 0.3170188387650512141, 0.3333333333333333703, 0.3170188387650512141, 0.3333333333333333703, 0.3170188387650512141, 0.3333333333333333703, 0.3170188387650512141, 0.3333333333333333703, 0.3170188387650512141, 0.3333333333333333703, 0.3170188387650512141, 0.3333333333333333703, 0.3170188387650512141, 0.3333333333333333703, 0.3170188387650512141, 0.3333333333333333703, 0.3170188387650512141, 0.3333333333333333703, 0.3170188387650512141, 0.3333333333333333703, 0.3170188387650512141, 0.3333333333333333703, 0.3170188387650512141, 0.3333333333333333703, 0.3170188387650512141, 0.3333333333333333703, 0.3170188387650512141, 0.3333333333333333703, 0.3170188387650512141, 0.3333333333333333703, 0.3170188387650512141, 0.3333333333333333703, 0.3170188387650512141, 0.3333333333333333703, 0.3170188387650512141, 0.3333333333333333703, 0.3170188387650512141, 0.3333333333333333703, 0.3170188387650512141, 0.3333333333333333703, 0.3170188387650512141, 0.3333333333333333703, 0.3170188387650512141, 0.3333333333333333703, 0.3170188387650512141, 0.3333333333333333703, 0.3170188387650512141, 0.3333333333333333703, 0.3170188387650512141, 0.3333333333333333703, 0.3170188387650512141, 0.3333333333333333703, 0.3170188387650512141, 0.3333333333333333703, 0.3170188387650512141, 0.3333333333333333703, 0.3170188387650512141, 0.3333333333333333703, 0.3170188387650512141, 0.3333333333333333703, 0.3170188387650512141, 0.3333333333333333703, 0.3170188387650512141, 0.3333333333333333703, 0.3170188387650512141, 0.3333333333333333703, 0.3170188387650512141, 0.3333333333333333703, 0.3170188387650512141, 0.3333333333333333703, 0.3170188387650512141, 0.3333333333333333703, 0.3170188387650512141, 0.3333333333333333703, 0.3170188387650512141, 0.3333333333333333703, 0.3170188387650512141, 0.3333333333333333703, 0.3170188387650512141, 0.3333333333333333703, 0.3170188387650512141, 0.3333333333333333703, 0.3170188387650512141, 0.3333333333333333703, 0.3170188387650512141, 0.3333333333333333703, 0.3170188387650512141, 0.3333333333333333703, 0.3170188387650512141, 0.3333333333333333703, 0.3170188387650512141, 0.3333333333333333703, 0.3170188387650512141, 0.3333333333333333703, 0.3170188387650512141, 0.3333333333333333703, 0.3170188387650512141, 0.3333333333333333703, 0.3170188387650512141, 0.3333333333333333703, 0.3170188387650512141, 0.3333333333333333703, 0.3170188387650512141, 0.3333333333333333703, 0.3170188387650512141, 0.3333333333333333703, 0.3170188387650512141, 0.3333333333333333703, 0.3170188387650512141, 0.3333333333333333703, 0.3170188387650512141, 0.3333333333333333703, 0.3170188387650512141, 0.3333333333333333703, 0.3170188387650512141, 0.3333333333333333703, 0.3170188387650512141, 0.3333333333333333703, 0.3170188387650512141, 0.3333333333333333703, 0.3170188387650512141, 0.3333333333333333703, 0.3170188387650512141, 0.3333333333333333703, 0.3170188387650512141, 0.3333333333333333703, 0.3170188387650512141, 0.3333333333333333703, 0.3170188387650512141, 0.3333333333333333703, 0.3170188387650512141, 0.3333333333333333703, 0.3170188387650512141, 0.3333333333333333703, 0.3170188387650512141, 0.3333333333333333703, 0.3170188387650512141, 0.3333333333333333703, 0.3170188387650512141, 0.3333333333333333703, 0.3170188387650512141, 0.3333333333333333703, 0.3170188387650512141, 0.3333333333333333703, 0.3170188387650512141, 0.3333333333333333703, 0.3170188387650512141, 0.3333333333333333703, 0.3170188387650512141, 0.3333333333333333703, 0.3170188387650512141, 0.3333333333333333703, 0.3170188387650512141, 0.3333333333333333703, 0.3170188387650512141, 0.3333333333333333703, 0.3170188387650512141, 0.3333333333333333703, 0.3170188387650512141, 0.3333333333333333703, 0.3170188387650512141, 0.3333333333333333703, 0.3170188387650512141, 0.3333333333333333703, 0.3170188387650512141, 0.3333333333333333703, 0.3170188387650512141, 0.3333333333333333703, 0.3170188387650512141, 0.3333333333333333703, 0.3170188387650512141, 0.3333333333333333703, 0.3170188387650512141, 0.3333333333333333703, 0.3170188387650512141, 0.3333333333333333703, 0.3170188387650512141, 0.3333333333333333703, 0.3170188387650512141, 0.3333333333333333703, 0.3170188387650512141, 0.3333333333333333703, 0.3170188387650512141, 0.3333333333333333703, 0.3170188387650512141, 0.3333333333333333703, 0.3170188387650512141, 0.3333333333333333703, 0.3170188387650512141, 0.3333333333333333703, 0.3170188387650512141, 0.3333333333333333703, 0.3170188387650512141, 0.3333333333333333703, 0.3170188387650512141, 0.3333333333333333703, 0.3170188387650512141, 0.3333333333333333703, 0.3170188387650512141, 0.3333333333333333703, 0.3170188387650512141, 0.3333333333333333703, 0.3170188387650512141, 0.3333333333333333703, 0.3170188387650512141, 0.3333333333333333703, 0.3170188387650512141, 0.3333333333333333703, 0.3170188387650512141, 0.3333333333333333703, 0.3170188387650512141, 0.3333333333333333703, 0.3170188387650512141, 0.3333333333333333703, 0.3170188387650512141, 0.3333333333333333703, 0.3170188387650512141, 0.3333333333333333703, 0.3170188387650512141, 0.3333333333333333703, 0.3170188387650512141, 0.3333333333333333703, 0.3170188387650512141, 0.3333333333333333703, 0.3170188387650512141, 0.3333333333333333703, 0.3170188387650512141, 0.3333333333333333703, 0.3170188387650512141, 0.3333333333333333703, 0.3170188387650512141, 0.3333333333333333703, 0.3170188387650512141, 0.3333333333333333703, 0.3170188387650512141, 0.3333333333333333703, 0.3170188387650512141, 0.3333333333333333703, 0.3170188387650512141, 0.3333333333333333703, 0.3170188387650512141, 0.3333333333333333703, 0.3170188387650512141, 0.3333333333333333703, 0.3170188387650512141, 0.3333333333333333703, 0.3170188387650512141, 0.3333333333333333703, 0.3170188387650512141, 0.3333333333333333703, 0.3170188387650512141, 0.3333333333333333703, 0.3170188387650512141, 0.3333333333333333703, 0.3170188387650512141, 0.3333333333333333703, 0.3170188387650512141, 0.3333333333333333703, 0.3170188387650512141, 0.3333333333333333703, 0.3170188387650512141, 0.3333333333333333703, 0.3170188387650512141, 0.3333333333333333703, 0.3170188387650512141, 0.3333333333333333703, 0.3170188387650512141, 0.3333333333333333703, 0.3170188387650512141, 0.3333333333333333703, 0.3170188387650512141, 0.3333333333333333703, 0.3170188387650512141, 0.3333333333333333703, 0.3170188387650512141, 0.3333333333333333703, 0.3170188387650512141, 0.3333333333333333703, 0.3170188387650512141, 0.3333333333333333703, 0.3170188387650512141, 0.3333333333333333703, 0.3170188387650512141, 0.3333333333333333703, 0.3170188387650512141, 0.3333333333333333703, 0.3170188387650512141, 0.3333333333333333703, 0.3170188387650512141, 0.3333333333333333703, 0.3170188387650512141, 0.3333333333333333703, 0.3170188387650512141, 0.3333333333333333703, 0.3170188387650512141, 0.3333333333333333703, 0.3170188387650512141, 0.3333333333333333703, 0.3170188387650512141, 0.3333333333333333703, 0.3170188387650512141, 0.3333333333333333703, 0.3170188387650512141, 0.3333333333333333703, 0.3170188387650512141, 0.3333333333333333703, 0.3170188387650512141, 0.3333333333333333703, 0.3170188387650512141, 0.3333333333333333703, 0.3170188387650512141, 0.3333333333333333703, 0.3170188387650512141, 0.3333333333333333703, 0.3170188387650512141, 0.3333333333333333703, 0.3170188387650512141, 0.3333333333333333703, 0.3170188387650512141, 0.3333333333333333703, 0.3170188387650512141, 0.3333333333333333703, 0.3170188387650512141, 0.3333333333333333703, 0.3170188387650512141, 0.3333333333333333703, 0.3170188387650512141, 0.3333333333333333703, 0.3170188387650512141, 0.3333333333333333703, 0.3170188387650512141, 0.3333333333333333703, 0.3170188387650512141, 0.3333333333333333703, 0.3170188387650512141, 0.3333333333333333703, 0.3170188387650512141, 0.3333333333333333703, 0.3170188387650512141, 0.3333333333333333703, 0.3170188387650512141, 0.3333333333333333703, 0.3170188387650512141, 0.3333333333333333703, 0.3170188387650512141, 0.3333333333333333703, 0.3170188387650512141, 0.3333333333333333703, 0.3170188387650512141, 0.3333333333333333703, 0.3170188387650512141, 0.3333333333333333703, 0.3170188387650512141, 0.3333333333333333703, 0.3170188387650512141, 0.3333333333333333703, 0.3170188387650512141, 0.3333333333333333703, 0.3170188387650512141, 0.3333333333333333703, 0.3170188387650512141, 0.3333333333333333703, 0.3170188387650512141, 0.3333333333333333703, 0.3170188387650512141, 0.3333333333333333703, 0.3170188387650512141, 0.3333333333333333703, 0.3170188387650512141, 0.3333333333333333703, 0.3170188387650512141, 0.3333333333333333703, 0.3170188387650512141, 0.3333333333333333703, 0.3170188387650512141, 0.3333333333333333703, 0.3170188387650512141, 0.3333333333333333703, 0.3170188387650512141, 0.3333333333333333703, 0.3170188387650512141, 0.3333333333333333703, 0.3170188387650512141, 0.3333333333333333703, 0.3170188387650512141, 0.3333333333333333703, 0.3170188387650512141, 0.3333333333333333703, 0.3170188387650512141, 0.3333333333333333703, 0.3170188387650512141, 0.3333333333333333703, 0.3170188387650512141, 0.3333333333333333703, 0.3333333333333333703, 0.3333333333333333703),
 ( 0.3333333333333333703, 0.3170188387650512141, 0.3333333333333333703, 0.3170188387650512141, 0.3333333333333333703, 0.3170188387650512141, 0.3333333333333333703, 0.3170188387650512141, 0.3333333333333333703, 0.3170188387650512141, 0.3333333333333333703, 0.3170188387650512141, 0.3333333333333333703, 0.3170188387650512141, 0.3333333333333333703, 0.3170188387650512141, 0.3333333333333333703, 0.3170188387650512141, 0.3333333333333333703, 0.3170188387650512141, 0.3333333333333333703, 0.3170188387650512141, 0.3333333333333333703, 0.3170188387650512141, 0.3333333333333333703, 0.3170188387650512141, 0.3333333333333333703, 0.3170188387650512141, 0.3333333333333333703, 0.3170188387650512141, 0.3333333333333333703, 0.3170188387650512141, 0.3333333333333333703, 0.3170188387650512141, 0.3333333333333333703, 0.3170188387650512141, 0.3333333333333333703, 0.3170188387650512141, 0.3333333333333333703, 0.3170188387650512141, 0.3333333333333333703, 0.3170188387650512141, 0.3333333333333333703, 0.3170188387650512141, 0.3333333333333333703, 0.3170188387650512141, 0.3333333333333333703, 0.3170188387650512141, 0.3333333333333333703, 0.3170188387650512141, 0.3333333333333333703, 0.3170188387650512141, 0.3333333333333333703, 0.3170188387650512141, 0.3333333333333333703, 0.3170188387650512141, 0.3333333333333333703, 0.3170188387650512141, 0.3333333333333333703, 0.3170188387650512141, 0.3333333333333333703, 0.3170188387650512141, 0.3333333333333333703, 0.3170188387650512141, 0.3333333333333333703, 0.3170188387650512141, 0.3333333333333333703, 0.3170188387650512141, 0.3333333333333333703, 0.3170188387650512141, 0.3333333333333333703, 0.3170188387650512141, 0.3333333333333333703, 0.3170188387650512141, 0.3333333333333333703, 0.3170188387650512141, 0.3333333333333333703, 0.3170188387650512141, 0.3333333333333333703, 0.3170188387650512141, 0.3333333333333333703, 0.3170188387650512141, 0.3333333333333333703, 0.3170188387650512141, 0.3333333333333333703, 0.3170188387650512141, 0.3333333333333333703, 0.3170188387650512141, 0.3333333333333333703, 0.3170188387650512141, 0.3333333333333333703, 0.3170188387650512141, 0.3333333333333333703, 0.3170188387650512141, 0.3333333333333333703, 0.3170188387650512141, 0.3333333333333333703, 0.3170188387650512141, 0.3333333333333333703, 0.3170188387650512141, 0.3333333333333333703, 0.3170188387650512141, 0.3333333333333333703, 0.3170188387650512141, 0.3333333333333333703, 0.3170188387650512141, 0.3333333333333333703, 0.3170188387650512141, 0.3333333333333333703, 0.3170188387650512141, 0.3333333333333333703, 0.3170188387650512141, 0.3333333333333333703, 0.3170188387650512141, 0.3333333333333333703, 0.3170188387650512141, 0.3333333333333333703, 0.3170188387650512141, 0.3333333333333333703, 0.3170188387650512141, 0.3333333333333333703, 0.3170188387650512141, 0.3333333333333333703, 0.3170188387650512141, 0.3333333333333333703, 0.3170188387650512141, 0.3333333333333333703, 0.3170188387650512141, 0.3333333333333333703, 0.3170188387650512141, 0.3333333333333333703, 0.3170188387650512141, 0.3333333333333333703, 0.3170188387650512141, 0.3333333333333333703, 0.3170188387650512141, 0.3333333333333333703, 0.3170188387650512141, 0.3333333333333333703, 0.3170188387650512141, 0.3333333333333333703, 0.3170188387650512141, 0.3333333333333333703, 0.3170188387650512141, 0.3333333333333333703, 0.3170188387650512141, 0.3333333333333333703, 0.3170188387650512141, 0.3333333333333333703, 0.3170188387650512141, 0.3333333333333333703, 0.3170188387650512141, 0.3333333333333333703, 0.3170188387650512141, 0.3333333333333333703, 0.3170188387650512141, 0.3333333333333333703, 0.3170188387650512141, 0.3333333333333333703, 0.3170188387650512141, 0.3333333333333333703, 0.3170188387650512141, 0.3333333333333333703, 0.3170188387650512141, 0.3333333333333333703, 0.3170188387650512141, 0.3333333333333333703, 0.3170188387650512141, 0.3333333333333333703, 0.3170188387650512141, 0.3333333333333333703, 0.3170188387650512141, 0.3333333333333333703, 0.3170188387650512141, 0.3333333333333333703, 0.3170188387650512141, 0.3333333333333333703, 0.3170188387650512141, 0.3333333333333333703, 0.3170188387650512141, 0.3333333333333333703, 0.3170188387650512141, 0.3333333333333333703, 0.3170188387650512141, 0.3333333333333333703, 0.3170188387650512141, 0.3333333333333333703, 0.3170188387650512141, 0.3333333333333333703, 0.3170188387650512141, 0.3333333333333333703, 0.3170188387650512141, 0.3333333333333333703, 0.3170188387650512141, 0.3333333333333333703, 0.3170188387650512141, 0.3333333333333333703, 0.3170188387650512141, 0.3333333333333333703, 0.3170188387650512141, 0.3333333333333333703, 0.3170188387650512141, 0.3333333333333333703, 0.3170188387650512141, 0.3333333333333333703, 0.3170188387650512141, 0.3333333333333333703, 0.3170188387650512141, 0.3333333333333333703, 0.3170188387650512141, 0.3333333333333333703, 0.3170188387650512141, 0.3333333333333333703, 0.3170188387650512141, 0.3333333333333333703, 0.3170188387650512141, 0.3333333333333333703, 0.3170188387650512141, 0.3333333333333333703, 0.3170188387650512141, 0.3333333333333333703, 0.3170188387650512141, 0.3333333333333333703, 0.3170188387650512141, 0.3333333333333333703, 0.3170188387650512141, 0.3333333333333333703, 0.3170188387650512141, 0.3333333333333333703, 0.3170188387650512141, 0.3333333333333333703, 0.3170188387650512141, 0.3333333333333333703, 0.3170188387650512141, 0.3333333333333333703, 0.3170188387650512141, 0.3333333333333333703, 0.3170188387650512141, 0.3333333333333333703, 0.3170188387650512141, 0.3333333333333333703, 0.3170188387650512141, 0.3333333333333333703, 0.3170188387650512141, 0.3333333333333333703, 0.3170188387650512141, 0.3333333333333333703, 0.3170188387650512141, 0.3333333333333333703, 0.3170188387650512141, 0.3333333333333333703, 0.3170188387650512141, 0.3333333333333333703, 0.3170188387650512141, 0.3333333333333333703, 0.3170188387650512141, 0.3333333333333333703, 0.3170188387650512141, 0.3333333333333333703, 0.3170188387650512141, 0.3333333333333333703, 0.3170188387650512141, 0.3333333333333333703, 0.3170188387650512141, 0.3333333333333333703, 0.3170188387650512141, 0.3333333333333333703, 0.3170188387650512141, 0.3333333333333333703, 0.3170188387650512141, 0.3333333333333333703, 0.3170188387650512141, 0.3333333333333333703, 0.3170188387650512141, 0.3333333333333333703, 0.3170188387650512141, 0.3333333333333333703, 0.3170188387650512141, 0.3333333333333333703, 0.3170188387650512141, 0.3333333333333333703, 0.3170188387650512141, 0.3333333333333333703, 0.3170188387650512141, 0.3333333333333333703, 0.3170188387650512141, 0.3333333333333333703, 0.3170188387650512141, 0.3333333333333333703, 0.3170188387650512141, 0.3333333333333333703, 0.3170188387650512141, 0.3333333333333333703, 0.3170188387650512141, 0.3333333333333333703, 0.3170188387650512141, 0.3333333333333333703, 0.3170188387650512141, 0.3333333333333333703, 0.3170188387650512141, 0.3333333333333333703, 0.3170188387650512141, 0.3333333333333333703, 0.3170188387650512141, 0.3333333333333333703, 0.3170188387650512141, 0.3333333333333333703, 0.3170188387650512141, 0.3333333333333333703, 0.3170188387650512141, 0.3333333333333333703, 0.3170188387650512141, 0.3333333333333333703, 0.3170188387650512141, 0.3333333333333333703, 0.3170188387650512141, 0.3333333333333333703, 0.3170188387650512141, 0.3333333333333333703, 0.3170188387650512141, 0.3333333333333333703, 0.3170188387650512141, 0.3333333333333333703, 0.3170188387650512141, 0.3333333333333333703, 0.3170188387650512141, 0.3333333333333333703, 0.3170188387650512141, 0.3333333333333333703, 0.3170188387650512141, 0.3333333333333333703, 0.3170188387650512141, 0.3333333333333333703, 0.3170188387650512141, 0.3333333333333333703, 0.3170188387650512141, 0.3333333333333333703, 0.3170188387650512141, 0.3333333333333333703, 0.3170188387650512141, 0.3333333333333333703, 0.3170188387650512141, 0.3333333333333333703, 0.3170188387650512141, 0.3333333333333333703, 0.3170188387650512141, 0.3333333333333333703, 0.3170188387650512141, 0.3333333333333333703, 0.3170188387650512141, 0.3333333333333333703, 0.3170188387650512141, 0.3333333333333333703, 0.3170188387650512141, 0.3333333333333333703, 0.3170188387650512141, 0.3333333333333333703, 0.3170188387650512141, 0.3333333333333333703, 0.3170188387650512141, 0.3333333333333333703, 0.3170188387650512141, 0.3333333333333333703, 0.3170188387650512141, 0.3333333333333333703, 0.3170188387650512141, 0.3333333333333333703, 0.3170188387650512141, 0.3333333333333333703, 0.3170188387650512141, 0.3333333333333333703, 0.3170188387650512141, 0.3333333333333333703, 0.3170188387650512141, 0.3333333333333333703, 0.3170188387650512141, 0.3333333333333333703, 0.3170188387650512141, 0.3333333333333333703, 0.3170188387650512141, 0.3333333333333333703, 0.3170188387650512141, 0.3333333333333333703, 0.3170188387650512141, 0.3333333333333333703, 0.3170188387650512141, 0.3333333333333333703, 0.3170188387650512141, 0.3333333333333333703, 0.3170188387650512141, 0.3333333333333333703, 0.3170188387650512141, 0.3333333333333333703, 0.3170188387650512141, 0.3333333333333333703, 0.3170188387650512141, 0.3333333333333333703, 0.3170188387650512141, 0.3333333333333333703, 0.3170188387650512141, 0.3333333333333333703, 0.3170188387650512141, 0.3333333333333333703, 0.3170188387650512141, 0.3333333333333333703, 0.3170188387650512141, 0.3333333333333333703, 0.3170188387650512141, 0.3333333333333333703, 0.3170188387650512141, 0.3333333333333333703, 0.3170188387650512141, 0.3333333333333333703, 0.3170188387650512141, 0.3333333333333333703, 0.3170188387650512141, 0.3333333333333333703, 0.3170188387650512141, 0.3333333333333333703, 0.3170188387650512141, 0.3333333333333333703, 0.3170188387650512141, 0.3333333333333333703, 0.3170188387650512141, 0.3333333333333333703, 0.3170188387650512141, 0.3333333333333333703, 0.3170188387650512141, 0.3333333333333333703, 0.3170188387650512141, 0.3333333333333333703, 0.3170188387650512141, 0.3333333333333333703, 0.3170188387650512141, 0.3333333333333333703, 0.3170188387650512141, 0.3333333333333333703, 0.3170188387650512141, 0.3333333333333333703, 0.3170188387650512141, 0.3333333333333333703, 0.3170188387650512141, 0.3333333333333333703, 0.3170188387650512141, 0.3333333333333333703, 0.3170188387650512141, 0.3333333333333333703, 0.3170188387650512141, 0.3333333333333333703, 0.3170188387650512141, 0.3333333333333333703, 0.3170188387650512141, 0.3333333333333333703, 0.3170188387650512141, 0.3333333333333333703, 0.3170188387650512141, 0.3333333333333333703, 0.3170188387650512141, 0.3333333333333333703, 0.3170188387650512141, 0.3333333333333333703, 0.3170188387650512141, 0.3333333333333333703, 0.3170188387650512141, 0.3333333333333333703, 0.3170188387650512141, 0.3333333333333333703, 0.3170188387650512141, 0.3333333333333333703, 0.3170188387650512141, 0.3333333333333333703, 0.3170188387650512141, 0.3333333333333333703, 0.3170188387650512141, 0.3333333333333333703, 0.3170188387650512141, 0.3333333333333333703, 0.3170188387650512141, 0.3333333333333333703, 0.3170188387650512141, 0.3333333333333333703, 0.3170188387650512141, 0.3333333333333333703, 0.3170188387650512141, 0.3333333333333333703, 0.3170188387650512141, 0.3333333333333333703, 0.3170188387650512141, 0.3333333333333333703, 0.3170188387650512141, 0.3333333333333333703, 0.3170188387650512141, 0.3333333333333333703, 0.3170188387650512141, 0.3333333333333333703, 0.3170188387650512141, 0.3333333333333333703, 0.3170188387650512141, 0.3333333333333333703, 0.3170188387650512141, 0.3333333333333333703, 0.3170188387650512141, 0.3333333333333333703, 0.3170188387650512141, 0.3333333333333333703, 0.3170188387650512141, 0.3333333333333333703, 0.3170188387650512141, 0.3333333333333333703, 0.3170188387650512141, 0.3333333333333333703, 0.3170188387650512141, 0.3333333333333333703, 0.3170188387650512141, 0.3333333333333333703, 0.3170188387650512141, 0.3333333333333333703, 0.3170188387650512141, 0.3333333333333333703, 0.3170188387650512141, 0.3333333333333333703, 0.3170188387650512141, 0.3333333333333333703, 0.3170188387650512141, 0.3333333333333333703, 0.3170188387650512141, 0.3333333333333333703, 0.3170188387650512141, 0.3333333333333333703, 0.3170188387650512141, 0.3333333333333333703, 0.3170188387650512141, 0.3333333333333333703, 0.3170188387650512141, 0.3333333333333333703, 0.3170188387650512141, 0.3333333333333333703, 0.3170188387650512141, 0.3333333333333333703, 0.3170188387650512141, 0.3333333333333333703, 0.3170188387650512141, 0.3333333333333333703, 0.3170188387650512141, 0.3333333333333333703, 0.3170188387650512141, 0.3333333333333333703, 0.3170188387650512141, 0.3333333333333333703, 0.3170188387650512141, 0.3333333333333333703, 0.3170188387650512141, 0.3333333333333333703, 0.3170188387650512141, 0.3333333333333333703, 0.3170188387650512141, 0.3333333333333333703, 0.3170188387650512141, 0.3333333333333333703, 0.3170188387650512141, 0.3333333333333333703, 0.3170188387650512141, 0.3333333333333333703, 0.3170188387650512141, 0.3333333333333333703, 0.3170188387650512141, 0.3333333333333333703, 0.3170188387650512141, 0.3333333333333333703, 0.3170188387650512141, 0.3333333333333333703, 0.3170188387650512141, 0.3333333333333333703, 0.3170188387650512141, 0.3333333333333333703, 0.3170188387650512141, 0.3333333333333333703, 0.3170188387650512141, 0.3333333333333333703, 0.3170188387650512141, 0.3333333333333333703, 0.3170188387650512141, 0.3333333333333333703, 0.3170188387650512141, 0.3333333333333333703, 0.3170188387650512141, 0.3333333333333333703, 0.3170188387650512141, 0.3333333333333333703, 0.3170188387650512141, 0.3333333333333333703, 0.3170188387650512141, 0.3333333333333333703, 0.3170188387650512141, 0.3333333333333333703, 0.3170188387650512141, 0.3333333333333333703, 0.3170188387650512141, 0.3333333333333333703, 0.3170188387650512141, 0.3333333333333333703, 0.3170188387650512141, 0.3333333333333333703, 0.3170188387650512141, 0.3333333333333333703, 0.3170188387650512141, 0.3333333333333333703, 0.3170188387650512141, 0.3333333333333333703, 0.3170188387650512141, 0.3333333333333333703, 0.3170188387650512141, 0.3333333333333333703, 0.3170188387650512141, 0.3333333333333333703, 0.3170188387650512141, 0.3333333333333333703, 0.3170188387650512141, 0.3333333333333333703, 0.3170188387650512141, 0.3333333333333333703, 0.3170188387650512141, 0.3333333333333333703, 0.3170188387650512141, 0.3333333333333333703, 0.3170188387650512141, 0.3333333333333333703, 0.3170188387650512141, 0.3333333333333333703, 0.3170188387650512141, 0.3333333333333333703, 0.3170188387650512141, 0.3333333333333333703, 0.3170188387650512141, 0.3333333333333333703, 0.3170188387650512141, 0.3333333333333333703, 0.3170188387650512141, 0.3333333333333333703, 0.3170188387650512141, 0.3333333333333333703, 0.3170188387650512141, 0.3333333333333333703, 0.3170188387650512141, 0.3333333333333333703, 0.3170188387650512141, 0.3333333333333333703, 0.3170188387650512141, 0.3333333333333333703, 0.3170188387650512141, 0.3333333333333333703, 0.3170188387650512141, 0.3333333333333333703, 0.3170188387650512141, 0.3333333333333333703, 0.3170188387650512141, 0.3333333333333333703, 0.3170188387650512141, 0.3333333333333333703, 0.3170188387650512141, 0.3333333333333333703, 0.3170188387650512141, 0.3333333333333333703, 0.3170188387650512141, 0.3333333333333333703, 0.3170188387650512141, 0.3333333333333333703, 0.3170188387650512141, 0.3333333333333333703, 0.3170188387650512141, 0.3333333333333333703, 0.3170188387650512141, 0.3333333333333333703, 0.3170188387650512141, 0.3333333333333333703, 0.3170188387650512141, 0.3333333333333333703, 0.3170188387650512141, 0.3333333333333333703, 0.3170188387650512141, 0.3333333333333333703, 0.3170188387650512141, 0.3333333333333333703, 0.3170188387650512141, 0.3333333333333333703, 0.3170188387650512141, 0.3333333333333333703, 0.3170188387650512141, 0.3333333333333333703, 0.3170188387650512141, 0.3333333333333333703, 0.3333333333333333703, 0.3333333333333333703),
 ( 1.000000000000000000, 0.9510565162951535312, 1.000000000000000000, 0.9510565162951535312, 1.000000000000000000, 0.9510565162951535312, 1.000000000000000000, 0.9510565162951535312, 1.000000000000000000, 0.9510565162951535312, 1.000000000000000000, 0.9510565162951535312, 1.000000000000000000, 0.9510565162951535312, 1.000000000000000000, 0.9510565162951535312, 1.000000000000000000, 0.9510565162951535312, 1.000000000000000000, 0.9510565162951535312, 1.000000000000000000, 0.9510565162951535312, 1.000000000000000000, 0.9510565162951535312, 1.000000000000000000, 0.9510565162951535312, 1.000000000000000000, 0.9510565162951535312, 1.000000000000000000, 0.9510565162951535312, 1.000000000000000000, 0.9510565162951535312, 1.000000000000000000, 0.9510565162951535312, 1.000000000000000000, 0.9510565162951535312, 1.000000000000000000, 0.9510565162951535312, 1.000000000000000000, 0.9510565162951535312, 1.000000000000000000, 0.9510565162951535312, 1.000000000000000000, 0.9510565162951535312, 1.000000000000000000, 0.9510565162951535312, 1.000000000000000000, 0.9510565162951535312, 1.000000000000000000, 0.9510565162951535312, 1.000000000000000000, 0.9510565162951535312, 1.000000000000000000, 0.9510565162951535312, 1.000000000000000000, 0.9510565162951535312, 1.000000000000000000, 0.9510565162951535312, 1.000000000000000000, 0.9510565162951535312, 1.000000000000000000, 0.9510565162951535312, 1.000000000000000000, 0.9510565162951535312, 1.000000000000000000, 0.9510565162951535312, 1.000000000000000000, 0.9510565162951535312, 1.000000000000000000, 0.9510565162951535312, 1.000000000000000000, 0.9510565162951535312, 1.000000000000000000, 0.9510565162951535312, 1.000000000000000000, 0.9510565162951535312, 1.000000000000000000, 0.9510565162951535312, 1.000000000000000000, 0.9510565162951535312, 1.000000000000000000, 0.9510565162951535312, 1.000000000000000000, 0.9510565162951535312, 1.000000000000000000, 0.9510565162951535312, 1.000000000000000000, 0.9510565162951535312, 1.000000000000000000, 0.9510565162951535312, 1.000000000000000000, 0.9510565162951535312, 1.000000000000000000, 0.9510565162951535312, 1.000000000000000000, 0.9510565162951535312, 1.000000000000000000, 0.9510565162951535312, 1.000000000000000000, 0.9510565162951535312, 1.000000000000000000, 0.9510565162951535312, 1.000000000000000000, 0.9510565162951535312, 1.000000000000000000, 0.9510565162951535312, 1.000000000000000000, 0.9510565162951535312, 1.000000000000000000, 0.9510565162951535312, 1.000000000000000000, 0.9510565162951535312, 1.000000000000000000, 0.9510565162951535312, 1.000000000000000000, 0.9510565162951535312, 1.000000000000000000, 0.9510565162951535312, 1.000000000000000000, 0.9510565162951535312, 1.000000000000000000, 0.9510565162951535312, 1.000000000000000000, 0.9510565162951535312, 1.000000000000000000, 0.9510565162951535312, 1.000000000000000000, 0.9510565162951535312, 1.000000000000000000, 0.9510565162951535312, 1.000000000000000000, 0.9510565162951535312, 1.000000000000000000, 0.9510565162951535312, 1.000000000000000000, 0.9510565162951535312, 1.000000000000000000, 0.9510565162951535312, 1.000000000000000000, 0.9510565162951535312, 1.000000000000000000, 0.9510565162951535312, 1.000000000000000000, 0.9510565162951535312, 1.000000000000000000, 0.9510565162951535312, 1.000000000000000000, 0.9510565162951535312, 1.000000000000000000, 0.9510565162951535312, 1.000000000000000000, 0.9510565162951535312, 1.000000000000000000, 0.9510565162951535312, 1.000000000000000000, 0.9510565162951535312, 1.000000000000000000, 0.9510565162951535312, 1.000000000000000000, 0.9510565162951535312, 1.000000000000000000, 0.9510565162951535312, 1.000000000000000000, 0.9510565162951535312, 1.000000000000000000, 0.9510565162951535312, 1.000000000000000000, 0.9510565162951535312, 1.000000000000000000, 0.9510565162951535312, 1.000000000000000000, 0.9510565162951535312, 1.000000000000000000, 0.9510565162951535312, 1.000000000000000000, 0.9510565162951535312, 1.000000000000000000, 0.9510565162951535312, 1.000000000000000000, 0.9510565162951535312, 1.000000000000000000, 0.9510565162951535312, 1.000000000000000000, 0.9510565162951535312, 1.000000000000000000, 0.9510565162951535312, 1.000000000000000000, 0.9510565162951535312, 1.000000000000000000, 0.9510565162951535312, 1.000000000000000000, 0.9510565162951535312, 1.000000000000000000, 0.9510565162951535312, 1.000000000000000000, 0.9510565162951535312, 1.000000000000000000, 0.9510565162951535312, 1.000000000000000000, 0.9510565162951535312, 1.000000000000000000, 0.9510565162951535312, 1.000000000000000000, 0.9510565162951535312, 1.000000000000000000, 0.9510565162951535312, 1.000000000000000000, 0.9510565162951535312, 1.000000000000000000, 0.9510565162951535312, 1.000000000000000000, 0.9510565162951535312, 1.000000000000000000, 0.9510565162951535312, 1.000000000000000000, 0.9510565162951535312, 1.000000000000000000, 0.9510565162951535312, 1.000000000000000000, 0.9510565162951535312, 1.000000000000000000, 0.9510565162951535312, 1.000000000000000000, 0.9510565162951535312, 1.000000000000000000, 0.9510565162951535312, 1.000000000000000000, 0.9510565162951535312, 1.000000000000000000, 0.9510565162951535312, 1.000000000000000000, 0.9510565162951535312, 1.000000000000000000, 0.9510565162951535312, 1.000000000000000000, 0.9510565162951535312, 1.000000000000000000, 0.9510565162951535312, 1.000000000000000000, 0.9510565162951535312, 1.000000000000000000, 0.9510565162951535312, 1.000000000000000000, 0.9510565162951535312, 1.000000000000000000, 0.9510565162951535312, 1.000000000000000000, 0.9510565162951535312, 1.000000000000000000, 0.9510565162951535312, 1.000000000000000000, 0.9510565162951535312, 1.000000000000000000, 0.9510565162951535312, 1.000000000000000000, 0.9510565162951535312, 1.000000000000000000, 0.9510565162951535312, 1.000000000000000000, 0.9510565162951535312, 1.000000000000000000, 0.9510565162951535312, 1.000000000000000000, 0.9510565162951535312, 1.000000000000000000, 0.9510565162951535312, 1.000000000000000000, 0.9510565162951535312, 1.000000000000000000, 0.9510565162951535312, 1.000000000000000000, 0.9510565162951535312, 1.000000000000000000, 0.9510565162951535312, 1.000000000000000000, 0.9510565162951535312, 1.000000000000000000, 0.9510565162951535312, 1.000000000000000000, 0.9510565162951535312, 1.000000000000000000, 0.9510565162951535312, 1.000000000000000000, 0.9510565162951535312, 1.000000000000000000, 0.9510565162951535312, 1.000000000000000000, 0.9510565162951535312, 1.000000000000000000, 0.9510565162951535312, 1.000000000000000000, 0.9510565162951535312, 1.000000000000000000, 0.9510565162951535312, 1.000000000000000000, 0.9510565162951535312, 1.000000000000000000, 0.9510565162951535312, 1.000000000000000000, 0.9510565162951535312, 1.000000000000000000, 0.9510565162951535312, 1.000000000000000000, 0.9510565162951535312, 1.000000000000000000, 0.9510565162951535312, 1.000000000000000000, 0.9510565162951535312, 1.000000000000000000, 0.9510565162951535312, 1.000000000000000000, 0.9510565162951535312, 1.000000000000000000, 0.9510565162951535312, 1.000000000000000000, 0.9510565162951535312, 1.000000000000000000, 0.9510565162951535312, 1.000000000000000000, 0.9510565162951535312, 1.000000000000000000, 0.9510565162951535312, 1.000000000000000000, 0.9510565162951535312, 1.000000000000000000, 0.9510565162951535312, 1.000000000000000000, 0.9510565162951535312, 1.000000000000000000, 0.9510565162951535312, 1.000000000000000000, 0.9510565162951535312, 1.000000000000000000, 0.9510565162951535312, 1.000000000000000000, 0.9510565162951535312, 1.000000000000000000, 0.9510565162951535312, 1.000000000000000000, 0.9510565162951535312, 1.000000000000000000, 0.9510565162951535312, 1.000000000000000000, 0.9510565162951535312, 1.000000000000000000, 0.9510565162951535312, 1.000000000000000000, 0.9510565162951535312, 1.000000000000000000, 0.9510565162951535312, 1.000000000000000000, 0.9510565162951535312, 1.000000000000000000, 0.9510565162951535312, 1.000000000000000000, 0.9510565162951535312, 1.000000000000000000, 0.9510565162951535312, 1.000000000000000000, 0.9510565162951535312, 1.000000000000000000, 0.9510565162951535312, 1.000000000000000000, 0.9510565162951535312, 1.000000000000000000, 0.9510565162951535312, 1.000000000000000000, 0.9510565162951535312, 1.000000000000000000, 0.9510565162951535312, 1.000000000000000000, 0.9510565162951535312, 1.000000000000000000, 0.9510565162951535312, 1.000000000000000000, 0.9510565162951535312, 1.000000000000000000, 0.9510565162951535312, 1.000000000000000000, 0.9510565162951535312, 1.000000000000000000, 0.9510565162951535312, 1.000000000000000000, 0.9510565162951535312, 1.000000000000000000, 0.9510565162951535312, 1.000000000000000000, 0.9510565162951535312, 1.000000000000000000, 0.9510565162951535312, 1.000000000000000000, 0.9510565162951535312, 1.000000000000000000, 0.9510565162951535312, 1.000000000000000000, 0.9510565162951535312, 1.000000000000000000, 0.9510565162951535312, 1.000000000000000000, 0.9510565162951535312, 1.000000000000000000, 0.9510565162951535312, 1.000000000000000000, 0.9510565162951535312, 1.000000000000000000, 0.9510565162951535312, 1.000000000000000000, 0.9510565162951535312, 1.000000000000000000, 0.9510565162951535312, 1.000000000000000000, 0.9510565162951535312, 1.000000000000000000, 0.9510565162951535312, 1.000000000000000000, 0.9510565162951535312, 1.000000000000000000, 0.9510565162951535312, 1.000000000000000000, 0.9510565162951535312, 1.000000000000000000, 0.9510565162951535312, 1.000000000000000000, 0.9510565162951535312, 1.000000000000000000, 0.9510565162951535312, 1.000000000000000000, 0.9510565162951535312, 1.000000000000000000, 0.9510565162951535312, 1.000000000000000000, 0.9510565162951535312, 1.000000000000000000, 0.9510565162951535312, 1.000000000000000000, 0.9510565162951535312, 1.000000000000000000, 0.9510565162951535312, 1.000000000000000000, 0.9510565162951535312, 1.000000000000000000, 0.9510565162951535312, 1.000000000000000000, 0.9510565162951535312, 1.000000000000000000, 0.9510565162951535312, 1.000000000000000000, 0.9510565162951535312, 1.000000000000000000, 0.9510565162951535312, 1.000000000000000000, 0.9510565162951535312, 1.000000000000000000, 0.9510565162951535312, 1.000000000000000000, 0.9510565162951535312, 1.000000000000000000, 0.9510565162951535312, 1.000000000000000000, 0.9510565162951535312, 1.000000000000000000, 0.9510565162951535312, 1.000000000000000000, 0.9510565162951535312, 1.000000000000000000, 0.9510565162951535312, 1.000000000000000000, 0.9510565162951535312, 1.000000000000000000, 0.9510565162951535312, 1.000000000000000000, 0.9510565162951535312, 1.000000000000000000, 0.9510565162951535312, 1.000000000000000000, 0.9510565162951535312, 1.000000000000000000, 0.9510565162951535312, 1.000000000000000000, 0.9510565162951535312, 1.000000000000000000, 0.9510565162951535312, 1.000000000000000000, 0.9510565162951535312, 1.000000000000000000, 0.9510565162951535312, 1.000000000000000000, 0.9510565162951535312, 1.000000000000000000, 0.9510565162951535312, 1.000000000000000000, 0.9510565162951535312, 1.000000000000000000, 0.9510565162951535312, 1.000000000000000000, 0.9510565162951535312, 1.000000000000000000, 0.9510565162951535312, 1.000000000000000000, 0.9510565162951535312, 1.000000000000000000, 0.9510565162951535312, 1.000000000000000000, 0.9510565162951535312, 1.000000000000000000, 0.9510565162951535312, 1.000000000000000000, 0.9510565162951535312, 1.000000000000000000, 0.9510565162951535312, 1.000000000000000000, 0.9510565162951535312, 1.000000000000000000, 0.9510565162951535312, 1.000000000000000000, 0.9510565162951535312, 1.000000000000000000, 0.9510565162951535312, 1.000000000000000000, 0.9510565162951535312, 1.000000000000000000, 0.9510565162951535312, 1.000000000000000000, 0.9510565162951535312, 1.000000000000000000, 0.9510565162951535312, 1.000000000000000000, 0.9510565162951535312, 1.000000000000000000, 0.9510565162951535312, 1.000000000000000000, 0.9510565162951535312, 1.000000000000000000, 0.9510565162951535312, 1.000000000000000000, 0.9510565162951535312, 1.000000000000000000, 0.9510565162951535312, 1.000000000000000000, 0.9510565162951535312, 1.000000000000000000, 0.9510565162951535312, 1.000000000000000000, 0.9510565162951535312, 1.000000000000000000, 0.9510565162951535312, 1.000000000000000000, 0.9510565162951535312, 1.000000000000000000, 0.9510565162951535312, 1.000000000000000000, 0.9510565162951535312, 1.000000000000000000, 0.9510565162951535312, 1.000000000000000000, 0.9510565162951535312, 1.000000000000000000, 0.9510565162951535312, 1.000000000000000000, 0.9510565162951535312, 1.000000000000000000, 0.9510565162951535312, 1.000000000000000000, 0.9510565162951535312, 1.000000000000000000, 0.9510565162951535312, 1.000000000000000000, 0.9510565162951535312, 1.000000000000000000, 0.9510565162951535312, 1.000000000000000000, 0.9510565162951535312, 1.000000000000000000, 0.9510565162951535312, 1.000000000000000000, 0.9510565162951535312, 1.000000000000000000, 0.9510565162951535312, 1.000000000000000000, 0.9510565162951535312, 1.000000000000000000, 0.9510565162951535312, 1.000000000000000000, 0.9510565162951535312, 1.000000000000000000, 0.9510565162951535312, 1.000000000000000000, 0.9510565162951535312, 1.000000000000000000, 0.9510565162951535312, 1.000000000000000000, 0.9510565162951535312, 1.000000000000000000, 0.9510565162951535312, 1.000000000000000000, 0.9510565162951535312, 1.000000000000000000, 0.9510565162951535312, 1.000000000000000000, 0.9510565162951535312, 1.000000000000000000, 0.9510565162951535312, 1.000000000000000000, 0.9510565162951535312, 1.000000000000000000, 0.9510565162951535312, 1.000000000000000000, 0.9510565162951535312, 1.000000000000000000, 0.9510565162951535312, 1.000000000000000000, 0.9510565162951535312, 1.000000000000000000, 0.9510565162951535312, 1.000000000000000000, 0.9510565162951535312, 1.000000000000000000, 0.9510565162951535312, 1.000000000000000000, 0.9510565162951535312, 1.000000000000000000, 0.9510565162951535312, 1.000000000000000000, 0.9510565162951535312, 1.000000000000000000, 0.9510565162951535312, 1.000000000000000000, 0.9510565162951535312, 1.000000000000000000, 0.9510565162951535312, 1.000000000000000000, 0.9510565162951535312, 1.000000000000000000, 0.9510565162951535312, 1.000000000000000000, 0.9510565162951535312, 1.000000000000000000, 0.9510565162951535312, 1.000000000000000000, 0.9510565162951535312, 1.000000000000000000, 0.9510565162951535312, 1.000000000000000000, 0.9510565162951535312, 1.000000000000000000, 0.9510565162951535312, 1.000000000000000000, 0.9510565162951535312, 1.000000000000000000, 0.9510565162951535312, 1.000000000000000000, 0.9510565162951535312, 1.000000000000000000, 0.9510565162951535312, 1.000000000000000000, 0.9510565162951535312, 1.000000000000000000, 0.9510565162951535312, 1.000000000000000000, 0.9510565162951535312, 1.000000000000000000, 0.9510565162951535312, 1.000000000000000000, 0.9510565162951535312, 1.000000000000000000, 0.9510565162951535312, 1.000000000000000000, 0.9510565162951535312, 1.000000000000000000, 0.9510565162951535312, 1.000000000000000000, 0.9510565162951535312, 1.000000000000000000, 0.9510565162951535312, 1.000000000000000000, 0.9510565162951535312, 1.000000000000000000, 0.9510565162951535312, 1.000000000000000000, 0.9510565162951535312, 1.000000000000000000, 0.9510565162951535312, 1.000000000000000000, 0.9510565162951535312, 1.000000000000000000, 0.9510565162951535312, 1.000000000000000000, 0.9510565162951535312, 1.000000000000000000, 0.9510565162951535312, 1.000000000000000000, 1.000000000000000000, 1.000000000000000000),
 ( 0.3333333333333333703, 0.3170188387650512141, 0.3333333333333333703, 0.3170188387650512141, 0.3333333333333333703, 0.3170188387650512141, 0.3333333333333333703, 0.3170188387650512141, 0.3333333333333333703, 0.3170188387650512141, 0.3333333333333333703, 0.3170188387650512141, 0.3333333333333333703, 0.3170188387650512141, 0.3333333333333333703, 0.3170188387650512141, 0.3333333333333333703, 0.3170188387650512141, 0.3333333333333333703, 0.3170188387650512141, 0.3333333333333333703, 0.3170188387650512141, 0.3333333333333333703, 0.3170188387650512141, 0.3333333333333333703, 0.3170188387650512141, 0.3333333333333333703, 0.3170188387650512141, 0.3333333333333333703, 0.3170188387650512141, 0.3333333333333333703, 0.3170188387650512141, 0.3333333333333333703, 0.3170188387650512141, 0.3333333333333333703, 0.3170188387650512141, 0.3333333333333333703, 0.3170188387650512141, 0.3333333333333333703, 0.3170188387650512141, 0.3333333333333333703, 0.3170188387650512141, 0.3333333333333333703, 0.3170188387650512141, 0.3333333333333333703, 0.3170188387650512141, 0.3333333333333333703, 0.3170188387650512141, 0.3333333333333333703, 0.3170188387650512141, 0.3333333333333333703, 0.3170188387650512141, 0.3333333333333333703, 0.3170188387650512141, 0.3333333333333333703, 0.3170188387650512141, 0.3333333333333333703, 0.3170188387650512141, 0.3333333333333333703, 0.3170188387650512141, 0.3333333333333333703, 0.3170188387650512141, 0.3333333333333333703, 0.3170188387650512141, 0.3333333333333333703, 0.3170188387650512141, 0.3333333333333333703, 0.3170188387650512141, 0.3333333333333333703, 0.3170188387650512141, 0.3333333333333333703, 0.3170188387650512141, 0.3333333333333333703, 0.3170188387650512141, 0.3333333333333333703, 0.3170188387650512141, 0.3333333333333333703, 0.3170188387650512141, 0.3333333333333333703, 0.3170188387650512141, 0.3333333333333333703, 0.3170188387650512141, 0.3333333333333333703, 0.3170188387650512141, 0.3333333333333333703, 0.3170188387650512141, 0.3333333333333333703, 0.3170188387650512141, 0.3333333333333333703, 0.3170188387650512141, 0.3333333333333333703, 0.3170188387650512141, 0.3333333333333333703, 0.3170188387650512141, 0.3333333333333333703, 0.3170188387650512141, 0.3333333333333333703, 0.3170188387650512141, 0.3333333333333333703, 0.3170188387650512141, 0.3333333333333333703, 0.3170188387650512141, 0.3333333333333333703, 0.3170188387650512141, 0.3333333333333333703, 0.3170188387650512141, 0.3333333333333333703, 0.3170188387650512141, 0.3333333333333333703, 0.3170188387650512141, 0.3333333333333333703, 0.3170188387650512141, 0.3333333333333333703, 0.3170188387650512141, 0.3333333333333333703, 0.3170188387650512141, 0.3333333333333333703, 0.3170188387650512141, 0.3333333333333333703, 0.3170188387650512141, 0.3333333333333333703, 0.3170188387650512141, 0.3333333333333333703, 0.3170188387650512141, 0.3333333333333333703, 0.3170188387650512141, 0.3333333333333333703, 0.3170188387650512141, 0.3333333333333333703, 0.3170188387650512141, 0.3333333333333333703, 0.3170188387650512141, 0.3333333333333333703, 0.3170188387650512141, 0.3333333333333333703, 0.3170188387650512141, 0.3333333333333333703, 0.3170188387650512141, 0.3333333333333333703, 0.3170188387650512141, 0.3333333333333333703, 0.3170188387650512141, 0.3333333333333333703, 0.3170188387650512141, 0.3333333333333333703, 0.3170188387650512141, 0.3333333333333333703, 0.3170188387650512141, 0.3333333333333333703, 0.3170188387650512141, 0.3333333333333333703, 0.3170188387650512141, 0.3333333333333333703, 0.3170188387650512141, 0.3333333333333333703, 0.3170188387650512141, 0.3333333333333333703, 0.3170188387650512141, 0.3333333333333333703, 0.3170188387650512141, 0.3333333333333333703, 0.3170188387650512141, 0.3333333333333333703, 0.3170188387650512141, 0.3333333333333333703, 0.3170188387650512141, 0.3333333333333333703, 0.3170188387650512141, 0.3333333333333333703, 0.3170188387650512141, 0.3333333333333333703, 0.3170188387650512141, 0.3333333333333333703, 0.3170188387650512141, 0.3333333333333333703, 0.3170188387650512141, 0.3333333333333333703, 0.3170188387650512141, 0.3333333333333333703, 0.3170188387650512141, 0.3333333333333333703, 0.3170188387650512141, 0.3333333333333333703, 0.3170188387650512141, 0.3333333333333333703, 0.3170188387650512141, 0.3333333333333333703, 0.3170188387650512141, 0.3333333333333333703, 0.3170188387650512141, 0.3333333333333333703, 0.3170188387650512141, 0.3333333333333333703, 0.3170188387650512141, 0.3333333333333333703, 0.3170188387650512141, 0.3333333333333333703, 0.3170188387650512141, 0.3333333333333333703, 0.3170188387650512141, 0.3333333333333333703, 0.3170188387650512141, 0.3333333333333333703, 0.3170188387650512141, 0.3333333333333333703, 0.3170188387650512141, 0.3333333333333333703, 0.3170188387650512141, 0.3333333333333333703, 0.3170188387650512141, 0.3333333333333333703, 0.3170188387650512141, 0.3333333333333333703, 0.3170188387650512141, 0.3333333333333333703, 0.3170188387650512141, 0.3333333333333333703, 0.3170188387650512141, 0.3333333333333333703, 0.3170188387650512141, 0.3333333333333333703, 0.3170188387650512141, 0.3333333333333333703, 0.3170188387650512141, 0.3333333333333333703, 0.3170188387650512141, 0.3333333333333333703, 0.3170188387650512141, 0.3333333333333333703, 0.3170188387650512141, 0.3333333333333333703, 0.3170188387650512141, 0.3333333333333333703, 0.3170188387650512141, 0.3333333333333333703, 0.3170188387650512141, 0.3333333333333333703, 0.3170188387650512141, 0.3333333333333333703, 0.3170188387650512141, 0.3333333333333333703, 0.3170188387650512141, 0.3333333333333333703, 0.3170188387650512141, 0.3333333333333333703, 0.3170188387650512141, 0.3333333333333333703, 0.3170188387650512141, 0.3333333333333333703, 0.3170188387650512141, 0.3333333333333333703, 0.3170188387650512141, 0.3333333333333333703, 0.3170188387650512141, 0.3333333333333333703, 0.3170188387650512141, 0.3333333333333333703, 0.3170188387650512141, 0.3333333333333333703, 0.3170188387650512141, 0.3333333333333333703, 0.3170188387650512141, 0.3333333333333333703, 0.3170188387650512141, 0.3333333333333333703, 0.3170188387650512141, 0.3333333333333333703, 0.3170188387650512141, 0.3333333333333333703, 0.3170188387650512141, 0.3333333333333333703, 0.3170188387650512141, 0.3333333333333333703, 0.3170188387650512141, 0.3333333333333333703, 0.3170188387650512141, 0.3333333333333333703, 0.3170188387650512141, 0.3333333333333333703, 0.3170188387650512141, 0.3333333333333333703, 0.3170188387650512141, 0.3333333333333333703, 0.3170188387650512141, 0.3333333333333333703, 0.3170188387650512141, 0.3333333333333333703, 0.3170188387650512141, 0.3333333333333333703, 0.3170188387650512141, 0.3333333333333333703, 0.3170188387650512141, 0.3333333333333333703, 0.3170188387650512141, 0.3333333333333333703, 0.3170188387650512141, 0.3333333333333333703, 0.3170188387650512141, 0.3333333333333333703, 0.3170188387650512141, 0.3333333333333333703, 0.3170188387650512141, 0.3333333333333333703, 0.3170188387650512141, 0.3333333333333333703, 0.3170188387650512141, 0.3333333333333333703, 0.3170188387650512141, 0.3333333333333333703, 0.3170188387650512141, 0.3333333333333333703, 0.3170188387650512141, 0.3333333333333333703, 0.3170188387650512141, 0.3333333333333333703, 0.3170188387650512141, 0.3333333333333333703, 0.3170188387650512141, 0.3333333333333333703, 0.3170188387650512141, 0.3333333333333333703, 0.3170188387650512141, 0.3333333333333333703, 0.3170188387650512141, 0.3333333333333333703, 0.3170188387650512141, 0.3333333333333333703, 0.3170188387650512141, 0.3333333333333333703, 0.3170188387650512141, 0.3333333333333333703, 0.3170188387650512141, 0.3333333333333333703, 0.3170188387650512141, 0.3333333333333333703, 0.3170188387650512141, 0.3333333333333333703, 0.3170188387650512141, 0.3333333333333333703, 0.3170188387650512141, 0.3333333333333333703, 0.3170188387650512141, 0.3333333333333333703, 0.3170188387650512141, 0.3333333333333333703, 0.3170188387650512141, 0.3333333333333333703, 0.3170188387650512141, 0.3333333333333333703, 0.3170188387650512141, 0.3333333333333333703, 0.3170188387650512141, 0.3333333333333333703, 0.3170188387650512141, 0.3333333333333333703, 0.3170188387650512141, 0.3333333333333333703, 0.3170188387650512141, 0.3333333333333333703, 0.3170188387650512141, 0.3333333333333333703, 0.3170188387650512141, 0.3333333333333333703, 0.3170188387650512141, 0.3333333333333333703, 0.3170188387650512141, 0.3333333333333333703, 0.3170188387650512141, 0.3333333333333333703, 0.3170188387650512141, 0.3333333333333333703, 0.3170188387650512141, 0.3333333333333333703, 0.3170188387650512141, 0.3333333333333333703, 0.3170188387650512141, 0.3333333333333333703, 0.3170188387650512141, 0.3333333333333333703, 0.3170188387650512141, 0.3333333333333333703, 0.3170188387650512141, 0.3333333333333333703, 0.3170188387650512141, 0.3333333333333333703, 0.3170188387650512141, 0.3333333333333333703, 0.3170188387650512141, 0.3333333333333333703, 0.3170188387650512141, 0.3333333333333333703, 0.3170188387650512141, 0.3333333333333333703, 0.3170188387650512141, 0.3333333333333333703, 0.3170188387650512141, 0.3333333333333333703, 0.3170188387650512141, 0.3333333333333333703, 0.3170188387650512141, 0.3333333333333333703, 0.3170188387650512141, 0.3333333333333333703, 0.3170188387650512141, 0.3333333333333333703, 0.3170188387650512141, 0.3333333333333333703, 0.3170188387650512141, 0.3333333333333333703, 0.3170188387650512141, 0.3333333333333333703, 0.3170188387650512141, 0.3333333333333333703, 0.3170188387650512141, 0.3333333333333333703, 0.3170188387650512141, 0.3333333333333333703, 0.3170188387650512141, 0.3333333333333333703, 0.3170188387650512141, 0.3333333333333333703, 0.3170188387650512141, 0.3333333333333333703, 0.3170188387650512141, 0.3333333333333333703, 0.3170188387650512141, 0.3333333333333333703, 0.3170188387650512141, 0.3333333333333333703, 0.3170188387650512141, 0.3333333333333333703, 0.3170188387650512141, 0.3333333333333333703, 0.3170188387650512141, 0.3333333333333333703, 0.3170188387650512141, 0.3333333333333333703, 0.3170188387650512141, 0.3333333333333333703, 0.3170188387650512141, 0.3333333333333333703, 0.3170188387650512141, 0.3333333333333333703, 0.3170188387650512141, 0.3333333333333333703, 0.3170188387650512141, 0.3333333333333333703, 0.3170188387650512141, 0.3333333333333333703, 0.3170188387650512141, 0.3333333333333333703, 0.3170188387650512141, 0.3333333333333333703, 0.3170188387650512141, 0.3333333333333333703, 0.3170188387650512141, 0.3333333333333333703, 0.3170188387650512141, 0.3333333333333333703, 0.3170188387650512141, 0.3333333333333333703, 0.3170188387650512141, 0.3333333333333333703, 0.3170188387650512141, 0.3333333333333333703, 0.3170188387650512141, 0.3333333333333333703, 0.3170188387650512141, 0.3333333333333333703, 0.3170188387650512141, 0.3333333333333333703, 0.3170188387650512141, 0.3333333333333333703, 0.3170188387650512141, 0.3333333333333333703, 0.3170188387650512141, 0.3333333333333333703, 0.3170188387650512141, 0.3333333333333333703, 0.3170188387650512141, 0.3333333333333333703, 0.3170188387650512141, 0.3333333333333333703, 0.3170188387650512141, 0.3333333333333333703, 0.3170188387650512141, 0.3333333333333333703, 0.3170188387650512141, 0.3333333333333333703, 0.3170188387650512141, 0.3333333333333333703, 0.3170188387650512141, 0.3333333333333333703, 0.3170188387650512141, 0.3333333333333333703, 0.3170188387650512141, 0.3333333333333333703, 0.3170188387650512141, 0.3333333333333333703, 0.3170188387650512141, 0.3333333333333333703, 0.3170188387650512141, 0.3333333333333333703, 0.3170188387650512141, 0.3333333333333333703, 0.3170188387650512141, 0.3333333333333333703, 0.3170188387650512141, 0.3333333333333333703, 0.3170188387650512141, 0.3333333333333333703, 0.3170188387650512141, 0.3333333333333333703, 0.3170188387650512141, 0.3333333333333333703, 0.3170188387650512141, 0.3333333333333333703, 0.3170188387650512141, 0.3333333333333333703, 0.3170188387650512141, 0.3333333333333333703, 0.3170188387650512141, 0.3333333333333333703, 0.3170188387650512141, 0.3333333333333333703, 0.3170188387650512141, 0.3333333333333333703, 0.3170188387650512141, 0.3333333333333333703, 0.3170188387650512141, 0.3333333333333333703, 0.3170188387650512141, 0.3333333333333333703, 0.3170188387650512141, 0.3333333333333333703, 0.3170188387650512141, 0.3333333333333333703, 0.3170188387650512141, 0.3333333333333333703, 0.3170188387650512141, 0.3333333333333333703, 0.3170188387650512141, 0.3333333333333333703, 0.3170188387650512141, 0.3333333333333333703, 0.3170188387650512141, 0.3333333333333333703, 0.3170188387650512141, 0.3333333333333333703, 0.3170188387650512141, 0.3333333333333333703, 0.3170188387650512141, 0.3333333333333333703, 0.3170188387650512141, 0.3333333333333333703, 0.3170188387650512141, 0.3333333333333333703, 0.3170188387650512141, 0.3333333333333333703, 0.3170188387650512141, 0.3333333333333333703, 0.3170188387650512141, 0.3333333333333333703, 0.3170188387650512141, 0.3333333333333333703, 0.3170188387650512141, 0.3333333333333333703, 0.3170188387650512141, 0.3333333333333333703, 0.3170188387650512141, 0.3333333333333333703, 0.3170188387650512141, 0.3333333333333333703, 0.3170188387650512141, 0.3333333333333333703, 0.3170188387650512141, 0.3333333333333333703, 0.3170188387650512141, 0.3333333333333333703, 0.3170188387650512141, 0.3333333333333333703, 0.3170188387650512141, 0.3333333333333333703, 0.3170188387650512141, 0.3333333333333333703, 0.3170188387650512141, 0.3333333333333333703, 0.3170188387650512141, 0.3333333333333333703, 0.3170188387650512141, 0.3333333333333333703, 0.3170188387650512141, 0.3333333333333333703, 0.3170188387650512141, 0.3333333333333333703, 0.3170188387650512141, 0.3333333333333333703, 0.3170188387650512141, 0.3333333333333333703, 0.3170188387650512141, 0.3333333333333333703, 0.3170188387650512141, 0.3333333333333333703, 0.3170188387650512141, 0.3333333333333333703, 0.3170188387650512141, 0.3333333333333333703, 0.3170188387650512141, 0.3333333333333333703, 0.3170188387650512141, 0.3333333333333333703, 0.3170188387650512141, 0.3333333333333333703, 0.3170188387650512141, 0.3333333333333333703, 0.3170188387650512141, 0.3333333333333333703, 0.3170188387650512141, 0.3333333333333333703, 0.3170188387650512141, 0.3333333333333333703, 0.3170188387650512141, 0.3333333333333333703, 0.3170188387650512141, 0.3333333333333333703, 0.3170188387650512141, 0.3333333333333333703, 0.3170188387650512141, 0.3333333333333333703, 0.3170188387650512141, 0.3333333333333333703, 0.3170188387650512141, 0.3333333333333333703, 0.3170188387650512141, 0.3333333333333333703, 0.3170188387650512141, 0.3333333333333333703, 0.3170188387650512141, 0.3333333333333333703, 0.3170188387650512141, 0.3333333333333333703, 0.3170188387650512141, 0.3333333333333333703, 0.3170188387650512141, 0.3333333333333333703, 0.3170188387650512141, 0.3333333333333333703, 0.3170188387650512141, 0.3333333333333333703, 0.3170188387650512141, 0.3333333333333333703, 0.3170188387650512141, 0.3333333333333333703, 0.3170188387650512141, 0.3333333333333333703, 0.3170188387650512141, 0.3333333333333333703, 0.3170188387650512141, 0.3333333333333333703, 0.3170188387650512141, 0.3333333333333333703, 0.3170188387650512141, 0.3333333333333333703, 0.3170188387650512141, 0.3333333333333333703, 0.3170188387650512141, 0.3333333333333333703, 0.3170188387650512141, 0.3333333333333333703, 0.3170188387650512141, 0.3333333333333333703, 0.3170188387650512141, 0.3333333333333333703, 0.3170188387650512141, 0.3333333333333333703, 0.3170188387650512141, 0.3333333333333333703, 0.3170188387650512141, 0.3333333333333333703, 0.3170188387650512141, 0.3333333333333333703, 0.3170188387650512141, 0.3333333333333333703, 0.3170188387650512141, 0.3333333333333333703, 0.3170188387650512141, 0.3333333333333333703, 0.3170188387650512141, 0.3333333333333333703, 0.3170188387650512141, 0.3333333333333333703, 0.3333333333333333703, 0.3333333333333333703),
 ( 0.3333333333333333703, 0.3170188387650512141, 0.3333333333333333703, 0.3170188387650512141, 0.3333333333333333703, 0.3170188387650512141, 0.3333333333333333703, 0.3170188387650512141, 0.3333333333333333703, 0.3170188387650512141, 0.3333333333333333703, 0.3170188387650512141, 0.3333333333333333703, 0.3170188387650512141, 0.3333333333333333703, 0.3170188387650512141, 0.3333333333333333703, 0.3170188387650512141, 0.3333333333333333703, 0.3170188387650512141, 0.3333333333333333703, 0.3170188387650512141, 0.3333333333333333703, 0.3170188387650512141, 0.3333333333333333703, 0.3170188387650512141, 0.3333333333333333703, 0.3170188387650512141, 0.3333333333333333703, 0.3170188387650512141, 0.3333333333333333703, 0.3170188387650512141, 0.3333333333333333703, 0.3170188387650512141, 0.3333333333333333703, 0.3170188387650512141, 0.3333333333333333703, 0.3170188387650512141, 0.3333333333333333703, 0.3170188387650512141, 0.3333333333333333703, 0.3170188387650512141, 0.3333333333333333703, 0.3170188387650512141, 0.3333333333333333703, 0.3170188387650512141, 0.3333333333333333703, 0.3170188387650512141, 0.3333333333333333703, 0.3170188387650512141, 0.3333333333333333703, 0.3170188387650512141, 0.3333333333333333703, 0.3170188387650512141, 0.3333333333333333703, 0.3170188387650512141, 0.3333333333333333703, 0.3170188387650512141, 0.3333333333333333703, 0.3170188387650512141, 0.3333333333333333703, 0.3170188387650512141, 0.3333333333333333703, 0.3170188387650512141, 0.3333333333333333703, 0.3170188387650512141, 0.3333333333333333703, 0.3170188387650512141, 0.3333333333333333703, 0.3170188387650512141, 0.3333333333333333703, 0.3170188387650512141, 0.3333333333333333703, 0.3170188387650512141, 0.3333333333333333703, 0.3170188387650512141, 0.3333333333333333703, 0.3170188387650512141, 0.3333333333333333703, 0.3170188387650512141, 0.3333333333333333703, 0.3170188387650512141, 0.3333333333333333703, 0.3170188387650512141, 0.3333333333333333703, 0.3170188387650512141, 0.3333333333333333703, 0.3170188387650512141, 0.3333333333333333703, 0.3170188387650512141, 0.3333333333333333703, 0.3170188387650512141, 0.3333333333333333703, 0.3170188387650512141, 0.3333333333333333703, 0.3170188387650512141, 0.3333333333333333703, 0.3170188387650512141, 0.3333333333333333703, 0.3170188387650512141, 0.3333333333333333703, 0.3170188387650512141, 0.3333333333333333703, 0.3170188387650512141, 0.3333333333333333703, 0.3170188387650512141, 0.3333333333333333703, 0.3170188387650512141, 0.3333333333333333703, 0.3170188387650512141, 0.3333333333333333703, 0.3170188387650512141, 0.3333333333333333703, 0.3170188387650512141, 0.3333333333333333703, 0.3170188387650512141, 0.3333333333333333703, 0.3170188387650512141, 0.3333333333333333703, 0.3170188387650512141, 0.3333333333333333703, 0.3170188387650512141, 0.3333333333333333703, 0.3170188387650512141, 0.3333333333333333703, 0.3170188387650512141, 0.3333333333333333703, 0.3170188387650512141, 0.3333333333333333703, 0.3170188387650512141, 0.3333333333333333703, 0.3170188387650512141, 0.3333333333333333703, 0.3170188387650512141, 0.3333333333333333703, 0.3170188387650512141, 0.3333333333333333703, 0.3170188387650512141, 0.3333333333333333703, 0.3170188387650512141, 0.3333333333333333703, 0.3170188387650512141, 0.3333333333333333703, 0.3170188387650512141, 0.3333333333333333703, 0.3170188387650512141, 0.3333333333333333703, 0.3170188387650512141, 0.3333333333333333703, 0.3170188387650512141, 0.3333333333333333703, 0.3170188387650512141, 0.3333333333333333703, 0.3170188387650512141, 0.3333333333333333703, 0.3170188387650512141, 0.3333333333333333703, 0.3170188387650512141, 0.3333333333333333703, 0.3170188387650512141, 0.3333333333333333703, 0.3170188387650512141, 0.3333333333333333703, 0.3170188387650512141, 0.3333333333333333703, 0.3170188387650512141, 0.3333333333333333703, 0.3170188387650512141, 0.3333333333333333703, 0.3170188387650512141, 0.3333333333333333703, 0.3170188387650512141, 0.3333333333333333703, 0.3170188387650512141, 0.3333333333333333703, 0.3170188387650512141, 0.3333333333333333703, 0.3170188387650512141, 0.3333333333333333703, 0.3170188387650512141, 0.3333333333333333703, 0.3170188387650512141, 0.3333333333333333703, 0.3170188387650512141, 0.3333333333333333703, 0.3170188387650512141, 0.3333333333333333703, 0.3170188387650512141, 0.3333333333333333703, 0.3170188387650512141, 0.3333333333333333703, 0.3170188387650512141, 0.3333333333333333703, 0.3170188387650512141, 0.3333333333333333703, 0.3170188387650512141, 0.3333333333333333703, 0.3170188387650512141, 0.3333333333333333703, 0.3170188387650512141, 0.3333333333333333703, 0.3170188387650512141, 0.3333333333333333703, 0.3170188387650512141, 0.3333333333333333703, 0.3170188387650512141, 0.3333333333333333703, 0.3170188387650512141, 0.3333333333333333703, 0.3170188387650512141, 0.3333333333333333703, 0.3170188387650512141, 0.3333333333333333703, 0.3170188387650512141, 0.3333333333333333703, 0.3170188387650512141, 0.3333333333333333703, 0.3170188387650512141, 0.3333333333333333703, 0.3170188387650512141, 0.3333333333333333703, 0.3170188387650512141, 0.3333333333333333703, 0.3170188387650512141, 0.3333333333333333703, 0.3170188387650512141, 0.3333333333333333703, 0.3170188387650512141, 0.3333333333333333703, 0.3170188387650512141, 0.3333333333333333703, 0.3170188387650512141, 0.3333333333333333703, 0.3170188387650512141, 0.3333333333333333703, 0.3170188387650512141, 0.3333333333333333703, 0.3170188387650512141, 0.3333333333333333703, 0.3170188387650512141, 0.3333333333333333703, 0.3170188387650512141, 0.3333333333333333703, 0.3170188387650512141, 0.3333333333333333703, 0.3170188387650512141, 0.3333333333333333703, 0.3170188387650512141, 0.3333333333333333703, 0.3170188387650512141, 0.3333333333333333703, 0.3170188387650512141, 0.3333333333333333703, 0.3170188387650512141, 0.3333333333333333703, 0.3170188387650512141, 0.3333333333333333703, 0.3170188387650512141, 0.3333333333333333703, 0.3170188387650512141, 0.3333333333333333703, 0.3170188387650512141, 0.3333333333333333703, 0.3170188387650512141, 0.3333333333333333703, 0.3170188387650512141, 0.3333333333333333703, 0.3170188387650512141, 0.3333333333333333703, 0.3170188387650512141, 0.3333333333333333703, 0.3170188387650512141, 0.3333333333333333703, 0.3170188387650512141, 0.3333333333333333703, 0.3170188387650512141, 0.3333333333333333703, 0.3170188387650512141, 0.3333333333333333703, 0.3170188387650512141, 0.3333333333333333703, 0.3170188387650512141, 0.3333333333333333703, 0.3170188387650512141, 0.3333333333333333703, 0.3170188387650512141, 0.3333333333333333703, 0.3170188387650512141, 0.3333333333333333703, 0.3170188387650512141, 0.3333333333333333703, 0.3170188387650512141, 0.3333333333333333703, 0.3170188387650512141, 0.3333333333333333703, 0.3170188387650512141, 0.3333333333333333703, 0.3170188387650512141, 0.3333333333333333703, 0.3170188387650512141, 0.3333333333333333703, 0.3170188387650512141, 0.3333333333333333703, 0.3170188387650512141, 0.3333333333333333703, 0.3170188387650512141, 0.3333333333333333703, 0.3170188387650512141, 0.3333333333333333703, 0.3170188387650512141, 0.3333333333333333703, 0.3170188387650512141, 0.3333333333333333703, 0.3170188387650512141, 0.3333333333333333703, 0.3170188387650512141, 0.3333333333333333703, 0.3170188387650512141, 0.3333333333333333703, 0.3170188387650512141, 0.3333333333333333703, 0.3170188387650512141, 0.3333333333333333703, 0.3170188387650512141, 0.3333333333333333703, 0.3170188387650512141, 0.3333333333333333703, 0.3170188387650512141, 0.3333333333333333703, 0.3170188387650512141, 0.3333333333333333703, 0.3170188387650512141, 0.3333333333333333703, 0.3170188387650512141, 0.3333333333333333703, 0.3170188387650512141, 0.3333333333333333703, 0.3170188387650512141, 0.3333333333333333703, 0.3170188387650512141, 0.3333333333333333703, 0.3170188387650512141, 0.3333333333333333703, 0.3170188387650512141, 0.3333333333333333703, 0.3170188387650512141, 0.3333333333333333703, 0.3170188387650512141, 0.3333333333333333703, 0.3170188387650512141, 0.3333333333333333703, 0.3170188387650512141, 0.3333333333333333703, 0.3170188387650512141, 0.3333333333333333703, 0.3170188387650512141, 0.3333333333333333703, 0.3170188387650512141, 0.3333333333333333703, 0.3170188387650512141, 0.3333333333333333703, 0.3170188387650512141, 0.3333333333333333703, 0.3170188387650512141, 0.3333333333333333703, 0.3170188387650512141, 0.3333333333333333703, 0.3170188387650512141, 0.3333333333333333703, 0.3170188387650512141, 0.3333333333333333703, 0.3170188387650512141, 0.3333333333333333703, 0.3170188387650512141, 0.3333333333333333703, 0.3170188387650512141, 0.3333333333333333703, 0.3170188387650512141, 0.3333333333333333703, 0.3170188387650512141, 0.3333333333333333703, 0.3170188387650512141, 0.3333333333333333703, 0.3170188387650512141, 0.3333333333333333703, 0.3170188387650512141, 0.3333333333333333703, 0.3170188387650512141, 0.3333333333333333703, 0.3170188387650512141, 0.3333333333333333703, 0.3170188387650512141, 0.3333333333333333703, 0.3170188387650512141, 0.3333333333333333703, 0.3170188387650512141, 0.3333333333333333703, 0.3170188387650512141, 0.3333333333333333703, 0.3170188387650512141, 0.3333333333333333703, 0.3170188387650512141, 0.3333333333333333703, 0.3170188387650512141, 0.3333333333333333703, 0.3170188387650512141, 0.3333333333333333703, 0.3170188387650512141, 0.3333333333333333703, 0.3170188387650512141, 0.3333333333333333703, 0.3170188387650512141, 0.3333333333333333703, 0.3170188387650512141, 0.3333333333333333703, 0.3170188387650512141, 0.3333333333333333703, 0.3170188387650512141, 0.3333333333333333703, 0.3170188387650512141, 0.3333333333333333703, 0.3170188387650512141, 0.3333333333333333703, 0.3170188387650512141, 0.3333333333333333703, 0.3170188387650512141, 0.3333333333333333703, 0.3170188387650512141, 0.3333333333333333703, 0.3170188387650512141, 0.3333333333333333703, 0.3170188387650512141, 0.3333333333333333703, 0.3170188387650512141, 0.3333333333333333703, 0.3170188387650512141, 0.3333333333333333703, 0.3170188387650512141, 0.3333333333333333703, 0.3170188387650512141, 0.3333333333333333703, 0.3170188387650512141, 0.3333333333333333703, 0.3170188387650512141, 0.3333333333333333703, 0.3170188387650512141, 0.3333333333333333703, 0.3170188387650512141, 0.3333333333333333703, 0.3170188387650512141, 0.3333333333333333703, 0.3170188387650512141, 0.3333333333333333703, 0.3170188387650512141, 0.3333333333333333703, 0.3170188387650512141, 0.3333333333333333703, 0.3170188387650512141, 0.3333333333333333703, 0.3170188387650512141, 0.3333333333333333703, 0.3170188387650512141, 0.3333333333333333703, 0.3170188387650512141, 0.3333333333333333703, 0.3170188387650512141, 0.3333333333333333703, 0.3170188387650512141, 0.3333333333333333703, 0.3170188387650512141, 0.3333333333333333703, 0.3170188387650512141, 0.3333333333333333703, 0.3170188387650512141, 0.3333333333333333703, 0.3170188387650512141, 0.3333333333333333703, 0.3170188387650512141, 0.3333333333333333703, 0.3170188387650512141, 0.3333333333333333703, 0.3170188387650512141, 0.3333333333333333703, 0.3170188387650512141, 0.3333333333333333703, 0.3170188387650512141, 0.3333333333333333703, 0.3170188387650512141, 0.3333333333333333703, 0.3170188387650512141, 0.3333333333333333703, 0.3170188387650512141, 0.3333333333333333703, 0.3170188387650512141, 0.3333333333333333703, 0.3170188387650512141, 0.3333333333333333703, 0.3170188387650512141, 0.3333333333333333703, 0.3170188387650512141, 0.3333333333333333703, 0.3170188387650512141, 0.3333333333333333703, 0.3170188387650512141, 0.3333333333333333703, 0.3170188387650512141, 0.3333333333333333703, 0.3170188387650512141, 0.3333333333333333703, 0.3170188387650512141, 0.3333333333333333703, 0.3170188387650512141, 0.3333333333333333703, 0.3170188387650512141, 0.3333333333333333703, 0.3170188387650512141, 0.3333333333333333703, 0.3170188387650512141, 0.3333333333333333703, 0.3170188387650512141, 0.3333333333333333703, 0.3170188387650512141, 0.3333333333333333703, 0.3170188387650512141, 0.3333333333333333703, 0.3170188387650512141, 0.3333333333333333703, 0.3170188387650512141, 0.3333333333333333703, 0.3170188387650512141, 0.3333333333333333703, 0.3170188387650512141, 0.3333333333333333703, 0.3170188387650512141, 0.3333333333333333703, 0.3170188387650512141, 0.3333333333333333703, 0.3170188387650512141, 0.3333333333333333703, 0.3170188387650512141, 0.3333333333333333703, 0.3170188387650512141, 0.3333333333333333703, 0.3170188387650512141, 0.3333333333333333703, 0.3170188387650512141, 0.3333333333333333703, 0.3170188387650512141, 0.3333333333333333703, 0.3170188387650512141, 0.3333333333333333703, 0.3170188387650512141, 0.3333333333333333703, 0.3170188387650512141, 0.3333333333333333703, 0.3170188387650512141, 0.3333333333333333703, 0.3170188387650512141, 0.3333333333333333703, 0.3170188387650512141, 0.3333333333333333703, 0.3170188387650512141, 0.3333333333333333703, 0.3170188387650512141, 0.3333333333333333703, 0.3170188387650512141, 0.3333333333333333703, 0.3170188387650512141, 0.3333333333333333703, 0.3170188387650512141, 0.3333333333333333703, 0.3170188387650512141, 0.3333333333333333703, 0.3170188387650512141, 0.3333333333333333703, 0.3170188387650512141, 0.3333333333333333703, 0.3170188387650512141, 0.3333333333333333703, 0.3170188387650512141, 0.3333333333333333703, 0.3170188387650512141, 0.3333333333333333703, 0.3170188387650512141, 0.3333333333333333703, 0.3170188387650512141, 0.3333333333333333703, 0.3170188387650512141, 0.3333333333333333703, 0.3170188387650512141, 0.3333333333333333703, 0.3170188387650512141, 0.3333333333333333703, 0.3170188387650512141, 0.3333333333333333703, 0.3170188387650512141, 0.3333333333333333703, 0.3170188387650512141, 0.3333333333333333703, 0.3170188387650512141, 0.3333333333333333703, 0.3170188387650512141, 0.3333333333333333703, 0.3170188387650512141, 0.3333333333333333703, 0.3170188387650512141, 0.3333333333333333703, 0.3170188387650512141, 0.3333333333333333703, 0.3170188387650512141, 0.3333333333333333703, 0.3170188387650512141, 0.3333333333333333703, 0.3170188387650512141, 0.3333333333333333703, 0.3170188387650512141, 0.3333333333333333703, 0.3170188387650512141, 0.3333333333333333703, 0.3170188387650512141, 0.3333333333333333703, 0.3170188387650512141, 0.3333333333333333703, 0.3170188387650512141, 0.3333333333333333703, 0.3170188387650512141, 0.3333333333333333703, 0.3170188387650512141, 0.3333333333333333703, 0.3170188387650512141, 0.3333333333333333703, 0.3170188387650512141, 0.3333333333333333703, 0.3170188387650512141, 0.3333333333333333703, 0.3170188387650512141, 0.3333333333333333703, 0.3170188387650512141, 0.3333333333333333703, 0.3170188387650512141, 0.3333333333333333703, 0.3170188387650512141, 0.3333333333333333703, 0.3170188387650512141, 0.3333333333333333703, 0.3170188387650512141, 0.3333333333333333703, 0.3170188387650512141, 0.3333333333333333703, 0.3170188387650512141, 0.3333333333333333703, 0.3170188387650512141, 0.3333333333333333703, 0.3170188387650512141, 0.3333333333333333703, 0.3170188387650512141, 0.3333333333333333703, 0.3170188387650512141, 0.3333333333333333703, 0.3170188387650512141, 0.3333333333333333703, 0.3170188387650512141, 0.3333333333333333703, 0.3170188387650512141, 0.3333333333333333703, 0.3170188387650512141, 0.3333333333333333703, 0.3170188387650512141, 0.3333333333333333703, 0.3170188387650512141, 0.3333333333333333703, 0.3170188387650512141, 0.3333333333333333703, 0.3170188387650512141, 0.3333333333333333703, 0.3170188387650512141, 0.3333333333333333703, 0.3170188387650512141, 0.3333333333333333703, 0.3170188387650512141, 0.3333333333333333703, 0.3170188387650512141, 0.3333333333333333703, 0.3170188387650512141, 0.3333333333333333703, 0.3170188387650512141, 0.3333333333333333703, 0.3170188387650512141, 0.3333333333333333703, 0.3170188387650512141, 0.3333333333333333703, 0.3333333333333333703, 0.3333333333333333703),
 ( 1.000000000000000000, 0.9510565162951535312, 1.000000000000000000, 0.9510565162951535312, 1.000000000000000000, 0.9510565162951535312, 1.000000000000000000, 0.9510565162951535312, 1.000000000000000000, 0.9510565162951535312, 1.000000000000000000, 0.9510565162951535312, 1.000000000000000000, 0.9510565162951535312, 1.000000000000000000, 0.9510565162951535312, 1.000000000000000000, 0.9510565162951535312, 1.000000000000000000, 0.9510565162951535312, 1.000000000000000000, 0.9510565162951535312, 1.000000000000000000, 0.9510565162951535312, 1.000000000000000000, 0.9510565162951535312, 1.000000000000000000, 0.9510565162951535312, 1.000000000000000000, 0.9510565162951535312, 1.000000000000000000, 0.9510565162951535312, 1.000000000000000000, 0.9510565162951535312, 1.000000000000000000, 0.9510565162951535312, 1.000000000000000000, 0.9510565162951535312, 1.000000000000000000, 0.9510565162951535312, 1.000000000000000000, 0.9510565162951535312, 1.000000000000000000, 0.9510565162951535312, 1.000000000000000000, 0.9510565162951535312, 1.000000000000000000, 0.9510565162951535312, 1.000000000000000000, 0.9510565162951535312, 1.000000000000000000, 0.9510565162951535312, 1.000000000000000000, 0.9510565162951535312, 1.000000000000000000, 0.9510565162951535312, 1.000000000000000000, 0.9510565162951535312, 1.000000000000000000, 0.9510565162951535312, 1.000000000000000000, 0.9510565162951535312, 1.000000000000000000, 0.9510565162951535312, 1.000000000000000000, 0.9510565162951535312, 1.000000000000000000, 0.9510565162951535312, 1.000000000000000000, 0.9510565162951535312, 1.000000000000000000, 0.9510565162951535312, 1.000000000000000000, 0.9510565162951535312, 1.000000000000000000, 0.9510565162951535312, 1.000000000000000000, 0.9510565162951535312, 1.000000000000000000, 0.9510565162951535312, 1.000000000000000000, 0.9510565162951535312, 1.000000000000000000, 0.9510565162951535312, 1.000000000000000000, 0.9510565162951535312, 1.000000000000000000, 0.9510565162951535312, 1.000000000000000000, 0.9510565162951535312, 1.000000000000000000, 0.9510565162951535312, 1.000000000000000000, 0.9510565162951535312, 1.000000000000000000, 0.9510565162951535312, 1.000000000000000000, 0.9510565162951535312, 1.000000000000000000, 0.9510565162951535312, 1.000000000000000000, 0.9510565162951535312, 1.000000000000000000, 0.9510565162951535312, 1.000000000000000000, 0.9510565162951535312, 1.000000000000000000, 0.9510565162951535312, 1.000000000000000000, 0.9510565162951535312, 1.000000000000000000, 0.9510565162951535312, 1.000000000000000000, 0.9510565162951535312, 1.000000000000000000, 0.9510565162951535312, 1.000000000000000000, 0.9510565162951535312, 1.000000000000000000, 0.9510565162951535312, 1.000000000000000000, 0.9510565162951535312, 1.000000000000000000, 0.9510565162951535312, 1.000000000000000000, 0.9510565162951535312, 1.000000000000000000, 0.9510565162951535312, 1.000000000000000000, 0.9510565162951535312, 1.000000000000000000, 0.9510565162951535312, 1.000000000000000000, 0.9510565162951535312, 1.000000000000000000, 0.9510565162951535312, 1.000000000000000000, 0.9510565162951535312, 1.000000000000000000, 0.9510565162951535312, 1.000000000000000000, 0.9510565162951535312, 1.000000000000000000, 0.9510565162951535312, 1.000000000000000000, 0.9510565162951535312, 1.000000000000000000, 0.9510565162951535312, 1.000000000000000000, 0.9510565162951535312, 1.000000000000000000, 0.9510565162951535312, 1.000000000000000000, 0.9510565162951535312, 1.000000000000000000, 0.9510565162951535312, 1.000000000000000000, 0.9510565162951535312, 1.000000000000000000, 0.9510565162951535312, 1.000000000000000000, 0.9510565162951535312, 1.000000000000000000, 0.9510565162951535312, 1.000000000000000000, 0.9510565162951535312, 1.000000000000000000, 0.9510565162951535312, 1.000000000000000000, 0.9510565162951535312, 1.000000000000000000, 0.9510565162951535312, 1.000000000000000000, 0.9510565162951535312, 1.000000000000000000, 0.9510565162951535312, 1.000000000000000000, 0.9510565162951535312, 1.000000000000000000, 0.9510565162951535312, 1.000000000000000000, 0.9510565162951535312, 1.000000000000000000, 0.9510565162951535312, 1.000000000000000000, 0.9510565162951535312, 1.000000000000000000, 0.9510565162951535312, 1.000000000000000000, 0.9510565162951535312, 1.000000000000000000, 0.9510565162951535312, 1.000000000000000000, 0.9510565162951535312, 1.000000000000000000, 0.9510565162951535312, 1.000000000000000000, 0.9510565162951535312, 1.000000000000000000, 0.9510565162951535312, 1.000000000000000000, 0.9510565162951535312, 1.000000000000000000, 0.9510565162951535312, 1.000000000000000000, 0.9510565162951535312, 1.000000000000000000, 0.9510565162951535312, 1.000000000000000000, 0.9510565162951535312, 1.000000000000000000, 0.9510565162951535312, 1.000000000000000000, 0.9510565162951535312, 1.000000000000000000, 0.9510565162951535312, 1.000000000000000000, 0.9510565162951535312, 1.000000000000000000, 0.9510565162951535312, 1.000000000000000000, 0.9510565162951535312, 1.000000000000000000, 0.9510565162951535312, 1.000000000000000000, 0.9510565162951535312, 1.000000000000000000, 0.9510565162951535312, 1.000000000000000000, 0.9510565162951535312, 1.000000000000000000, 0.9510565162951535312, 1.000000000000000000, 0.9510565162951535312, 1.000000000000000000, 0.9510565162951535312, 1.000000000000000000, 0.9510565162951535312, 1.000000000000000000, 0.9510565162951535312, 1.000000000000000000, 0.9510565162951535312, 1.000000000000000000, 0.9510565162951535312, 1.000000000000000000, 0.9510565162951535312, 1.000000000000000000, 0.9510565162951535312, 1.000000000000000000, 0.9510565162951535312, 1.000000000000000000, 0.9510565162951535312, 1.000000000000000000, 0.9510565162951535312, 1.000000000000000000, 0.9510565162951535312, 1.000000000000000000, 0.9510565162951535312, 1.000000000000000000, 0.9510565162951535312, 1.000000000000000000, 0.9510565162951535312, 1.000000000000000000, 0.9510565162951535312, 1.000000000000000000, 0.9510565162951535312, 1.000000000000000000, 0.9510565162951535312, 1.000000000000000000, 0.9510565162951535312, 1.000000000000000000, 0.9510565162951535312, 1.000000000000000000, 0.9510565162951535312, 1.000000000000000000, 0.9510565162951535312, 1.000000000000000000, 0.9510565162951535312, 1.000000000000000000, 0.9510565162951535312, 1.000000000000000000, 0.9510565162951535312, 1.000000000000000000, 0.9510565162951535312, 1.000000000000000000, 0.9510565162951535312, 1.000000000000000000, 0.9510565162951535312, 1.000000000000000000, 0.9510565162951535312, 1.000000000000000000, 0.9510565162951535312, 1.000000000000000000, 0.9510565162951535312, 1.000000000000000000, 0.9510565162951535312, 1.000000000000000000, 0.9510565162951535312, 1.000000000000000000, 0.9510565162951535312, 1.000000000000000000, 0.9510565162951535312, 1.000000000000000000, 0.9510565162951535312, 1.000000000000000000, 0.9510565162951535312, 1.000000000000000000, 0.9510565162951535312, 1.000000000000000000, 0.9510565162951535312, 1.000000000000000000, 0.9510565162951535312, 1.000000000000000000, 0.9510565162951535312, 1.000000000000000000, 0.9510565162951535312, 1.000000000000000000, 0.9510565162951535312, 1.000000000000000000, 0.9510565162951535312, 1.000000000000000000, 0.9510565162951535312, 1.000000000000000000, 0.9510565162951535312, 1.000000000000000000, 0.9510565162951535312, 1.000000000000000000, 0.9510565162951535312, 1.000000000000000000, 0.9510565162951535312, 1.000000000000000000, 0.9510565162951535312, 1.000000000000000000, 0.9510565162951535312, 1.000000000000000000, 0.9510565162951535312, 1.000000000000000000, 0.9510565162951535312, 1.000000000000000000, 0.9510565162951535312, 1.000000000000000000, 0.9510565162951535312, 1.000000000000000000, 0.9510565162951535312, 1.000000000000000000, 0.9510565162951535312, 1.000000000000000000, 0.9510565162951535312, 1.000000000000000000, 0.9510565162951535312, 1.000000000000000000, 0.9510565162951535312, 1.000000000000000000, 0.9510565162951535312, 1.000000000000000000, 0.9510565162951535312, 1.000000000000000000, 0.9510565162951535312, 1.000000000000000000, 0.9510565162951535312, 1.000000000000000000, 0.9510565162951535312, 1.000000000000000000, 0.9510565162951535312, 1.000000000000000000, 0.9510565162951535312, 1.000000000000000000, 0.9510565162951535312, 1.000000000000000000, 0.9510565162951535312, 1.000000000000000000, 0.9510565162951535312, 1.000000000000000000, 0.9510565162951535312, 1.000000000000000000, 0.9510565162951535312, 1.000000000000000000, 0.9510565162951535312, 1.000000000000000000, 0.9510565162951535312, 1.000000000000000000, 0.9510565162951535312, 1.000000000000000000, 0.9510565162951535312, 1.000000000000000000, 0.9510565162951535312, 1.000000000000000000, 0.9510565162951535312, 1.000000000000000000, 0.9510565162951535312, 1.000000000000000000, 0.9510565162951535312, 1.000000000000000000, 0.9510565162951535312, 1.000000000000000000, 0.9510565162951535312, 1.000000000000000000, 0.9510565162951535312, 1.000000000000000000, 0.9510565162951535312, 1.000000000000000000, 0.9510565162951535312, 1.000000000000000000, 0.9510565162951535312, 1.000000000000000000, 0.9510565162951535312, 1.000000000000000000, 0.9510565162951535312, 1.000000000000000000, 0.9510565162951535312, 1.000000000000000000, 0.9510565162951535312, 1.000000000000000000, 0.9510565162951535312, 1.000000000000000000, 0.9510565162951535312, 1.000000000000000000, 0.9510565162951535312, 1.000000000000000000, 0.9510565162951535312, 1.000000000000000000, 0.9510565162951535312, 1.000000000000000000, 0.9510565162951535312, 1.000000000000000000, 0.9510565162951535312, 1.000000000000000000, 0.9510565162951535312, 1.000000000000000000, 0.9510565162951535312, 1.000000000000000000, 0.9510565162951535312, 1.000000000000000000, 0.9510565162951535312, 1.000000000000000000, 0.9510565162951535312, 1.000000000000000000, 0.9510565162951535312, 1.000000000000000000, 0.9510565162951535312, 1.000000000000000000, 0.9510565162951535312, 1.000000000000000000, 0.9510565162951535312, 1.000000000000000000, 0.9510565162951535312, 1.000000000000000000, 0.9510565162951535312, 1.000000000000000000, 0.9510565162951535312, 1.000000000000000000, 0.9510565162951535312, 1.000000000000000000, 0.9510565162951535312, 1.000000000000000000, 0.9510565162951535312, 1.000000000000000000, 0.9510565162951535312, 1.000000000000000000, 0.9510565162951535312, 1.000000000000000000, 0.9510565162951535312, 1.000000000000000000, 0.9510565162951535312, 1.000000000000000000, 0.9510565162951535312, 1.000000000000000000, 0.9510565162951535312, 1.000000000000000000, 0.9510565162951535312, 1.000000000000000000, 0.9510565162951535312, 1.000000000000000000, 0.9510565162951535312, 1.000000000000000000, 0.9510565162951535312, 1.000000000000000000, 0.9510565162951535312, 1.000000000000000000, 0.9510565162951535312, 1.000000000000000000, 0.9510565162951535312, 1.000000000000000000, 0.9510565162951535312, 1.000000000000000000, 0.9510565162951535312, 1.000000000000000000, 0.9510565162951535312, 1.000000000000000000, 0.9510565162951535312, 1.000000000000000000, 0.9510565162951535312, 1.000000000000000000, 0.9510565162951535312, 1.000000000000000000, 0.9510565162951535312, 1.000000000000000000, 0.9510565162951535312, 1.000000000000000000, 0.9510565162951535312, 1.000000000000000000, 0.9510565162951535312, 1.000000000000000000, 0.9510565162951535312, 1.000000000000000000, 0.9510565162951535312, 1.000000000000000000, 0.9510565162951535312, 1.000000000000000000, 0.9510565162951535312, 1.000000000000000000, 0.9510565162951535312, 1.000000000000000000, 0.9510565162951535312, 1.000000000000000000, 0.9510565162951535312, 1.000000000000000000, 0.9510565162951535312, 1.000000000000000000, 0.9510565162951535312, 1.000000000000000000, 0.9510565162951535312, 1.000000000000000000, 0.9510565162951535312, 1.000000000000000000, 0.9510565162951535312, 1.000000000000000000, 0.9510565162951535312, 1.000000000000000000, 0.9510565162951535312, 1.000000000000000000, 0.9510565162951535312, 1.000000000000000000, 0.9510565162951535312, 1.000000000000000000, 0.9510565162951535312, 1.000000000000000000, 0.9510565162951535312, 1.000000000000000000, 0.9510565162951535312, 1.000000000000000000, 0.9510565162951535312, 1.000000000000000000, 0.9510565162951535312, 1.000000000000000000, 0.9510565162951535312, 1.000000000000000000, 0.9510565162951535312, 1.000000000000000000, 0.9510565162951535312, 1.000000000000000000, 0.9510565162951535312, 1.000000000000000000, 0.9510565162951535312, 1.000000000000000000, 0.9510565162951535312, 1.000000000000000000, 0.9510565162951535312, 1.000000000000000000, 0.9510565162951535312, 1.000000000000000000, 0.9510565162951535312, 1.000000000000000000, 0.9510565162951535312, 1.000000000000000000, 0.9510565162951535312, 1.000000000000000000, 0.9510565162951535312, 1.000000000000000000, 0.9510565162951535312, 1.000000000000000000, 0.9510565162951535312, 1.000000000000000000, 0.9510565162951535312, 1.000000000000000000, 0.9510565162951535312, 1.000000000000000000, 0.9510565162951535312, 1.000000000000000000, 0.9510565162951535312, 1.000000000000000000, 0.9510565162951535312, 1.000000000000000000, 0.9510565162951535312, 1.000000000000000000, 0.9510565162951535312, 1.000000000000000000, 0.9510565162951535312, 1.000000000000000000, 0.9510565162951535312, 1.000000000000000000, 0.9510565162951535312, 1.000000000000000000, 0.9510565162951535312, 1.000000000000000000, 0.9510565162951535312, 1.000000000000000000, 0.9510565162951535312, 1.000000000000000000, 0.9510565162951535312, 1.000000000000000000, 0.9510565162951535312, 1.000000000000000000, 0.9510565162951535312, 1.000000000000000000, 0.9510565162951535312, 1.000000000000000000, 0.9510565162951535312, 1.000000000000000000, 0.9510565162951535312, 1.000000000000000000, 0.9510565162951535312, 1.000000000000000000, 0.9510565162951535312, 1.000000000000000000, 0.9510565162951535312, 1.000000000000000000, 0.9510565162951535312, 1.000000000000000000, 0.9510565162951535312, 1.000000000000000000, 0.9510565162951535312, 1.000000000000000000, 0.9510565162951535312, 1.000000000000000000, 0.9510565162951535312, 1.000000000000000000, 0.9510565162951535312, 1.000000000000000000, 0.9510565162951535312, 1.000000000000000000, 0.9510565162951535312, 1.000000000000000000, 0.9510565162951535312, 1.000000000000000000, 0.9510565162951535312, 1.000000000000000000, 0.9510565162951535312, 1.000000000000000000, 0.9510565162951535312, 1.000000000000000000, 0.9510565162951535312, 1.000000000000000000, 0.9510565162951535312, 1.000000000000000000, 0.9510565162951535312, 1.000000000000000000, 0.9510565162951535312, 1.000000000000000000, 0.9510565162951535312, 1.000000000000000000, 0.9510565162951535312, 1.000000000000000000, 0.9510565162951535312, 1.000000000000000000, 0.9510565162951535312, 1.000000000000000000, 0.9510565162951535312, 1.000000000000000000, 0.9510565162951535312, 1.000000000000000000, 0.9510565162951535312, 1.000000000000000000, 0.9510565162951535312, 1.000000000000000000, 0.9510565162951535312, 1.000000000000000000, 0.9510565162951535312, 1.000000000000000000, 0.9510565162951535312, 1.000000000000000000, 0.9510565162951535312, 1.000000000000000000, 0.9510565162951535312, 1.000000000000000000, 0.9510565162951535312, 1.000000000000000000, 0.9510565162951535312, 1.000000000000000000, 0.9510565162951535312, 1.000000000000000000, 0.9510565162951535312, 1.000000000000000000, 0.9510565162951535312, 1.000000000000000000, 0.9510565162951535312, 1.000000000000000000, 0.9510565162951535312, 1.000000000000000000, 0.9510565162951535312, 1.000000000000000000, 1.000000000000000000, 1.000000000000000000) ) ) 
 REPRESENTATION_ITEM ( '' )  SURFACE ( )  );
#21390 = CARTESIAN_POINT ( 'NONE',  ( 4.984841277089891776, 200.2242689037093726, 58.44886208192144039 ) ) ;
#21391 = VECTOR ( 'NONE', #1737, 1000.000000000000000 ) ;
#21392 = ORIENTED_EDGE ( 'NONE', *, *, #16983, .T. ) ;
#21393 = ADVANCED_FACE ( 'NONE', ( #12483 ), #4305, .T. ) ;
#21394 = VECTOR ( 'NONE', #23956, 1000.000000000000000 ) ;
#21395 = CARTESIAN_POINT ( 'NONE',  ( 79.72499999726881015, 169.8198683612136222, 4.815267126137181997 ) ) ;
#21396 = ORIENTED_EDGE ( 'NONE', *, *, #7071, .F. ) ;
#21397 = CYLINDRICAL_SURFACE ( 'NONE', #16244, 15.00000000000001776 ) ;
#21398 = ADVANCED_FACE ( 'NONE', ( #1741 ), #17588, .T. ) ;
#21399 = CARTESIAN_POINT ( 'NONE',  ( 72.32499999726880446, 145.8408176439707802, 12.60653300113718345 ) ) ;
#21400 = CARTESIAN_POINT ( 'NONE',  ( -2.426778023690262742, 214.6231898156240163, 73.10113791807857808 ) ) ;
#21401 = DIRECTION ( 'NONE',  ( -0.9945218953682687379, 1.280104479605762779E-17, -0.1045284632676965614 ) ) ;
#21402 = CARTESIAN_POINT ( 'NONE',  ( -6.830473686658677934E-14, -4.041451884327390331, -2.587392608830344720 ) ) ;
#21403 = AXIS2_PLACEMENT_3D ( 'NONE', #32454, #14912, #14737 ) ;
#21404 = FILL_AREA_STYLE_COLOUR ( '', #263 ) ;
#21405 = CARTESIAN_POINT ( 'NONE',  ( 36.29999999999999716, 146.4771138417591203, -11.73074641843674470 ) ) ;
#21406 = COLOUR_RGB ( '', 0.72549020, 0.75294118, 0.79215686) ;
#21407 = CARTESIAN_POINT ( 'NONE',  ( -2.517493886309087880, 214.5937144450984135, 42.09886208192144608 ) ) ;
#21408 = CARTESIAN_POINT ( 'NONE',  ( 6.139770520408368348, 198.4640165459539674, 80.45113791807857240 ) ) ;
#21409 = CARTESIAN_POINT ( 'NONE',  ( -3.135527875058821579, 197.5041725223112223, 65.90113791807857524 ) ) ;
#21410 = DIRECTION ( 'NONE',  ( 1.000000000000000000, 0.000000000000000000, -0.000000000000000000 ) ) ;
#21411 = CARTESIAN_POINT ( 'NONE',  ( 6.500168698208129925, 211.6636982574063381, 25.70113791807857240 ) ) ;
#21412 = CARTESIAN_POINT ( 'NONE',  ( 127.6439996469472504, -4.587378538859826271, 35.00001200000000523 ) ) ;
#21413 = AXIS2_PLACEMENT_3D ( 'NONE', #17092, #11977, #9585 ) ;
#21414 = DIRECTION ( 'NONE',  ( 0.3362851123284906207, 0.04491457122451913281, 0.9406885799869860731 ) ) ;
#21415 = CARTESIAN_POINT ( 'NONE',  ( 45.92499999726881299, 164.1591823560292198, 12.60653300113718167 ) ) ;
#21416 = CARTESIAN_POINT ( 'NONE',  ( 0.05014649552807549926, 219.6175466908591716, 46.25113791807856956 ) ) ;
#21417 = CARTESIAN_POINT ( 'NONE',  ( -5.000000000000000888, 6.123233995736767268E-16, 0.000000000000000000 ) ) ;
#21418 = CIRCLE ( 'NONE', #20896, 2.499999999999988454 ) ;
#21419 = CARTESIAN_POINT ( 'NONE',  ( 9.984503880673470277, 203.7031108863295401, 95.15113791807854682 ) ) ;
#21420 = CARTESIAN_POINT ( 'NONE',  ( -3.044812012440131443, 216.5253028482142952, 64.10113791807857808 ) ) ;
#21421 = CARTESIAN_POINT ( 'NONE',  ( -7.456977232089471386, 217.1783343296987709, 29.94886208192143684 ) ) ;
#21422 = CARTESIAN_POINT ( 'NONE',  ( 9.984503880673420539, 210.2968891136705736, 42.84886208192143897 ) ) ;
#21423 = CARTESIAN_POINT ( 'NONE',  ( 80.79999999453762882, 163.5228861582408797, 11.73074641843673049 ) ) ;
#21424 = CARTESIAN_POINT ( 'NONE',  ( 9.736236675707914401, 214.0148392665762458, 76.70113791807857240 ) ) ;
#21425 = CARTESIAN_POINT ( 'NONE',  ( 2.517493886308900919, 214.5937144450984420, 88.40113791807857524 ) ) ;
#21426 = EDGE_CURVE ( 'NONE', #31727, #6290, #14859, .T. ) ;
#21427 = CARTESIAN_POINT ( 'NONE',  ( 8.062137200540822946, 212.9164362838583315, 45.69886208192143329 ) ) ;
#21428 = CARTESIAN_POINT ( 'NONE',  ( 99.99999999999998579, 0.000000000000000000, 0.000000000000000000 ) ) ;
#21429 = VERTEX_POINT ( 'NONE', #33091 ) ;
#21430 = CARTESIAN_POINT ( 'NONE',  ( -12.00000000000000711, 206.9523078486584780, 59.49886208192143044 ) ) ;
#21431 = COLOUR_RGB ( '', 0.66274510, 0.83137255, 0.94901961) ;
#21432 = EDGE_LOOP ( 'NONE', ( #28521, #11173, #8998, #22016, #30832, #7999 ) ) ;
#21433 = CARTESIAN_POINT ( 'NONE',  ( -7.984503880673422316, 204.3529502787951628, 29.34886208192143897 ) ) ;
#21434 = VERTEX_POINT ( 'NONE', #7202 ) ;
#21435 = EDGE_CURVE ( 'NONE', #30624, #30017, #11073, .T. ) ;
#21436 = CARTESIAN_POINT ( 'NONE',  ( 76.17499999726881299, 164.1591823560292198, 12.60653300113718167 ) ) ;
#21437 = CARTESIAN_POINT ( 'NONE',  ( 53.31132485994280756, 140.7341522555726669, -4.635254915624220651 ) ) ;
#21438 = DIRECTION ( 'NONE',  ( -0.000000000000000000, 1.295896757998781572E-15, 1.000000000000000000 ) ) ;
#21439 =( GEOMETRIC_REPRESENTATION_CONTEXT ( 3 ) GLOBAL_UNCERTAINTY_ASSIGNED_CONTEXT ( ( #15786 ) ) GLOBAL_UNIT_ASSIGNED_CONTEXT ( ( #15345, #15513, #31355 ) ) REPRESENTATION_CONTEXT ( 'NONE', 'WORKASPACE' ) );
#21440 = CARTESIAN_POINT ( 'NONE',  ( -8.015496119326531499, 204.4483345814780364, 51.35113791807857098 ) ) ;
#21441 = CIRCLE ( 'NONE', #28517, 2.149999999999985256 ) ;
#21442 = ADVANCED_FACE ( 'NONE', ( #11971 ), #32745, .F. ) ;
#21443 =( NAMED_UNIT ( * ) SI_UNIT ( $, .STERADIAN. ) SOLID_ANGLE_UNIT ( ) );
#21444 = CARTESIAN_POINT ( 'NONE',  ( 3.044812012439969795, 216.5253028482143520, 33.39886208192143613 ) ) ;
#21445 = CARTESIAN_POINT ( 'NONE',  ( 68.47499999726879594, 149.9369285172503510, 15.58253174999999580 ) ) ;
#21446 = ORIENTED_EDGE ( 'NONE', *, *, #28045, .T. ) ;
#21447 = CARTESIAN_POINT ( 'NONE',  ( 41.38867513459481984, 169.2658477444273331, 4.635254915624208216 ) ) ;
#21448 = CARTESIAN_POINT ( 'NONE',  ( 1.500000000000001332, 0.000000000000000000, 0.000000000000000000 ) ) ;
#21449 = CARTESIAN_POINT ( 'NONE',  ( 0.05014649552828262524, 198.5883022060938572, 13.74886208192143577 ) ) ;
#21450 = CARTESIAN_POINT ( 'NONE',  ( 10.01549611932653860, 210.2015048109876716, 55.85113791807857808 ) ) ;
#21451 = CARTESIAN_POINT ( 'NONE',  ( 83.68867513459485963, 159.8737954434934636, 15.00000000000014211 ) ) ;
#21452 = CARTESIAN_POINT ( 'NONE',  ( 6.220909254589536808, 215.4770327129947702, 40.55113791807855250 ) ) ;
#21453 = CARTESIAN_POINT ( 'NONE',  ( 87.77499999726882152, 169.8198683612136222, -4.815267126137197984 ) ) ;
#21454 = ITEM_DEFINED_TRANSFORMATION ( 'NONE', 'NONE', #10489,  #2404 ) ;
#21455 =( GEOMETRIC_REPRESENTATION_CONTEXT ( 3 ) GLOBAL_UNCERTAINTY_ASSIGNED_CONTEXT ( ( #17525 ) ) GLOBAL_UNIT_ASSIGNED_CONTEXT ( ( #12784, #31345, #13437 ) ) REPRESENTATION_CONTEXT ( 'NONE', 'WORKASPACE' ) );
#21456 = CARTESIAN_POINT ( 'NONE',  ( 2.517493886309087436, 199.4062855549015865, 88.59886208192143897 ) ) ;
#21457 = CARTESIAN_POINT ( 'NONE',  ( 36.12499999726881583, 155.0000000000000000, 15.58253174999999402 ) ) ;
#21458 = CARTESIAN_POINT ( 'NONE',  ( 80.78867513459482552, 155.0000000000000000, -15.00000000000002487 ) ) ;
#21459 = DIRECTION ( 'NONE',  ( -0.000000000000000000, -0.000000000000000000, -1.000000000000000000 ) ) ;
#21460 = CARTESIAN_POINT ( 'NONE',  ( -12.01549611932652972, 203.1486557965464499, 24.35113791807856742 ) ) ;
#21461 = CARTESIAN_POINT ( 'NONE',  ( 2.352174619736673744, -7.302225387959338399, -7.450218641350605076 ) ) ;
#21462 = CARTESIAN_POINT ( 'NONE',  ( 59.37499999726881583, 155.0000000000000000, -15.58253175000000823 ) ) ;
#21463 = CARTESIAN_POINT ( 'NONE',  ( 8.118202686958039038, 212.8392687619912635, 70.70113791807857240 ) ) ;
#21464 = CARTESIAN_POINT ( 'NONE',  ( -9.984503880673475606, 210.2968891136704315, 42.65113791807856813 ) ) ;
#21465 = DIRECTION ( 'NONE',  ( -1.000000000000000000, -0.000000000000000000, -0.000000000000000000 ) ) ;
#21466 = CARTESIAN_POINT ( 'NONE',  ( -7.500000000000000000, -2.886751345948133984, -7.198902722707428481 ) ) ;
#21467 = CARTESIAN_POINT ( 'NONE',  ( -8.118202686958138514, 212.8392687619910930, 11.79886208192143471 ) ) ;
#21468 = CARTESIAN_POINT ( 'NONE',  ( 62.39999999453763024, 168.7903194862797420, -4.480746418436745593 ) ) ;
#21469 = ORIENTED_EDGE ( 'NONE', *, *, #23908, .T. ) ;
#21470 = CARTESIAN_POINT ( 'NONE',  ( -12.01549611932652972, 203.1486557965464499, 45.35113791807857098 ) ) ;
#21471 = DIRECTION ( 'NONE',  ( 1.000000000000000000, 0.000000000000000000, 0.000000000000000000 ) ) ;
#21472 = CARTESIAN_POINT ( 'NONE',  ( 3.135527875058981895, 197.5041725223112792, 19.59886208192143542 ) ) ;
#21473 = ADVANCED_FACE ( 'NONE', ( #14035 ), #881, .F. ) ;
#21474 = FACE_OUTER_BOUND ( 'NONE', #2049, .T. ) ;
#21475 = ORIENTED_EDGE ( 'NONE', *, *, #23673, .T. ) ;
#21476 = CARTESIAN_POINT ( 'NONE',  ( 9.984503880673470277, 203.7031108863295401, 83.15113791807853261 ) ) ;
#21477 = ORIENTED_EDGE ( 'NONE', *, *, #5814, .F. ) ;
#21478 = EDGE_CURVE ( 'NONE', #31012, #20137, #12926, .T. ) ;
#21479 = CARTESIAN_POINT ( 'NONE',  ( 127.5000000000000000, 154.9999999999996305, -106.0000000000000142 ) ) ;
#21480 = CARTESIAN_POINT ( 'NONE',  ( -5.727634848076946561, -4.575561887448768239, -6.326622577870699260 ) ) ;
#21481 = ORIENTED_EDGE ( 'NONE', *, *, #24347, .F. ) ;
#21482 = CARTESIAN_POINT ( 'NONE',  ( 4.984841277089725686, 213.7757310962907411, 22.55113791807857027 ) ) ;
#21483 = CARTESIAN_POINT ( 'NONE',  ( -60.38481630464774241, 194.9660974499433053, -1.650668498912690740 ) ) ;
#21484 = CARTESIAN_POINT ( 'NONE',  ( -12.10169002831357510, 232.5389149829038331, 105.4832055762867782 ) ) ;
#21485 = CARTESIAN_POINT ( 'NONE',  ( 43.47499999726881015, 160.0630714827496206, -15.58253175000000823 ) ) ;
#21486 = EDGE_LOOP ( 'NONE', ( #123, #23504, #32583, #22828 ) ) ;
#21487 = CARTESIAN_POINT ( 'NONE',  ( 56.12499999726880873, 155.0000000000000000, 15.58253174999999402 ) ) ;
#21488 = CARTESIAN_POINT ( 'NONE',  ( 77.50000000000000000, 155.0000000000000000, 15.50000000000000355 ) ) ;
#21489 = CARTESIAN_POINT ( 'NONE',  ( 60.88867513459483405, 159.8737954434936910, -14.99999999999998046 ) ) ;
#21490 = CARTESIAN_POINT ( 'NONE',  ( 0.3999999999999975797, 7.470345474798854293E-16, -6.099999999999999645 ) ) ;
#21491 = CARTESIAN_POINT ( 'NONE',  ( -3.044812012439970683, 197.4746971517856196, 79.89886208192143613 ) ) ;
#21492 = CARTESIAN_POINT ( 'NONE',  ( 54.87499999726880162, 138.6155565068815463, -3.929120461958505118E-15 ) ) ;
#21493 = CARTESIAN_POINT ( 'NONE',  ( 9.984503880673470277, 203.7031108863295401, 23.15113791807856813 ) ) ;
#21494 = CARTESIAN_POINT ( 'NONE',  ( -12.00000000000000711, 206.9523078486584780, 77.49886208192144466 ) ) ;
#21495 = CARTESIAN_POINT ( 'NONE',  ( 74.40000000000000568, 150.2886644046228639, -14.50000000000000888 ) ) ;
#21496 = CARTESIAN_POINT ( 'NONE',  ( 65.58867513459482268, 163.8167787843871110, 12.13525491562421621 ) ) ;
#21497 = FACE_OUTER_BOUND ( 'NONE', #17670, .T. ) ;
#21498 = CARTESIAN_POINT ( 'NONE',  ( 0.05014649552810505201, 217.5146222423826714, 94.25113791807855534 ) ) ;
#21499 = DIRECTION ( 'NONE',  ( 1.000000000000000000, 0.000000000000000000, 0.000000000000000000 ) ) ;
#21500 = CARTESIAN_POINT ( 'NONE',  ( 36.67499999726879878, 141.7447067706911810, 9.630534252274376428 ) ) ;
#21501 = CARTESIAN_POINT ( 'NONE',  ( -6.139770520408369237, 215.5359834540460042, 39.95113791807857240 ) ) ;
#21502 = CARTESIAN_POINT ( 'NONE',  ( 77.72499999726881015, 169.8198683612136222, 4.815267126137181997 ) ) ;
#21503 = ORIENTED_EDGE ( 'NONE', *, *, #7071, .T. ) ;
#21504 = CARTESIAN_POINT ( 'NONE',  ( 48.11132485994281183, 169.2658477444273331, -4.635254915624224203 ) ) ;
#21505 = CARTESIAN_POINT ( 'NONE',  ( 39.29999999453762882, 142.6655632788954620, 8.961492836873471646 ) ) ;
#21506 = CARTESIAN_POINT ( 'NONE',  ( -3.662846001190052991, 218.4274158808045740, 7.101137918078566535 ) ) ;
#21507 = PRODUCT_DEFINITION_SHAPE ( 'NONE', 'NONE',  #33705 ) ;
#21508 = DIRECTION ( 'NONE',  ( 0.000000000000000000, 0.000000000000000000, 1.000000000000000000 ) ) ;
#21509 = CARTESIAN_POINT ( 'NONE',  ( 3.499999999999999556, 0.000000000000000000, 0.000000000000000000 ) ) ;
#21510 = ORIENTED_EDGE ( 'NONE', *, *, #19724, .T. ) ;
#21511 = CARTESIAN_POINT ( 'NONE',  ( 3.044812012439969795, 216.5253028482143520, 93.39886208192143613 ) ) ;
#21512 = CARTESIAN_POINT ( 'NONE',  ( -7.375838497908014268, 196.7627149292498530, 29.04886208192143471 ) ) ;
#21513 = CARTESIAN_POINT ( 'NONE',  ( -10.40947905833197673, 207.8831653815483662, 102.6241284678525432 ) ) ;
#21514 = CARTESIAN_POINT ( 'NONE',  ( 8.062137200540920645, 201.0835637161417822, 56.30113791807857382 ) ) ;
#21515 = EDGE_LOOP ( 'NONE', ( #1114, #33687 ) ) ;
#21516 = CARTESIAN_POINT ( 'NONE',  ( -2.426778023690076225, 199.3768101843759553, 10.89886208192143613 ) ) ;
#21517 = CARTESIAN_POINT ( 'NONE',  ( -19.55945325266601031, -20.46160920480082623, -17.55088044235631983 ) ) ;
#21518 = ORIENTED_EDGE ( 'NONE', *, *, #2040, .T. ) ;
#21519 = CARTESIAN_POINT ( 'NONE',  ( 7.984503880673422316, 209.6470497212048372, 87.84886208192142476 ) ) ;
#21520 = CARTESIAN_POINT ( 'NONE',  ( 2.426778023690261410, 199.3768101843759837, 41.60113791807857808 ) ) ;
#21521 = CARTESIAN_POINT ( 'NONE',  ( 2.000000000000000000, -0.8865213383406685965, 1.535500000000000531 ) ) ;
#21522 = VERTEX_POINT ( 'NONE', #29707 ) ;
#21523 = CARTESIAN_POINT ( 'NONE',  ( 1.060314165522845187, 8.048081368953960535, -7.659344964963204383 ) ) ;
#21524 = CARTESIAN_POINT ( 'NONE',  ( 86.92499999726881299, 145.8408176439707802, -12.60653300113719588 ) ) ;
#21525 = CARTESIAN_POINT ( 'NONE',  ( 107.9108275708642850, 155.0000000000000000, 0.000000000000000000 ) ) ;
#21526 = CARTESIAN_POINT ( 'NONE',  ( -8.000000000000008882, 207.0476921513413515, 96.50113791807856956 ) ) ;
#21527 = DIRECTION ( 'NONE',  ( 1.000000000000000000, 0.000000000000000000, 0.000000000000000000 ) ) ;
#21528 = CARTESIAN_POINT ( 'NONE',  ( 53.79999999999999005, 142.6655632788954620, 8.961492836873471646 ) ) ;
#21529 = CARTESIAN_POINT ( 'NONE',  ( -8.015496119326597224, 209.5516654185217362, 71.64886208192143613 ) ) ;
#21530 = CARTESIAN_POINT ( 'NONE',  ( 4.000000000000000000, -1.759474945355381958, 3.047500000000001208 ) ) ;
#21531 =( BOUNDED_CURVE ( )  B_SPLINE_CURVE ( 2, ( #9508, #19732, #23097, #17988, #30129, #4868, #25019, #32845, #17350, #19395, #24511 ),
 .UNSPECIFIED., .F., .T. ) 
 B_SPLINE_CURVE_WITH_KNOTS ( ( 3, 2, 2, 2, 2, 3 ),
 ( 0.3571428571428569287, 0.3607142857142854875, 0.3642857142857140462, 0.3678571428571425495, 0.3714285714285711082, 0.3749999999999997780 ),
 .UNSPECIFIED. ) 
 CURVE ( )  GEOMETRIC_REPRESENTATION_ITEM ( )  RATIONAL_B_SPLINE_CURVE ( ( 1.000000000000002220, 0.9510565162951510887, 1.000000000000000000, 0.9510565162951534202, 1.000000000000000000, 0.9510565162951534202, 1.000000000000000000, 0.9510565162951534202, 1.000000000000000000, 0.9510565162951564178, 0.9999999999999970024 ) ) 
 REPRESENTATION_ITEM ( '' )  );
#21532 = CARTESIAN_POINT ( 'NONE',  ( 60.82499999726881867, 141.7447067706911810, -9.630534252274385310 ) ) ;
#21533 = CARTESIAN_POINT ( 'NONE',  ( -0.05014649552810635652, 196.4853777576173002, 8.751137918078567779 ) ) ;
#21534 = CARTESIAN_POINT ( 'NONE',  ( 79.78867513459482552, 155.0000000000000000, 15.00000000000001243 ) ) ;
#21535 = CARTESIAN_POINT ( 'NONE',  ( 62.92499999726880588, 145.8408176439707802, -12.60653300113719588 ) ) ;
#21536 = CARTESIAN_POINT ( 'NONE',  ( 74.17499999726881299, 164.1591823560292198, 12.60653300113718167 ) ) ;
#21537 = CARTESIAN_POINT ( 'NONE',  ( 7.375838497908181246, 196.7627149292499666, 80.45113791807857240 ) ) ;
#21538 = CARTESIAN_POINT ( 'NONE',  ( 9.984503880673473830, 203.7031108863295401, 101.1511379180785752 ) ) ;
#21539 = LINE ( 'NONE', #18997, #3638 ) ;
#21540 = AXIS2_PLACEMENT_3D ( 'NONE', #30958, #28224, #33499 ) ;
#21541 = EDGE_LOOP ( 'NONE', ( #20563, #11669 ) ) ;
#21542 = CARTESIAN_POINT ( 'NONE',  ( -3.135527875058982783, 216.4958274776886924, 6.098862081921434530 ) ) ;
#21543 = CARTESIAN_POINT ( 'NONE',  ( -3.662846001189865142, 195.5725841191952838, 64.89886208192143613 ) ) ;
#21544 = CARTESIAN_POINT ( 'NONE',  ( 0.05014649552828275014, 196.4853777576173002, 64.74886208192143044 ) ) ;
#21545 = CARTESIAN_POINT ( 'NONE',  ( -7.456977232089471386, 217.1783343296987709, 8.948862081921433287 ) ) ;
#21546 = CYLINDRICAL_SURFACE ( 'NONE', #7769, 5.200000000000009948 ) ;
#21547 = CARTESIAN_POINT ( 'NONE',  ( -9.984503880673473830, 210.2968891136704315, 18.65113791807856813 ) ) ;
#21548 = CARTESIAN_POINT ( 'NONE',  ( -10.01549611932659722, 210.2015048109875011, 86.64886208192139350 ) ) ;
#21549 = ORIENTED_EDGE ( 'NONE', *, *, #3474, .T. ) ;
#21550 = CARTESIAN_POINT ( 'NONE',  ( -125.0000000000000000, -95.00000000000000000, 20.00000000000001776 ) ) ;
#21551 = ORIENTED_EDGE ( 'NONE', *, *, #2095, .T. ) ;
#21552 = CARTESIAN_POINT ( 'NONE',  ( -8.015496119326597224, 209.5516654185217362, 59.64886208192145034 ) ) ;
#21553 = ORIENTED_EDGE ( 'NONE', *, *, #10381, .F. ) ;
#21554 = EDGE_CURVE ( 'NONE', #17667, #31655, #3599, .T. ) ;
#21555 = CARTESIAN_POINT ( 'NONE',  ( 77.02499999726880731, 149.9369285172503510, -15.58253175000000823 ) ) ;
#21556 = ORIENTED_EDGE ( 'NONE', *, *, #9577, .F. ) ;
#21557 = CARTESIAN_POINT ( 'NONE',  ( 121.3406204335659879, 155.0000000000000000, 7.500000000000007994 ) ) ;
#21558 = UNCERTAINTY_MEASURE_WITH_UNIT (LENGTH_MEASURE( 1.000000000000000082E-05 ), #32821, 'distance_accuracy_value', 'NONE');
#21559 = CARTESIAN_POINT ( 'NONE',  ( 72.72499999726881015, 140.1801316387863778, -4.815267126137194431 ) ) ;
#21560 = CARTESIAN_POINT ( 'NONE',  ( 6.444103211791042618, 202.2591342207267644, 68.30113791807856671 ) ) ;
#21561 = AXIS2_PLACEMENT_3D ( 'NONE', #5051, #16063, #31895 ) ;
#21562 = DIRECTION ( 'NONE',  ( 0.000000000000000000, -0.5000000000000009992, -0.8660254037844380415 ) ) ;
#21563 = FILL_AREA_STYLE ('',( #21404 ) ) ;
#21564 = CARTESIAN_POINT ( 'NONE',  ( 34.80000000000000426, 167.3344367211045096, -8.961492836873482304 ) ) ;
#21565 = CARTESIAN_POINT ( 'NONE',  ( 8.015496119326595448, 204.4483345814782638, 46.14886208192143613 ) ) ;
#21566 = CARTESIAN_POINT ( 'NONE',  ( -6.220909254589537696, 198.5229672870051161, 78.05113791807858092 ) ) ;
#21567 = CARTESIAN_POINT ( 'NONE',  ( -9.984503880673473830, 210.2968891136704315, 66.65113791807857524 ) ) ;
#21568 = CIRCLE ( 'NONE', #19189, 2.466666666666999408 ) ;
#21569 = CARTESIAN_POINT ( 'NONE',  ( 95.70416941062676131, 155.0000000000000000, 0.000000000000000000 ) ) ;
#21570 = CARTESIAN_POINT ( 'NONE',  ( -4.903702542908602524, 213.8346818373418898, 24.95113791807856884 ) ) ;
#21571 = CARTESIAN_POINT ( 'NONE',  ( 2.500000000000000444, 7.216878364870322748, -7.063244554130000630 ) ) ;
#21572 = CARTESIAN_POINT ( 'NONE',  ( -4.424031367838696660, 4.951337798339958240, -6.056431503346038525 ) ) ;
#21573 = CARTESIAN_POINT ( 'NONE',  ( 46.02499999726880731, 160.0630714827496206, 15.58253174999999224 ) ) ;
#21574 = CARTESIAN_POINT ( 'NONE',  ( 9.736236675707914401, 214.0148392665762458, 43.70113791807857240 ) ) ;
#21575 = FACE_OUTER_BOUND ( 'NONE', #11209, .T. ) ;
#21576 = CARTESIAN_POINT ( 'NONE',  ( -6.220909254589537696, 198.5229672870051161, 96.05113791807858092 ) ) ;
#21577 = CARTESIAN_POINT ( 'NONE',  ( 8.062137200540920645, 201.0835637161417822, 71.30113791807856671 ) ) ;
#21578 = CARTESIAN_POINT ( 'NONE',  ( -9.680171189290716072, 199.9079932115567146, 32.19886208192144039 ) ) ;
#21579 = CARTESIAN_POINT ( 'NONE',  ( 8.118202686958138514, 201.1607312380088501, 37.29886208192143471 ) ) ;
#21580 = CARTESIAN_POINT ( 'NONE',  ( 87.39999999453762314, 141.2096805137202580, 4.480746418436733158 ) ) ;
#21581 = CARTESIAN_POINT ( 'NONE',  ( 7.375838497908181246, 196.7627149292499666, 80.45113791807857240 ) ) ;
#21582 = AXIS2_PLACEMENT_3D ( 'NONE', #5977, #18934, #16364 ) ;
#21583 = CARTESIAN_POINT ( 'NONE',  ( -8.015496119326531499, 204.4483345814780364, 102.3511379180785639 ) ) ;
#21584 = EDGE_CURVE ( 'NONE', #19123, #1694, #9598, .T. ) ;
#21585 = CARTESIAN_POINT ( 'NONE',  ( -3.044812012439970683, 197.4746971517856196, 49.89886208192143613 ) ) ;
#21586 = CIRCLE ( 'NONE', #5282, 12.00000000000001066 ) ;
#21587 = CARTESIAN_POINT ( 'NONE',  ( -1.650000000000000133, 2.020667218593133001E-16, -2.629527361626598836 ) ) ;
#21588 = ORIENTED_EDGE ( 'NONE', *, *, #20497, .F. ) ;
#21589 = CARTESIAN_POINT ( 'NONE',  ( 7.375838497908012492, 217.2372850707501186, 66.54886208192144181 ) ) ;
#21590 = VECTOR ( 'NONE', #10568, 1000.000000000000000 ) ;
#21591 = ORIENTED_EDGE ( 'NONE', *, *, #29173, .T. ) ;
#21592 = CARTESIAN_POINT ( 'NONE',  ( 6.500168698208244500, 202.3363017425938324, 28.29886208192143826 ) ) ;
#21593 = VERTEX_POINT ( 'NONE', #32938 ) ;
#21594 = EDGE_CURVE ( 'NONE', #7491, #26705, #9704, .T. ) ;
#21595 = AXIS2_PLACEMENT_3D ( 'NONE', #4350, #24460, #3670 ) ;
#21596 = CARTESIAN_POINT ( 'NONE',  ( 78.47499999726881015, 149.9369285172503510, 15.58253174999999580 ) ) ;
#21597 = CARTESIAN_POINT ( 'NONE',  ( 86.88867513459483405, 159.8737954434935489, -15.00000000000009237 ) ) ;
#21598 = LINE ( 'NONE', #10893, #19256 ) ;
#21599 = CARTESIAN_POINT ( 'NONE',  ( 4.903702542908601636, 200.1653181626581102, 56.45113791807857950 ) ) ;
#21600 = CARTESIAN_POINT ( 'NONE',  ( -9.984503880673420539, 203.7031108863293980, 29.34886208192144252 ) ) ;
#21601 = CARTESIAN_POINT ( 'NONE',  ( 70.37499999726881583, 155.0000000000000000, 15.58253174999999402 ) ) ;
#21602 = ORIENTED_EDGE ( 'NONE', *, *, #13220, .F. ) ;
#21603 = CARTESIAN_POINT ( 'NONE',  ( 64.50000000000000000, -73.00000000000000000, -30.00000000000000000 ) ) ;
#21604 = EDGE_CURVE ( 'NONE', #5932, #5597, #15647, .T. ) ;
#21605 =( NAMED_UNIT ( * ) PLANE_ANGLE_UNIT ( ) SI_UNIT ( $, .RADIAN. ) );
#21606 = CARTESIAN_POINT ( 'NONE',  ( 42.98867513459482836, 163.8167787843871110, -12.13525491562423397 ) ) ;
#21607 = CARTESIAN_POINT ( 'NONE',  ( -7.984503880673422316, 204.3529502787951628, 11.34886208192143542 ) ) ;
#21608 = AXIS2_PLACEMENT_3D ( 'NONE', #7639, #18022, #15465 ) ;
#21609 = CARTESIAN_POINT ( 'NONE',  ( -8.062137200540920645, 212.9164362838581894, 48.80113791807857382 ) ) ;
#21610 = CARTESIAN_POINT ( 'NONE',  ( 0.6511518506208960888, -8.763486134561278007, -7.907570769506051533 ) ) ;
#21611 = CARTESIAN_POINT ( 'NONE',  ( 8.118202686958039038, 212.8392687619912635, 37.70113791807857240 ) ) ;
#21612 = CARTESIAN_POINT ( 'NONE',  ( 82.17499999726882720, 164.1591823560292198, 12.60653300113718167 ) ) ;
#21613 = COLOUR_RGB ( '', 0.31764706, 0.68627451, 0.89019608) ;
#21614 = AXIS2_PLACEMENT_3D ( 'NONE', #24940, #8926, #6365 ) ;
#21615 = CARTESIAN_POINT ( 'NONE',  ( -8.000000000000008882, 206.9523078486584780, 104.4988620819214304 ) ) ;
#21616 = CARTESIAN_POINT ( 'NONE',  ( 36.02499999726881441, 160.0630714827496206, 15.58253174999999402 ) ) ;
#21617 = CARTESIAN_POINT ( 'NONE',  ( 80.88867513459481984, 159.8737954434937762, -14.99999999999989519 ) ) ;
#21618 = DIRECTION ( 'NONE',  ( 0.000000000000000000, 0.000000000000000000, 1.000000000000000000 ) ) ;
#21619 = CARTESIAN_POINT ( 'NONE',  ( -9.736236675707914401, 199.9851607334237542, 21.20113791807856529 ) ) ;
#21620 = CARTESIAN_POINT ( 'NONE',  ( 5.276498195232308674, -6.073236878017951312, -7.633618187056764981 ) ) ;
#21621 = CARTESIAN_POINT ( 'NONE',  ( 64.37499999726881583, 155.0000000000000000, 15.58253174999999402 ) ) ;
#21622 = EDGE_CURVE ( 'NONE', #26980, #14311, #9435, .T. ) ;
#21623 = CARTESIAN_POINT ( 'NONE',  ( 9.984503880673470277, 203.7031108863295401, 65.15113791807856103 ) ) ;
#21624 = CARTESIAN_POINT ( 'NONE',  ( -3.044812012440131443, 216.5253028482142952, 40.10113791807857098 ) ) ;
#21625 = AXIS2_PLACEMENT_3D ( 'NONE', #5037, #21035, #424 ) ;
#21626 = CARTESIAN_POINT ( 'NONE',  ( 3.750000000000005329, 6.495190528383288253, 0.000000000000000000 ) ) ;
#21627 = CARTESIAN_POINT ( 'NONE',  ( -4.506125120515186211, 29.15265225409784478, -16.90910675883083414 ) ) ;
#21628 = CARTESIAN_POINT ( 'NONE',  ( 3.753561863808876797, 195.6020594897209719, 1.598862081921433864 ) ) ;
#21629 = CARTESIAN_POINT ( 'NONE',  ( -8.062137200540822946, 201.0835637161416400, 8.198862081921435063 ) ) ;
#21630 = CARTESIAN_POINT ( 'NONE',  ( 58.79999999453762882, 163.5228861582408797, 11.73074641843673049 ) ) ;
#21631 = ORIENTED_EDGE ( 'NONE', *, *, #7954, .T. ) ;
#21632 = CARTESIAN_POINT ( 'NONE',  ( 3.662846001190051659, 195.5725841191953691, 47.60113791807857808 ) ) ;
#21633 = EDGE_CURVE ( 'NONE', #5010, #33593, #23189, .T. ) ;
#21634 = CARTESIAN_POINT ( 'NONE',  ( 9.379977934355958169, 208.8253170565643302, -1.014254689207424676 ) ) ;
#21635 = CARTESIAN_POINT ( 'NONE',  ( -8.062137200540822946, 201.0835637161416400, 20.19886208192143684 ) ) ;
#21636 = CARTESIAN_POINT ( 'NONE',  ( 71.18867513459481700, 169.2658477444273331, -4.635254915624224203 ) ) ;
#21637 = ORIENTED_EDGE ( 'NONE', *, *, #19354, .T. ) ;
#21638 = CARTESIAN_POINT ( 'NONE',  ( -0.05014649552810635652, 196.4853777576173002, 77.75113791807856956 ) ) ;
#21639 = AXIS2_PLACEMENT_3D ( 'NONE', #20410, #30634, #18192 ) ;
#21640 = ORIENTED_EDGE ( 'NONE', *, *, #25017, .F. ) ;
#21641 = AXIS2_PLACEMENT_3D ( 'NONE', #25714, #2556, #4936 ) ;
#21642 = CARTESIAN_POINT ( 'NONE',  ( 50.51132485994281041, 163.8167787843871110, 12.13525491562421621 ) ) ;
#21643 = FACE_OUTER_BOUND ( 'NONE', #22272, .T. ) ;
#21644 = EDGE_LOOP ( 'NONE', ( #19585, #5177, #23785, #2, #6331 ) ) ;
#21645 = CARTESIAN_POINT ( 'NONE',  ( -6.444103211791042618, 211.7408657792732356, 18.80113791807856671 ) ) ;
#21646 = CARTESIAN_POINT ( 'NONE',  ( 0.000000000000000000, 0.000000000000000000, 0.000000000000000000 ) ) ;
#21647 = CARTESIAN_POINT ( 'NONE',  ( 10.00000000000000711, 207.0476921513415220, 3.998862081921434442 ) ) ;
#21648 = CARTESIAN_POINT ( 'NONE',  ( 52.07499999726881157, 168.2552932293087906, 9.630534252274372875 ) ) ;
#21649 = VERTEX_POINT ( 'NONE', #27490 ) ;
#21650 = CARTESIAN_POINT ( 'NONE',  ( 55.42499999726879878, 168.2552932293087906, -9.630534252274385310 ) ) ;
#21651 = DIRECTION ( 'NONE',  ( 1.000000000000000000, 0.000000000000000000, 0.000000000000000000 ) ) ;
#21652 = DIRECTION ( 'NONE',  ( 0.000000000000000000, 0.000000000000000000, -1.000000000000000000 ) ) ;
#21653 = DIRECTION ( 'NONE',  ( -1.000000000000000000, 1.224646799147354686E-16, 0.000000000000000000 ) ) ;
#21654 = CARTESIAN_POINT ( 'NONE',  ( 6.139770520408223575, 215.5359834540460611, 87.54886208192142760 ) ) ;
#21655 = CARTESIAN_POINT ( 'NONE',  ( 59.57499999726881157, 164.1591823560292198, -12.60653300113719766 ) ) ;
#21656 = CARTESIAN_POINT ( 'NONE',  ( -0.05014649552810635652, 196.4853777576173002, 26.75113791807856956 ) ) ;
#21657 = CARTESIAN_POINT ( 'NONE',  ( 73.28867513459483973, 170.7719333635740497, -7.904646289410545231E-15 ) ) ;
#21658 = EDGE_CURVE ( 'NONE', #15028, #27213, #23260, .T. ) ;
#21659 = EDGE_CURVE ( 'NONE', #11308, #22951, #1264, .T. ) ;
#21660 = CARTESIAN_POINT ( 'NONE',  ( -11.98450388067341876, 203.0532714938636047, 80.34886208192143897 ) ) ;
#21661 = CARTESIAN_POINT ( 'NONE',  ( 76.39999999999996305, 150.2886644046228639, -14.50000000000000888 ) ) ;
#21662 = CARTESIAN_POINT ( 'NONE',  ( 65.08867513459482268, 167.7597621252805880, -9.270509831248443078 ) ) ;
#21663 = DIRECTION ( 'NONE',  ( 1.000000000000000000, -0.000000000000000000, -0.000000000000000000 ) ) ;
#21664 = CARTESIAN_POINT ( 'NONE',  ( 3.044812012440130555, 197.4746971517856764, 95.60113791807857808 ) ) ;
#21665 = CIRCLE ( 'NONE', #11869, 100.0000000000000284 ) ;
#21666 = CARTESIAN_POINT ( 'NONE',  ( 27.50000000000000355, -10.64700562007355344, -16.86587997430611807 ) ) ;
#21667 = CARTESIAN_POINT ( 'NONE',  ( 37.87499999726880873, 171.3844434931184253, -7.942151717890132712E-15 ) ) ;
#21668 = PRODUCT_RELATED_PRODUCT_CATEGORY ( 'part', '', ( #22203 ) ) ;
#21669 = EDGE_CURVE ( 'NONE', #6902, #31655, #950, .T. ) ;
#21670 = CARTESIAN_POINT ( 'NONE',  ( 6.139770520408368348, 198.4640165459539674, 35.45113791807857240 ) ) ;
#21671 = AXIS2_PLACEMENT_3D ( 'NONE', #13932, #19048, #6086 ) ;
#21672 = CARTESIAN_POINT ( 'NONE',  ( 77.32499999726881867, 164.1591823560292198, -12.60653300113719766 ) ) ;
#21673 = VERTEX_POINT ( 'NONE', #12160 ) ;
#21674 = CARTESIAN_POINT ( 'NONE',  ( 0.000000000000000000, 0.000000000000000000, -18.00000000000000000 ) ) ;
#21675 = CARTESIAN_POINT ( 'NONE',  ( 41.49999999453762456, 139.7537977485451393, -4.138211985947621020E-15 ) ) ;
#21676 = CARTESIAN_POINT ( 'NONE',  ( 11.98450388067348271, 203.0532714938637753, 20.15113791807856458 ) ) ;
#21677 = EDGE_CURVE ( 'NONE', #6436, #17153, #31951, .T. ) ;
#21678 = CARTESIAN_POINT ( 'NONE',  ( 39.91132485994280898, 163.8167787843871110, -12.13525491562423397 ) ) ;
#21679 = AXIS2_PLACEMENT_3D ( 'NONE', #5249, #23647, #15304 ) ;
#21680 = FACE_OUTER_BOUND ( 'NONE', #13029, .T. ) ;
#21681 = ORIENTED_EDGE ( 'NONE', *, *, #31027, .T. ) ;
#21682 = CARTESIAN_POINT ( 'NONE',  ( 11.98450388067341876, 210.9467285061363953, 33.84886208192142476 ) ) ;
#21683 = DIRECTION ( 'NONE',  ( -0.9945218953682772867, 0.000000000000000000, 0.1045284632676156678 ) ) ;
#21684 = CARTESIAN_POINT ( 'NONE',  ( -3.135527875058821579, 197.5041725223112223, 50.90113791807856813 ) ) ;
#21685 = ORIENTED_EDGE ( 'NONE', *, *, #13698, .F. ) ;
#21686 = CARTESIAN_POINT ( 'NONE',  ( 7.984503880673422316, 209.6470497212048372, 12.84886208192143719 ) ) ;
#21687 = PRODUCT_DEFINITION_CONTEXT ( 'detailed design', #13556, 'design' ) ;
#21688 = VERTEX_POINT ( 'NONE', #25099 ) ;
#21689 = CARTESIAN_POINT ( 'NONE',  ( -4.903702542908436435, 200.1653181626580249, 104.0488620819214560 ) ) ;
#21690 = CIRCLE ( 'NONE', #17337, 8.000000000000000000 ) ;
#21691 = CARTESIAN_POINT ( 'NONE',  ( -4.984841277089726574, 200.2242689037092305, 39.05113791807855961 ) ) ;
#21692 = DIRECTION ( 'NONE',  ( 0.000000000000000000, 0.000000000000000000, 1.000000000000000000 ) ) ;
#21693 = ORIENTED_EDGE ( 'NONE', *, *, #21584, .F. ) ;
#21694 = CARTESIAN_POINT ( 'NONE',  ( 39.42499999726881299, 168.2552932293087906, -9.630534252274385310 ) ) ;
#21695 = AXIS2_PLACEMENT_3D ( 'NONE', #21490, #29330, #13820 ) ;
#21696 = CARTESIAN_POINT ( 'NONE',  ( 3.135527875058981895, 197.5041725223112792, 61.59886208192143897 ) ) ;
#21697 = CARTESIAN_POINT ( 'NONE',  ( 34.57499999726881157, 145.8408176439707802, 12.60653300113718345 ) ) ;
#21698 = CARTESIAN_POINT ( 'NONE',  ( 1.525316667890869448E-15, 4.041451884327390331, -2.899999999999999911 ) ) ;
#21699 = CARTESIAN_POINT ( 'NONE',  ( -7.949154985843430055, 215.5765611960900117, 102.9933096652613642 ) ) ;
#21700 = CIRCLE ( 'NONE', #21168, 2.149999999999985256 ) ;
#21701 = CARTESIAN_POINT ( 'NONE',  ( 56.09999999999999432, 141.2096805137202580, -4.480746418436742040 ) ) ;
#21702 = CARTESIAN_POINT ( 'NONE',  ( -6.500168698208244500, 211.6636982574061676, 74.79886208192142760 ) ) ;
#21703 = CARTESIAN_POINT ( 'NONE',  ( 127.5000000000000000, 261.0000000000000000, 0.000000000000000000 ) ) ;
#21704 = CARTESIAN_POINT ( 'NONE',  ( 56.62499999726880162, 138.6155565068815463, -3.929120461958505118E-15 ) ) ;
#21706 = ORIENTED_EDGE ( 'NONE', *, *, #1569, .T. ) ;
#21705 = CARTESIAN_POINT ( 'NONE',  ( 8.062137200540920645, 201.0835637161417822, 8.301137918078566713 ) ) ;
#21707 = CARTESIAN_POINT ( 'NONE',  ( 37.21132485994281325, 139.2280666364260071, -4.041636747397287284E-15 ) ) ;
#21708 = CARTESIAN_POINT ( 'NONE',  ( 65.32499999726881867, 164.1591823560292198, -12.60653300113719766 ) ) ;
#21709 = CARTESIAN_POINT ( 'NONE',  ( 73.77499999726882152, 169.8198683612136222, -4.815267126137197984 ) ) ;
#21710 = CARTESIAN_POINT ( 'NONE',  ( 0.05014649552807549926, 219.6175466908591716, 79.25113791807856956 ) ) ;
#21711 = CIRCLE ( 'NONE', #5378, 32.10452846326769816 ) ;
#21712 = CARTESIAN_POINT ( 'NONE',  ( -3.135527875058821579, 197.5041725223112223, 101.9011379180785752 ) ) ;
#21713 = DIRECTION ( 'NONE',  ( -1.804112415015879625E-16, 1.000000000000000000, 0.000000000000000000 ) ) ;
#21714 = ORIENTED_EDGE ( 'NONE', *, *, #16249, .F. ) ;
#21715 = CARTESIAN_POINT ( 'NONE',  ( -3.662846001189865142, 195.5725841191952838, 103.8988620819214361 ) ) ;
#21716 = CARTESIAN_POINT ( 'NONE',  ( -11.98450388067341876, 203.0532714938636047, 65.34886208192142476 ) ) ;
#21717 = CARTESIAN_POINT ( 'NONE',  ( -6.139770520408224463, 198.4640165459539105, 71.04886208192141339 ) ) ;
#21718 = CARTESIAN_POINT ( 'NONE',  ( 3.753561863808876797, 195.6020594897209719, 7.598862081921434530 ) ) ;
#21719 = LINE ( 'NONE', #11334, #30623 ) ;
#21720 = CARTESIAN_POINT ( 'NONE',  ( -8.118202686958039038, 201.1607312380087080, 27.20113791807856884 ) ) ;
#21721 = CARTESIAN_POINT ( 'NONE',  ( 10.00000000000000711, 207.0476921513415220, 84.99886208192143044 ) ) ;
#21722 = ORIENTED_EDGE ( 'NONE', *, *, #17436, .F. ) ;
#21723 = LINE ( 'NONE', #6218, #21363 ) ;
#21724 = VERTEX_POINT ( 'NONE', #29888 ) ;
#21725 = CARTESIAN_POINT ( 'NONE',  ( -52.50000000000002132, 155.0000000000000000, -6.938893903907228378E-15 ) ) ;
#21726 = CARTESIAN_POINT ( 'NONE',  ( 4.903702542908435547, 213.8346818373419751, 72.54886208192141339 ) ) ;
#21727 = VERTEX_POINT ( 'NONE', #26976 ) ;
#21728 = CARTESIAN_POINT ( 'NONE',  ( 81.42499999726882720, 168.2552932293087906, -9.630534252274387086 ) ) ;
#21729 = ORIENTED_EDGE ( 'NONE', *, *, #15758, .F. ) ;
#21730 = CARTESIAN_POINT ( 'NONE',  ( 68.98867513459482836, 163.8167787843871110, -12.13525491562423397 ) ) ;
#21731 = AXIS2_PLACEMENT_3D ( 'NONE', #31891, #392, #3112 ) ;
#21732 = CARTESIAN_POINT ( 'NONE',  ( 71.62499999726881583, 171.3844434931184253, -7.942151717890132712E-15 ) ) ;
#21733 =( BOUNDED_CURVE ( )  B_SPLINE_CURVE ( 2, ( #14187, #11303, #3960, #11142, #14017, #32576, #16571, #31904, #1241, #18967, #32079 ),
 .UNSPECIFIED., .F., .T. ) 
 B_SPLINE_CURVE_WITH_KNOTS ( ( 3, 2, 2, 2, 2, 3 ),
 ( 0.3035714285714285476, 0.3071428571428571619, 0.3107142857142857761, 0.3142857142857143349, 0.3178571428571429491, 0.3214285714285715634 ),
 .UNSPECIFIED. ) 
 CURVE ( )  GEOMETRIC_REPRESENTATION_ITEM ( )  RATIONAL_B_SPLINE_CURVE ( ( 1.000000000000000000, 0.9510565162951534202, 1.000000000000000000, 0.9510565162951534202, 1.000000000000000000, 0.9510565162951534202, 1.000000000000000000, 0.9510565162951534202, 1.000000000000000000, 0.9510565162951518658, 1.000000000000001554 ) ) 
 REPRESENTATION_ITEM ( '' )  );
#21734 = CARTESIAN_POINT ( 'NONE',  ( -8.000000000000008882, 207.0476921513413515, 66.50113791807856956 ) ) ;
#21735 = DIRECTION ( 'NONE',  ( 1.000000000000000000, 0.000000000000000000, 0.000000000000000000 ) ) ;
#21736 = CARTESIAN_POINT ( 'NONE',  ( 57.91132485994280898, 163.8167787843871110, -12.13525491562423397 ) ) ;
#21737 = CARTESIAN_POINT ( 'NONE',  ( 37.70000000000000284, 146.4771138417591203, 11.73074641843673227 ) ) ;
#21738 = CARTESIAN_POINT ( 'NONE',  ( -2.426778023690076225, 199.3768101843759553, 46.89886208192144323 ) ) ;
#21739 = CARTESIAN_POINT ( 'NONE',  ( 0.05014649552810505201, 217.5146222423826714, 85.25113791807854113 ) ) ;
#21740 = CARTESIAN_POINT ( 'NONE',  ( -0.05014649552810635652, 196.4853777576173002, 65.75113791807856956 ) ) ;
#21741 = DIRECTION ( 'NONE',  ( -1.000000000000000000, 0.000000000000000000, 0.000000000000000000 ) ) ;
#21742 = CARTESIAN_POINT ( 'NONE',  ( 0.05014649552807626948, 215.4116977939061144, 25.25113791807856956 ) ) ;
#21743 = CARTESIAN_POINT ( 'NONE',  ( -61.00000000000002842, 209.9999999999999716, -3.061616997868380183E-16 ) ) ;
#21744 = CARTESIAN_POINT ( 'NONE',  ( 81.78867513459482552, 155.0000000000000000, 15.00000000000001243 ) ) ;
#21745 = CARTESIAN_POINT ( 'NONE',  ( 47.02499999726881441, 149.9369285172503510, -15.58253175000000823 ) ) ;
#21746 = CARTESIAN_POINT ( 'NONE',  ( -12.01549611932652972, 203.1486557965464499, 51.35113791807857098 ) ) ;
#21747 = CARTESIAN_POINT ( 'NONE',  ( 7.499999999999999112, 4.652409454067514716, -7.929128589908465585 ) ) ;
#21748 = CARTESIAN_POINT ( 'NONE',  ( 6.220909254589536808, 215.4770327129947702, 97.55113791807855250 ) ) ;
#21749 = EDGE_CURVE ( 'NONE', #31748, #13306, #19487, .T. ) ;
#21750 = CARTESIAN_POINT ( 'NONE',  ( -10.00000000000000711, 207.0476921513413515, 72.50113791807858377 ) ) ;
#21751 = CARTESIAN_POINT ( 'NONE',  ( -12.01549611932659722, 210.8513442034533227, 35.64886208192142902 ) ) ;
#21752 = CARTESIAN_POINT ( 'NONE',  ( 10.01549611932659367, 203.7984951890124421, 40.14886208192143613 ) ) ;
#21753 = CARTESIAN_POINT ( 'NONE',  ( 83.89999999453763735, 150.2886644046228639, -14.50000000000000888 ) ) ;
#21754 = CARTESIAN_POINT ( 'NONE',  ( -3.753561863808691168, 195.6020594897209435, 77.90113791807856103 ) ) ;
#21755 = CARTESIAN_POINT ( 'NONE',  ( 6.500168698208129925, 211.6636982574063381, 94.70113791807858661 ) ) ;
#21756 = CARTESIAN_POINT ( 'NONE',  ( -6.220909254589682469, 215.4770327129946850, 59.94886208192141908 ) ) ;
#21757 =( NAMED_UNIT ( * ) PLANE_ANGLE_UNIT ( ) SI_UNIT ( $, .RADIAN. ) );
#21758 = ORIENTED_EDGE ( 'NONE', *, *, #16863, .F. ) ;
#21759 = CARTESIAN_POINT ( 'NONE',  ( 11.98450388067341876, 210.9467285061363953, 60.84886208192143187 ) ) ;
#21760 = ORIENTED_EDGE ( 'NONE', *, *, #18516, .T. ) ;
#21761 = CARTESIAN_POINT ( 'NONE',  ( 70.07499999726881867, 168.2552932293087906, 9.630534252274372875 ) ) ;
#21762 = CARTESIAN_POINT ( 'NONE',  ( -6.444103211790928043, 202.2591342207265939, 38.19886208192144750 ) ) ;
#21763 = ORIENTED_EDGE ( 'NONE', *, *, #6994, .F. ) ;
#21764 = CARTESIAN_POINT ( 'NONE',  ( 73.97499999726881015, 169.8198683612136222, 4.815267126137181997 ) ) ;
#21765 = CARTESIAN_POINT ( 'NONE',  ( 107.0104235265664556, 155.0000000000000000, 0.000000000000000000 ) ) ;
#21766 = CARTESIAN_POINT ( 'NONE',  ( 125.0000000000000000, 3.061616997868383121E-14, 20.00000000000000000 ) ) ;
#21767 = AXIS2_PLACEMENT_3D ( 'NONE', #8181, #25727, #18061 ) ;
#21768 = CARTESIAN_POINT ( 'NONE',  ( -6.444103211791042618, 211.7408657792732356, 51.80113791807858092 ) ) ;
#21769 = CARTESIAN_POINT ( 'NONE',  ( 2.927447417349540615, -2.351289329882181534, -2.778243469714872571 ) ) ;
#21770 = CARTESIAN_POINT ( 'NONE',  ( 6.220909254589681581, 198.5229672870052582, 37.44886208192143329 ) ) ;
#21771 = CARTESIAN_POINT ( 'NONE',  ( 70.87499999726880162, 138.6155565068815747, -3.929120461958505118E-15 ) ) ;
#21772 = ORIENTED_EDGE ( 'NONE', *, *, #28569, .T. ) ;
#21773 = CARTESIAN_POINT ( 'NONE',  ( 7.500000000000000000, 4.330127018922190096, -10.00000000000000000 ) ) ;
#21774 = DIRECTION ( 'NONE',  ( 1.000000000000000000, 0.000000000000000000, 0.000000000000000000 ) ) ;
#21775 = ADVANCED_BREP_SHAPE_REPRESENTATION ( '', ( #12954, #2404 ), #1885 ) ;
#21776 = FACE_OUTER_BOUND ( 'NONE', #26306, .T. ) ;
#21777 = CARTESIAN_POINT ( 'NONE',  ( 7.984503880673422316, 209.6470497212048372, 15.84886208192143719 ) ) ;
#21778 = CARTESIAN_POINT ( 'NONE',  ( -9.984503880673473830, 210.2968891136704315, 51.65113791807855392 ) ) ;
#21779 = CARTESIAN_POINT ( 'NONE',  ( -0.05014649552810635652, 196.4853777576173002, 41.75113791807855534 ) ) ;
#21780 = CARTESIAN_POINT ( 'NONE',  ( 85.47499999726879594, 160.0630714827496206, -15.58253175000000823 ) ) ;
#21781 = CONTEXT_DEPENDENT_SHAPE_REPRESENTATION ( #32064, #25777 ) ;
#21782 = CARTESIAN_POINT ( 'NONE',  ( -2.517493886309087880, 214.5937144450984135, 99.09886208192145318 ) ) ;
#21783 = CARTESIAN_POINT ( 'NONE',  ( 41.12499999726880873, 155.0000000000000000, -15.58253175000000823 ) ) ;
#21784 = DIRECTION ( 'NONE',  ( 1.000000000000000000, 0.000000000000000000, 0.000000000000000000 ) ) ;
#21785 = FACE_OUTER_BOUND ( 'NONE', #8414, .T. ) ;
#21786 = CARTESIAN_POINT ( 'NONE',  ( -3.753561863808691168, 195.6020594897209435, 14.90113791807856636 ) ) ;
#21787 = CARTESIAN_POINT ( 'NONE',  ( -3.500000000000001332, 2.020725942163676070, -2.899999999999999911 ) ) ;
#21788 = CARTESIAN_POINT ( 'NONE',  ( -0.05014649552810635652, 196.4853777576173002, 68.75113791807855534 ) ) ;
#21789 = EDGE_CURVE ( 'NONE', #27139, #31166, #6319, .T. ) ;
#21790 = CARTESIAN_POINT ( 'NONE',  ( 10.00000000000000711, 206.9523078486586201, 38.00113791807857666 ) ) ;
#21791 = CARTESIAN_POINT ( 'NONE',  ( -52.50000000000002132, 155.0000000000000000, -16.99999999999999645 ) ) ;
#21792 = DIRECTION ( 'NONE',  ( 1.000000000000000000, 0.000000000000000000, 0.000000000000000000 ) ) ;
#21793 = CARTESIAN_POINT ( 'NONE',  ( 9.680171189290716072, 214.0920067884432854, 6.698862081921434175 ) ) ;
#21794 = CARTESIAN_POINT ( 'NONE',  ( -3.135527875058982783, 216.4958274776886924, 6.098862081921434530 ) ) ;
#21795 = CARTESIAN_POINT ( 'NONE',  ( 67.39999999453763735, 141.2096805137202580, 4.480746418436733158 ) ) ;
#21796 = ORIENTED_EDGE ( 'NONE', *, *, #9759, .F. ) ;
#21797 = CARTESIAN_POINT ( 'NONE',  ( 11.98450388067348271, 203.0532714938637753, 47.15113791807857524 ) ) ;
#21798 = CARTESIAN_POINT ( 'NONE',  ( 7.984503880673485376, 204.3529502787953902, 68.15113791807856103 ) ) ;
#21799 = CARTESIAN_POINT ( 'NONE',  ( 83.21132485994282035, 139.2280666364260071, -4.041636747397287284E-15 ) ) ;
#21800 = CARTESIAN_POINT ( 'NONE',  ( -3.135527875058982783, 216.4958274776886924, 33.09886208192143187 ) ) ;
#21801 = ORIENTED_EDGE ( 'NONE', *, *, #20574, .T. ) ;
#21802 = EDGE_CURVE ( 'NONE', #982, #22231, #14381, .T. ) ;
#21803 = CARTESIAN_POINT ( 'NONE',  ( 6.220909254589536808, 215.4770327129947702, 82.55113791807858092 ) ) ;
#21804 = VERTEX_POINT ( 'NONE', #22209 ) ;
#21805 = CARTESIAN_POINT ( 'NONE',  ( 50.71132485994280614, 155.0000000000000000, 15.00000000000001243 ) ) ;
#21806 = CARTESIAN_POINT ( 'NONE',  ( 1.750000000000014211, 3.031088913245526317, -2.899999999999999911 ) ) ;
#21807 = ORIENTED_EDGE ( 'NONE', *, *, #29729, .F. ) ;
#21808 = CARTESIAN_POINT ( 'NONE',  ( 6.444103211791042618, 202.2591342207267644, 23.30113791807857027 ) ) ;
#21809 = EDGE_CURVE ( 'NONE', #7596, #18104, #32598, .T. ) ;
#21810 = FACE_OUTER_BOUND ( 'NONE', #5555, .T. ) ;
#21811 = CARTESIAN_POINT ( 'NONE',  ( -3.044812012439970683, 197.4746971517856196, 1.898862081921434353 ) ) ;
#21812 = CARTESIAN_POINT ( 'NONE',  ( 51.17499999726880588, 145.8408176439707802, -12.60653300113719588 ) ) ;
#21813 = EDGE_LOOP ( 'NONE', ( #18511, #24069, #1823 ) ) ;
#21814 = CARTESIAN_POINT ( 'NONE',  ( 55.62499999726881583, 171.3844434931184253, -7.942151717890132712E-15 ) ) ;
#21815 = DIRECTION ( 'NONE',  ( 0.000000000000000000, 0.000000000000000000, -1.000000000000000000 ) ) ;
#21816 = CARTESIAN_POINT ( 'NONE',  ( 87.50000000000000000, 160.9457742543943652, -14.40357817542362540 ) ) ;
#21817 = AXIS2_PLACEMENT_3D ( 'NONE', #22801, #20238, #26514 ) ;
#21818 = LINE ( 'NONE', #19433, #13525 ) ;
#21819 = CARTESIAN_POINT ( 'NONE',  ( 0.05014649552828275708, 196.4853777576173002, 91.74886208192144466 ) ) ;
#21820 = EDGE_CURVE ( 'NONE', #9151, #3168, #12307, .T. ) ;
#21821 = CARTESIAN_POINT ( 'NONE',  ( 58.67499999726882010, 141.7447067706911810, 9.630534252274376428 ) ) ;
#21822 = CARTESIAN_POINT ( 'NONE',  ( -9.984503880673473830, 210.2968891136704315, 21.65113791807856458 ) ) ;
#21823 = CARTESIAN_POINT ( 'NONE',  ( 73.18867513459481700, 169.2658477444273331, -4.635254915624224203 ) ) ;
#21824 = CARTESIAN_POINT ( 'NONE',  ( 3.753561863808876797, 195.6020594897209719, 76.59886208192142476 ) ) ;
#21825 = CARTESIAN_POINT ( 'NONE',  ( 71.70000000000000284, 146.4771138417591203, 11.73074641843673227 ) ) ;
#21826 = CARTESIAN_POINT ( 'NONE',  ( 61.81132485994281467, 159.8737954434936057, -15.00000000000002665 ) ) ;
#21827 = DIRECTION ( 'NONE',  ( 0.000000000000000000, 0.000000000000000000, -1.000000000000000000 ) ) ;
#21828 = CARTESIAN_POINT ( 'NONE',  ( 6.220909254589536808, 215.4770327129947702, 94.55113791807858092 ) ) ;
#21829 = CARTESIAN_POINT ( 'NONE',  ( 33.68867513459484542, 159.8737954434934920, 15.00000000000010836 ) ) ;
#21830 = CARTESIAN_POINT ( 'NONE',  ( 47.27499999726880731, 149.9369285172503510, -15.58253175000000823 ) ) ;
#21831 = CARTESIAN_POINT ( 'NONE',  ( 8.062137200540920645, 201.0835637161417822, 41.30113791807857382 ) ) ;
#21832 = CARTESIAN_POINT ( 'NONE',  ( 73.82499999726879025, 168.2552932293087906, 9.630534252274372875 ) ) ;
#21833 = ORIENTED_EDGE ( 'NONE', *, *, #6430, .T. ) ;
#21834 = CYLINDRICAL_SURFACE ( 'NONE', #9218, 5.250000000000004441 ) ;
#21835 = CARTESIAN_POINT ( 'NONE',  ( 50.29999999453763593, 167.3344367211045096, -8.961492836873482304 ) ) ;
#21836 = CARTESIAN_POINT ( 'NONE',  ( -9.680171189290831535, 214.0920067884431148, 18.80113791807856671 ) ) ;
#21837 = CARTESIAN_POINT ( 'NONE',  ( 2.343682934607771440, 2.688325911136448809, -2.870065989602863965 ) ) ;
#21838 = CARTESIAN_POINT ( 'NONE',  ( -5.007715329123872641E-16, -8.660254037844399733, -7.422398894150038728 ) ) ;
#21839 = EDGE_LOOP ( 'NONE', ( #1191, #32357, #26584, #8090 ) ) ;
#21840 = CIRCLE ( 'NONE', #10442, 2.500000000000000000 ) ;
#21841 = CARTESIAN_POINT ( 'NONE',  ( 3.662846001189864698, 218.4274158808046593, 30.39886208192143613 ) ) ;
#21842 = CARTESIAN_POINT ( 'NONE',  ( 6.499999999999999112, -3.752776749732576356, -0.8000000000000003775 ) ) ;
#21843 = CARTESIAN_POINT ( 'NONE',  ( -3.044812012440131443, 216.5253028482142952, 55.10113791807857098 ) ) ;
#21844 = EDGE_LOOP ( 'NONE', ( #23902, #31905, #12082, #16739 ) ) ;
#21845 = CARTESIAN_POINT ( 'NONE',  ( -2.426778023690076225, 199.3768101843759553, 16.89886208192143613 ) ) ;
#21846 = EDGE_CURVE ( 'NONE', #30153, #7020, #8486, .T. ) ;
#21847 = ADVANCED_FACE ( 'NONE', ( #9777 ), #11295, .T. ) ;
#21848 = CARTESIAN_POINT ( 'NONE',  ( -22.99387487948482089, -18.47874495404630935, -16.90910675883082703 ) ) ;
#21849 = ORIENTED_EDGE ( 'NONE', *, *, #18151, .F. ) ;
#21850 = CARTESIAN_POINT ( 'NONE',  ( 0.05014649552828262524, 198.5883022060938572, 100.7488620819214304 ) ) ;
#21851 = EDGE_CURVE ( 'NONE', #23832, #8655, #16303, .T. ) ;
#21852 = CARTESIAN_POINT ( 'NONE',  ( 0.000000000000000000, 0.000000000000000000, -2.899999999999999911 ) ) ;
#21853 = CARTESIAN_POINT ( 'NONE',  ( 8.015496119326531499, 209.5516654185219636, 37.85113791807857098 ) ) ;
#21854 = FACE_OUTER_BOUND ( 'NONE', #15733, .T. ) ;
#21855 = ORIENTED_EDGE ( 'NONE', *, *, #7063, .F. ) ;
#21856 = CARTESIAN_POINT ( 'NONE',  ( 40.72499999726881725, 140.1801316387863778, -4.815267126137194431 ) ) ;
#21857 = CARTESIAN_POINT ( 'NONE',  ( 3.044812012439969795, 216.5253028482143520, 63.39886208192144323 ) ) ;
#21858 = EDGE_CURVE ( 'NONE', #26980, #8952, #25910, .T. ) ;
#21859 = CARTESIAN_POINT ( 'NONE',  ( 40.77499999726881441, 140.1801316387863778, 4.815267126137185549 ) ) ;
#21860 = CARTESIAN_POINT ( 'NONE',  ( -67.50000000000000000, 155.0000000000000000, -37.00000000000000000 ) ) ;
#21861 = CARTESIAN_POINT ( 'NONE',  ( -6.444103211791042618, 211.7408657792732356, 96.80113791807858092 ) ) ;
#21862 = CARTESIAN_POINT ( 'NONE',  ( 52.59999999999999432, 159.7113355953771077, -14.50000000000000888 ) ) ;
#21863 = FACE_BOUND ( 'NONE', #28235, .T. ) ;
#21864 = CARTESIAN_POINT ( 'NONE',  ( -4.984841277089891776, 213.7757310962905990, 71.94886208192144750 ) ) ;
#21865 = DIRECTION ( 'NONE',  ( 1.000000000000000000, -0.000000000000000000, -0.000000000000000000 ) ) ;
#21866 = DIRECTION ( 'NONE',  ( -0.000000000000000000, -0.000000000000000000, -1.000000000000000000 ) ) ;
#21867 = CARTESIAN_POINT ( 'NONE',  ( 57.32499999726881157, 164.1591823560292198, -12.60653300113719766 ) ) ;
#21869 = VERTEX_POINT ( 'NONE', #4664 ) ;
#21868 = CARTESIAN_POINT ( 'NONE',  ( -3.044812012440131443, 216.5253028482142952, 10.10113791807856565 ) ) ;
#21870 = FACE_OUTER_BOUND ( 'NONE', #14656, .T. ) ;
#21871 = AXIS2_PLACEMENT_3D ( 'NONE', #16457, #5733, #13908 ) ;
#21872 = CARTESIAN_POINT ( 'NONE',  ( 68.12499999726881583, 155.0000000000000000, 15.58253174999999402 ) ) ;
#21873 = CARTESIAN_POINT ( 'NONE',  ( 78.07499999726880446, 168.2552932293087906, 9.630534252274372875 ) ) ;
#21874 = CARTESIAN_POINT ( 'NONE',  ( 12.01549611932652972, 210.8513442034534933, 79.85113791807857808 ) ) ;
#21875 = CARTESIAN_POINT ( 'NONE',  ( 10.01549611932653860, 210.2015048109876716, 94.85113791807857808 ) ) ;
#21876 = DIRECTION ( 'NONE',  ( 0.000000000000000000, 0.000000000000000000, -1.000000000000000000 ) ) ;
#21877 = ORIENTED_EDGE ( 'NONE', *, *, #2027, .T. ) ;
#21878 = CARTESIAN_POINT ( 'NONE',  ( -9.736236675708031640, 214.0148392665760753, 101.7988620819214560 ) ) ;
#21879 = CARTESIAN_POINT ( 'NONE',  ( -3.753561863808878130, 218.3979405102790281, 57.09886208192143897 ) ) ;
#21880 = CARTESIAN_POINT ( 'NONE',  ( 8.118202686958138514, 201.1607312380088501, 79.29886208192144181 ) ) ;
#21881 = CARTESIAN_POINT ( 'NONE',  ( -3.662846001189865142, 195.5725841191952838, 4.898862081921434353 ) ) ;
#21882 = CARTESIAN_POINT ( 'NONE',  ( -52.50000000000002132, 155.0000000000000000, -40.00000000000000000 ) ) ;
#21883 = CARTESIAN_POINT ( 'NONE',  ( 3.135527875058820690, 216.4958274776887492, 22.40113791807856458 ) ) ;
#21884 = CARTESIAN_POINT ( 'NONE',  ( -6.139770520408224463, 198.4640165459539389, 92.04886208192139918 ) ) ;
#21885 = ADVANCED_FACE ( 'NONE', ( #25788 ), #31075, .F. ) ;
#21886 = ORIENTED_EDGE ( 'NONE', *, *, #28982, .T. ) ;
#21887 = PRODUCT_DEFINITION_FORMATION_WITH_SPECIFIED_SOURCE ( 'ANY', '', #29822, .NOT_KNOWN. ) ;
#21888 = CARTESIAN_POINT ( 'NONE',  ( 39.31132485994280756, 140.7341522555726669, -4.635254915624220651 ) ) ;
#21889 = ORIENTED_EDGE ( 'NONE', *, *, #1797, .F. ) ;
#21890 = DIRECTION ( 'NONE',  ( -1.804112415015879625E-16, 1.000000000000000000, 0.000000000000000000 ) ) ;
#21891 = CARTESIAN_POINT ( 'NONE',  ( 0.05014649552828262524, 198.5883022060938572, 67.74886208192143044 ) ) ;
#21892 = ORIENTED_EDGE ( 'NONE', *, *, #27707, .T. ) ;
#21893 = CARTESIAN_POINT ( 'NONE',  ( 87.02499999726880731, 149.9369285172503510, -15.58253175000000823 ) ) ;
#21894 = ORIENTED_EDGE ( 'NONE', *, *, #14599, .T. ) ;
#21895 = DIRECTION ( 'NONE',  ( 0.000000000000000000, 0.000000000000000000, -1.000000000000000000 ) ) ;
#21896 = VECTOR ( 'NONE', #12335, 1000.000000000000000 ) ;
#21897 = AXIS2_PLACEMENT_3D ( 'NONE', #26493, #605, #13551 ) ;
#21898 = CARTESIAN_POINT ( 'NONE',  ( 79.02499999726879309, 149.9369285172503510, -15.58253175000000823 ) ) ;
#21899 = CARTESIAN_POINT ( 'NONE',  ( -4.903702542908602524, 213.8346818373418898, 69.95113791807858661 ) ) ;
#21900 = DIRECTION ( 'NONE',  ( 0.000000000000000000, 0.000000000000000000, -1.000000000000000000 ) ) ;
#21901 =( NAMED_UNIT ( * ) PLANE_ANGLE_UNIT ( ) SI_UNIT ( $, .RADIAN. ) );
#21902 = CARTESIAN_POINT ( 'NONE',  ( 36.10000000000000142, 141.2096805137202580, -4.480746418436742040 ) ) ;
#21903 = CARTESIAN_POINT ( 'NONE',  ( 6.500168698208244500, 202.3363017425938324, 43.29886208192144181 ) ) ;
#21904 = CARTESIAN_POINT ( 'NONE',  ( 3.044812012440130555, 197.4746971517856764, 86.60113791807857808 ) ) ;
#21905 = CARTESIAN_POINT ( 'NONE',  ( 3.135527875058820690, 216.4958274776887492, 70.40113791807857524 ) ) ;
#21906 = AXIS2_PLACEMENT_3D ( 'NONE', #15352, #25742, #20640 ) ;
#21907 = CARTESIAN_POINT ( 'NONE',  ( 0.000000000000000000, 2.342598717236910488, 4.057499999999995666 ) ) ;
#21908 = DIRECTION ( 'NONE',  ( 1.000000000000000000, 0.000000000000000000, 0.000000000000000000 ) ) ;
#21909 = CARTESIAN_POINT ( 'NONE',  ( -3.499999999999999556, -3.004629197474309385E-15, -2.899999999999999911 ) ) ;
#21910 = CARTESIAN_POINT ( 'NONE',  ( 52.62499999726880873, 138.6155565068815747, -3.929120461958505118E-15 ) ) ;
#21911 = CARTESIAN_POINT ( 'NONE',  ( -7.456977232089304408, 196.8216656703010301, 45.05113791807857382 ) ) ;
#21912 = CARTESIAN_POINT ( 'NONE',  ( -2.000000000000000000, 0.000000000000000000, -2.874600000000001376 ) ) ;
#21913 = PRODUCT_DEFINITION_SHAPE ( 'NONE', 'NONE',  #13732 ) ;
#21914 = CARTESIAN_POINT ( 'NONE',  ( -3.135527875058821579, 197.5041725223112223, 95.90113791807858945 ) ) ;
#21915 = CARTESIAN_POINT ( 'NONE',  ( -3.135527875058821579, 197.5041725223112223, 68.90113791807857524 ) ) ;
#21916 = CARTESIAN_POINT ( 'NONE',  ( -9.680171189290716072, 199.9079932115567146, 29.19886208192143684 ) ) ;
#21917 = CARTESIAN_POINT ( 'NONE',  ( 3.044812012439969795, 216.5253028482143520, 39.39886208192143613 ) ) ;
#21918 = CARTESIAN_POINT ( 'NONE',  ( 83.69999999453763451, 142.6655632788954620, -8.961492836873480528 ) ) ;
#21919 = CIRCLE ( 'NONE', #6708, 13.00000000000001066 ) ;
#21920 = CARTESIAN_POINT ( 'NONE',  ( -11.98450388067348804, 210.9467285061362247, 75.65113791807856103 ) ) ;
#21921 = CARTESIAN_POINT ( 'NONE',  ( -7.984503880673488041, 209.6470497212046098, 96.65113791807858945 ) ) ;
#21922 = AXIS2_PLACEMENT_3D ( 'NONE', #4119, #22528, #19804 ) ;
#21923 = CARTESIAN_POINT ( 'NONE',  ( -8.118202686958138514, 212.8392687619910930, 62.79886208192144181 ) ) ;
#21924 = AXIS2_PLACEMENT_3D ( 'NONE', #13390, #3802, #29693 ) ;
#21925 = CARTESIAN_POINT ( 'NONE',  ( 5.274401269815139237, 6.074457022762083547, -7.633824513837111247 ) ) ;
#21926 = ORIENTED_EDGE ( 'NONE', *, *, #29585, .F. ) ;
#21927 = CARTESIAN_POINT ( 'NONE',  ( -11.98450388067341876, 203.0532714938636047, 65.34886208192142476 ) ) ;
#21928 = VERTEX_POINT ( 'NONE', #7571 ) ;
#21929 = CARTESIAN_POINT ( 'NONE',  ( 73.87499999726881583, 171.3844434931184253, -7.942151717890132712E-15 ) ) ;
#21930 = CARTESIAN_POINT ( 'NONE',  ( 4.984841277089891776, 200.2242689037093726, 40.44886208192144750 ) ) ;
#21931 = ORIENTED_EDGE ( 'NONE', *, *, #11856, .F. ) ;
#21932 = CARTESIAN_POINT ( 'NONE',  ( 80.97499999726881015, 140.1801316387863778, -4.815267126137194431 ) ) ;
#21933 = DIRECTION ( 'NONE',  ( 1.000000000000000000, -0.000000000000000000, -0.000000000000000000 ) ) ;
#21934 = CONICAL_SURFACE ( 'NONE', #30665, 6.500000000000000888, 0.8987552595851582282 ) ;
#21935 = DIRECTION ( 'NONE',  ( 0.000000000000000000, -1.000000000000000000, 1.295896757998781572E-15 ) ) ;
#21936 = CARTESIAN_POINT ( 'NONE',  ( -7.984503880673488041, 209.6470497212046098, 54.65113791807857524 ) ) ;
#21937 = PRESENTATION_LAYER_ASSIGNMENT (  '', '', ( #7268 ) ) ;
#21938 = DIRECTION ( 'NONE',  ( 1.000000000000000000, 0.000000000000000000, 0.000000000000000000 ) ) ;
#21939 = EDGE_CURVE ( 'NONE', #8233, #2299, #5167, .T. ) ;
#21940 = CARTESIAN_POINT ( 'NONE',  ( -9.984503880673420539, 203.7031108863293980, 32.34886208192143187 ) ) ;
#21941 = CARTESIAN_POINT ( 'NONE',  ( 71.07499999726880446, 141.7447067706911810, -9.630534252274387086 ) ) ;
#21942 = EDGE_LOOP ( 'NONE', ( #19285, #26098, #23203 ) ) ;
#21943 = DIRECTION ( 'NONE',  ( -0.8660254037844382635, 0.5000000000000005551, 0.000000000000000000 ) ) ;
#21944 = CIRCLE ( 'NONE', #5107, 4.199999999999988631 ) ;
#21945 = CARTESIAN_POINT ( 'NONE',  ( 115.4999999999999858, 61.05130719884918733, -52.99999999999945999 ) ) ;
#21946 = CYLINDRICAL_SURFACE ( 'NONE', #11470, 15.00000000000001776 ) ;
#21947 = B_SPLINE_CURVE_WITH_KNOTS ( 'NONE', 3,
 ( #10477, #33635, #18132, #17789, #4845, #25625, #17969, #28531, #5180, #25962 ),
 .UNSPECIFIED., .F., .F.,
 ( 4, 2, 2, 2, 4 ),
 ( 0.01606529487141860127, 0.01806591702017404724, 0.02006653916892948974, 0.02406778346644038169, 0.03207027206146215170 ),
 .UNSPECIFIED. ) ;
#21948 = CARTESIAN_POINT ( 'NONE',  ( -0.05014649552828365914, 215.4116977939061144, 18.24886208192143755 ) ) ;
#21949 = CIRCLE ( 'NONE', #10548, 1.499999999999999556 ) ;
#21950 = CARTESIAN_POINT ( 'NONE',  ( -6.139770520408369237, 215.5359834540460042, 57.95113791807856529 ) ) ;
#21951 = CARTESIAN_POINT ( 'NONE',  ( 6.139770520408368348, 198.4640165459539674, 41.45113791807857240 ) ) ;
#21952 = VECTOR ( 'NONE', #17746, 1000.000000000000000 ) ;
#21953 = CONTEXT_DEPENDENT_SHAPE_REPRESENTATION ( #19866, #26396 ) ;
#21954 = CARTESIAN_POINT ( 'NONE',  ( 2.517493886309087436, 199.4062855549015865, 97.59886208192145318 ) ) ;
#21955 = CARTESIAN_POINT ( 'NONE',  ( 48.02499999726879309, 160.0630714827496206, 15.58253174999999402 ) ) ;
#21956 = B_SPLINE_CURVE_WITH_KNOTS ( 'NONE', 3,
 ( #30599, #7264, #17813, #2663, #4870, #20541, #30943, #31443, #100 ),
 .UNSPECIFIED., .F., .F.,
 ( 4, 2, 1, 2, 4 ),
 ( 0.000000000000000000, 0.002165063509461098365, 0.004330127018922195863, 0.006495190528383293360, 0.008660254037844389990 ),
 .UNSPECIFIED. ) ;
#21957 = DIRECTION ( 'NONE',  ( 0.000000000000000000, 0.7071067811865411334, -0.7071067811865540120 ) ) ;
#21958 = DIRECTION ( 'NONE',  ( 0.000000000000000000, 0.000000000000000000, -1.000000000000000000 ) ) ;
#21959 = CARTESIAN_POINT ( 'NONE',  ( -12.00000000000000711, 207.0476921513413515, 18.50113791807856956 ) ) ;
#21960 = CARTESIAN_POINT ( 'NONE',  ( 1.015826369459276846, -8.073766409988136772, -7.642786413614194529 ) ) ;
#21961 = CARTESIAN_POINT ( 'NONE',  ( 8.118202686958039038, 212.8392687619912635, 64.70113791807857240 ) ) ;
#21962 = CARTESIAN_POINT ( 'NONE',  ( -10.00000000000000711, 207.0476921513413515, 39.50113791807856956 ) ) ;
#21963 = DIRECTION ( 'NONE',  ( -1.000000000000000000, -0.000000000000000000, -0.000000000000000000 ) ) ;
#21964 = AXIS2_PLACEMENT_3D ( 'NONE', #18312, #21356, #10978 ) ;
#21965 = CARTESIAN_POINT ( 'NONE',  ( -10.00000000000000178, 206.7692714347156198, 108.3323677711372000 ) ) ;
#21966 = CARTESIAN_POINT ( 'NONE',  ( -3.662846001189865142, 195.5725841191952838, 7.898862081921435241 ) ) ;
#21967 = CARTESIAN_POINT ( 'NONE',  ( -6.220909254589682469, 215.4770327129947134, 5.948862081921435063 ) ) ;
#21968 = CARTESIAN_POINT ( 'NONE',  ( 67.09999999453762598, 150.2886644046228639, 14.49999999999999645 ) ) ;
#21969 = EDGE_LOOP ( 'NONE', ( #14304, #27374, #8652, #18924 ) ) ;
#21970 = CARTESIAN_POINT ( 'NONE',  ( 9.736236675707914401, 214.0148392665762458, 52.70113791807856529 ) ) ;
#21971 = CARTESIAN_POINT ( 'NONE',  ( -4.984841277089726574, 200.2242689037092305, 69.05113791807856671 ) ) ;
#21972 = CARTESIAN_POINT ( 'NONE',  ( 130.2500000000000000, 3.061616997868383121E-14, -35.00000000000000000 ) ) ;
#21973 = CARTESIAN_POINT ( 'NONE',  ( 3.044812012439969795, 216.5253028482143520, 27.39886208192143613 ) ) ;
#21974 = VERTEX_POINT ( 'NONE', #23226 ) ;
#21975 = SHAPE_REPRESENTATION ( 'spring', ( #2404 ), #11135 ) ;
#21976 = EDGE_CURVE ( 'NONE', #82, #30802, #25947, .T. ) ;
#21977 = CARTESIAN_POINT ( 'NONE',  ( -3.044812012440131443, 216.5253028482142952, 79.10113791807857808 ) ) ;
#21978 = AXIS2_PLACEMENT_3D ( 'NONE', #18053, #2732, #4 ) ;
#21979 = ORIENTED_EDGE ( 'NONE', *, *, #13877, .T. ) ;
#21980 = CARTESIAN_POINT ( 'NONE',  ( 92.60208470531341618, 155.0000000000000000, -13.00000000000002487 ) ) ;
#21981 = ORIENTED_EDGE ( 'NONE', *, *, #4121, .T. ) ;
#21982 = CARTESIAN_POINT ( 'NONE',  ( -2.517493886308901807, 199.4062855549015012, 20.90113791807856813 ) ) ;
#21983 = CARTESIAN_POINT ( 'NONE',  ( -59.75427847806285797, 194.9412682558892982, -2.168710897896606760 ) ) ;
#21984 = EDGE_CURVE ( 'NONE', #17495, #30922, #33281, .T. ) ;
#21985 = CARTESIAN_POINT ( 'NONE',  ( -0.05014649552828403384, 217.5146222423826714, 6.248862081921433109 ) ) ;
#21986 = CARTESIAN_POINT ( 'NONE',  ( 52.27499999726880731, 160.0630714827496206, 15.58253174999999224 ) ) ;
#21987 = ORIENTED_EDGE ( 'NONE', *, *, #11473, .F. ) ;
#21988 = CARTESIAN_POINT ( 'NONE',  ( 55.02499999726881441, 149.9369285172503510, -15.58253175000000823 ) ) ;
#21989 = CARTESIAN_POINT ( 'NONE',  ( -8.015496119326531499, 204.4483345814780364, 48.35113791807857098 ) ) ;
#21990 = DIRECTION ( 'NONE',  ( -1.000000000000000000, -0.000000000000000000, -0.000000000000000000 ) ) ;
#21991 = PRESENTATION_LAYER_ASSIGNMENT (  '', '', ( #32884 ) ) ;
#21992 = LINE ( 'NONE', #5809, #3753 ) ;
#21993 = EDGE_CURVE ( 'NONE', #31781, #8611, #18119, .T. ) ;
#21994 = CARTESIAN_POINT ( 'NONE',  ( -3.135527875058982783, 216.4958274776886924, 93.09886208192145318 ) ) ;
#21995 = CARTESIAN_POINT ( 'NONE',  ( 62.97499999726881015, 140.1801316387863778, -4.815267126137194431 ) ) ;
#21996 = CARTESIAN_POINT ( 'NONE',  ( 8.118202686958039038, 212.8392687619912635, 34.70113791807857240 ) ) ;
#21997 = CARTESIAN_POINT ( 'NONE',  ( 7.499999999999999112, -1.443375672974070323, -7.063244554130001518 ) ) ;
#21998 = CARTESIAN_POINT ( 'NONE',  ( -9.680171189290716072, 199.9079932115567146, 83.19886208192144750 ) ) ;
#21999 = ADVANCED_FACE ( 'NONE', ( #2622 ), #4488, .F. ) ;
#22000 = AXIS2_PLACEMENT_3D ( 'NONE', #25526, #18091, #2195 ) ;
#22001 = CARTESIAN_POINT ( 'NONE',  ( 79.10000000000000853, 168.7903194862797420, 4.480746418436729606 ) ) ;
#22002 = CARTESIAN_POINT ( 'NONE',  ( -7.500000000000000000, -4.330127018922198090, -7.422398894150034288 ) ) ;
#22003 = CARTESIAN_POINT ( 'NONE',  ( 90.49452189536829394, 155.0000000000000000, 0.000000000000000000 ) ) ;
#22004 = CARTESIAN_POINT ( 'NONE',  ( 3.135527875058820690, 216.4958274776887492, 91.40113791807857524 ) ) ;
#22005 = CARTESIAN_POINT ( 'NONE',  ( 6.815830331203684089, -0.6610623347507956771, -6.171384342982605631 ) ) ;
#22006 = CARTESIAN_POINT ( 'NONE',  ( 42.27499999726880731, 160.0630714827496206, 15.58253174999999402 ) ) ;
#22007 = CARTESIAN_POINT ( 'NONE',  ( -6.220909254589537696, 198.5229672870051161, 33.05113791807857382 ) ) ;
#22008 = CARTESIAN_POINT ( 'NONE',  ( 77.62499999726880162, 171.3844434931184253, -7.942151717890132712E-15 ) ) ;
#22009 = ORIENTED_EDGE ( 'NONE', *, *, #23088, .F. ) ;
#22010 = CARTESIAN_POINT ( 'NONE',  ( 97.20416941062678973, 155.0000000000000000, -32.00000000000000000 ) ) ;
#22011 = CARTESIAN_POINT ( 'NONE',  ( 0.000000000000000000, 0.000000000000000000, -18.00000000000000000 ) ) ;
#22012 = CARTESIAN_POINT ( 'NONE',  ( 45.69999999453763451, 142.6655632788954620, -8.961492836873480528 ) ) ;
#22013 = CARTESIAN_POINT ( 'NONE',  ( -7.375838497908182134, 217.2372850707499765, 15.95113791807856707 ) ) ;
#22014 = CARTESIAN_POINT ( 'NONE',  ( 127.5000000000000000, 155.0000000000000000, -6.938893903907228378E-15 ) ) ;
#22015 = DIRECTION ( 'NONE',  ( -0.000000000000000000, -0.000000000000000000, 1.000000000000000000 ) ) ;
#22016 = ORIENTED_EDGE ( 'NONE', *, *, #4607, .T. ) ;
#22017 = CARTESIAN_POINT ( 'NONE',  ( -11.98450388067341876, 203.0532714938636047, 38.34886208192142476 ) ) ;
#22018 = CARTESIAN_POINT ( 'NONE',  ( 6.139770520408368348, 198.4640165459539674, 2.451137918078566180 ) ) ;
#22019 = CARTESIAN_POINT ( 'NONE',  ( 6.220909254589536808, 215.4770327129947702, 55.55113791807855961 ) ) ;
#22020 = ADVANCED_FACE ( 'NONE', ( #23402 ), #21334, .F. ) ;
#22021 = CARTESIAN_POINT ( 'NONE',  ( 6.500168698208244500, 202.3363017425938324, 10.29886208192143471 ) ) ;
#22022 = PRODUCT_DEFINITION_CONTEXT ( 'detailed design', #11815, 'design' ) ;
#22023 = PLANE ( 'NONE',  #25756 ) ;
#22024 = ORIENTED_EDGE ( 'NONE', *, *, #2094, .F. ) ;
#22025 = CARTESIAN_POINT ( 'NONE',  ( -0.05014649552828365914, 215.4116977939061144, 102.2488620819214447 ) ) ;
#22026 = EDGE_CURVE ( 'NONE', #15375, #4891, #3697, .T. ) ;
#22027 = DIRECTION ( 'NONE',  ( -0.000000000000000000, -0.000000000000000000, 1.000000000000000000 ) ) ;
#22028 = CARTESIAN_POINT ( 'NONE',  ( 8.000000000000008882, 206.9523078486586485, 44.00113791807857666 ) ) ;
#22029 = CARTESIAN_POINT ( 'NONE',  ( 109.0104235265664272, 155.0000000000000000, 0.000000000000000000 ) ) ;
#22030 = EDGE_LOOP ( 'NONE', ( #28055, #27307, #8411 ) ) ;
#22031 = CARTESIAN_POINT ( 'NONE',  ( 38.12499999726880873, 155.0000000000000000, 15.58253174999999402 ) ) ;
#22032 = CARTESIAN_POINT ( 'NONE',  ( 77.50000000000000000, 155.0000000000000000, -6.938893903907228378E-15 ) ) ;
#22033 = CARTESIAN_POINT ( 'NONE',  ( 0.05014649552828275708, 196.4853777576173002, 64.74886208192143044 ) ) ;
#22034 = CARTESIAN_POINT ( 'NONE',  ( 42.67499999726880588, 141.7447067706911810, 9.630534252274376428 ) ) ;
#22035 = DIRECTION ( 'NONE',  ( 0.000000000000000000, -0.04769215134145524809, -0.9988620819214351076 ) ) ;
#22036 = CARTESIAN_POINT ( 'NONE',  ( -7.984503880673488041, 209.6470497212046098, 99.65113791807858945 ) ) ;
#22037 = CARTESIAN_POINT ( 'NONE',  ( 62.89999999999999858, 168.7903194862797420, -4.480746418436745593 ) ) ;
#22038 = FACE_OUTER_BOUND ( 'NONE', #830, .T. ) ;
#22039 = CARTESIAN_POINT ( 'NONE',  ( 8.015496119326595448, 204.4483345814782638, 82.14886208192143613 ) ) ;
#22040 = CARTESIAN_POINT ( 'NONE',  ( -2.263183130831070589, 6.566419505188274996, -6.208110906918258287 ) ) ;
#22041 = CARTESIAN_POINT ( 'NONE',  ( -60.00000000000000000, -7.347880794884118356E-15, 20.00000000000001776 ) ) ;
#22042 = EDGE_CURVE ( 'NONE', #26876, #3255, #14545, .T. ) ;
#22043 = CARTESIAN_POINT ( 'NONE',  ( 59.72499999726881015, 169.8198683612136222, 4.815267126137181997 ) ) ;
#22045 = ORIENTED_EDGE ( 'NONE', *, *, #4396, .T. ) ;
#22044 = CARTESIAN_POINT ( 'NONE',  ( 3.044812012440130555, 197.4746971517856764, 20.60113791807856742 ) ) ;
#22046 = DIRECTION ( 'NONE',  ( -1.000000000000000000, 0.000000000000000000, 0.000000000000000000 ) ) ;
#22047 = CARTESIAN_POINT ( 'NONE',  ( 80.67499999726881299, 141.7447067706911810, 9.630534252274376428 ) ) ;
#22048 = CARTESIAN_POINT ( 'NONE',  ( 11.98450388067348271, 203.0532714938637753, 86.15113791807856103 ) ) ;
#22049 = EDGE_CURVE ( 'NONE', #7505, #7334, #30254, .T. ) ;
#22050 = CARTESIAN_POINT ( 'NONE',  ( 32.50000000000000000, 155.0000000000000000, 15.00000000000001243 ) ) ;
#22051 = FACE_OUTER_BOUND ( 'NONE', #25713, .T. ) ;
#22052 = EDGE_LOOP ( 'NONE', ( #8484, #27040, #9501, #871, #5995 ) ) ;
#22053 = CARTESIAN_POINT ( 'NONE',  ( 9.680171189290716072, 214.0920067884432854, 57.69886208192144039 ) ) ;
#22054 = CARTESIAN_POINT ( 'NONE',  ( -0.05014649552828402690, 217.5146222423826714, 72.24886208192143044 ) ) ;
#22055 = CARTESIAN_POINT ( 'NONE',  ( 7.375838497908012492, 217.2372850707501186, 9.548862081921432932 ) ) ;
#22056 = DIRECTION ( 'NONE',  ( 1.000000000000000000, 0.000000000000000000, 0.000000000000000000 ) ) ;
#22057 = CARTESIAN_POINT ( 'NONE',  ( -6.139770520408369237, 215.5359834540460042, 21.95113791807856884 ) ) ;
#22058 = ADVANCED_FACE ( 'NONE', ( #6928 ), #14596, .F. ) ;
#22059 = CARTESIAN_POINT ( 'NONE',  ( -3.135527875058982783, 216.4958274776886924, 90.09886208192143897 ) ) ;
#22060 =( REPRESENTATION_RELATIONSHIP ('NONE','NONE', #25663, #30243 ) REPRESENTATION_RELATIONSHIP_WITH_TRANSFORMATION ( #9680 )SHAPE_REPRESENTATION_RELATIONSHIP( ) );
#22061 = ORIENTED_EDGE ( 'NONE', *, *, #164, .F. ) ;
#22062 = PLANE ( 'NONE',  #3983 ) ;
#22063 = EDGE_LOOP ( 'NONE', ( #25447, #12353, #25932, #15867 ) ) ;
#22064 = LINE ( 'NONE', #16781, #420 ) ;
#22065 = CARTESIAN_POINT ( 'NONE',  ( 2.426778023690075337, 214.6231898156240447, 75.39886208192143613 ) ) ;
#22066 = VERTEX_POINT ( 'NONE', #20388 ) ;
#22067 = CARTESIAN_POINT ( 'NONE',  ( 83.22499999726881015, 160.0630714827496206, -15.58253175000000823 ) ) ;
#22068 = EDGE_LOOP ( 'NONE', ( #30490, #19678, #27974, #27248 ) ) ;
#22069 = CARTESIAN_POINT ( 'NONE',  ( -125.0000000000000000, 0.000000000000000000, 20.00000000000000000 ) ) ;
#22070 = CARTESIAN_POINT ( 'NONE',  ( 75.22499999726879594, 160.0630714827496206, -15.58253175000000823 ) ) ;
#22071 = DIRECTION ( 'NONE',  ( -0.000000000000000000, -0.000000000000000000, 1.000000000000000000 ) ) ;
#22072 = CARTESIAN_POINT ( 'NONE',  ( -2.426778023690262742, 214.6231898156240163, 67.10113791807857808 ) ) ;
#22073 = CARTESIAN_POINT ( 'NONE',  ( 87.50000000000000000, 170.0518911780263807, 2.651152351506866012 ) ) ;
#22074 = CARTESIAN_POINT ( 'NONE',  ( 36.90000000000000568, 168.7903194862797420, -4.480746418436745593 ) ) ;
#22075 = CARTESIAN_POINT ( 'NONE',  ( 2.426778023690075337, 214.6231898156240447, 45.39886208192144323 ) ) ;
#22076 = EDGE_CURVE ( 'NONE', #2474, #7112, #29164, .T. ) ;
#22077 = CARTESIAN_POINT ( 'NONE',  ( 3.135527875058820690, 216.4958274776887492, 76.40113791807857524 ) ) ;
#22078 = EDGE_CURVE ( 'NONE', #27344, #25544, #10238, .T. ) ;
#22079 = CARTESIAN_POINT ( 'NONE',  ( -64.50000000000000000, 2.605762844159070557, 20.00000000000000000 ) ) ;
#22080 = CARTESIAN_POINT ( 'NONE',  ( 0.000000000000000000, 0.000000000000000000, -2.874600000000001376 ) ) ;
#22081 = DIRECTION ( 'NONE',  ( 0.000000000000000000, 0.000000000000000000, -1.000000000000000000 ) ) ;
#22082 = CARTESIAN_POINT ( 'NONE',  ( 49.12499999726880873, 155.0000000000000000, -15.58253175000000823 ) ) ;
#22083 = CARTESIAN_POINT ( 'NONE',  ( 7.375838497908181246, 196.7627149292499666, 59.45113791807857240 ) ) ;
#22084 = CARTESIAN_POINT ( 'NONE',  ( -54.50000000000002132, 155.0000000000000000, 6.938893903907228378E-15 ) ) ;
#22085 = EDGE_CURVE ( 'NONE', #16190, #27924, #22630, .T. ) ;
#22086 = CARTESIAN_POINT ( 'NONE',  ( 9.736236675707914401, 214.0148392665762458, 4.701137918078565292 ) ) ;
#22087 = ADVANCED_FACE ( 'NONE', ( #14933 ), #10004, .F. ) ;
#22088 = CARTESIAN_POINT ( 'NONE',  ( -3.135527875058821579, 197.5041725223112223, 65.90113791807857524 ) ) ;
#22089 = CARTESIAN_POINT ( 'NONE',  ( 12.00000000000000711, 207.0476921513415220, 33.99886208192143044 ) ) ;
#22090 = CARTESIAN_POINT ( 'NONE',  ( 3.044812012439969795, 216.5253028482143520, 48.39886208192143613 ) ) ;
#22091 = CARTESIAN_POINT ( 'NONE',  ( 83.99999999453763166, 155.0000000000000000, -14.50000000000000711 ) ) ;
#22092 = CARTESIAN_POINT ( 'NONE',  ( 9.680171189290831535, 199.9079932115568852, 80.30113791807858092 ) ) ;
#22093 = CARTESIAN_POINT ( 'NONE',  ( 2.426778023690261410, 199.3768101843759837, 98.60113791807857808 ) ) ;
#22094 = CARTESIAN_POINT ( 'NONE',  ( 3.135527875058981895, 197.5041725223112792, 64.59886208192143897 ) ) ;
#22095 = CARTESIAN_POINT ( 'NONE',  ( 7.263825692932297962, 4.945657111639574666, -7.907570769506046204 ) ) ;
#22096 = ORIENTED_EDGE ( 'NONE', *, *, #16415, .F. ) ;
#22097 = CARTESIAN_POINT ( 'NONE',  ( 12.00000000000000711, 207.0476921513415220, 63.99886208192143044 ) ) ;
#22098 = ORIENTED_EDGE ( 'NONE', *, *, #32005, .T. ) ;
#22099 = CARTESIAN_POINT ( 'NONE',  ( 74.87499999726880162, 138.6155565068815463, -3.929120461958505118E-15 ) ) ;
#22100 = CARTESIAN_POINT ( 'NONE',  ( 8.015496119326595448, 204.4483345814782638, 40.14886208192143613 ) ) ;
#22101 = ORIENTED_EDGE ( 'NONE', *, *, #23673, .F. ) ;
#22102 = CIRCLE ( 'NONE', #20484, 1.033333333332998372 ) ;
#22103 = CARTESIAN_POINT ( 'NONE',  ( 81.07499999726880446, 141.7447067706911810, -9.630534252274387086 ) ) ;
#22104 = DIRECTION ( 'NONE',  ( 0.000000000000000000, 0.000000000000000000, -1.000000000000000000 ) ) ;
#22105 = CLOSED_SHELL ( 'NONE', ( #33035, #8972, #24585, #14136, #26238, #8564, #27276, #16752, #1253, #18298, #12229, #21847, #26376, #10038, #20969, #11682, #29366, #30567, #14736, #10807 ) ) ;
#22106 = CARTESIAN_POINT ( 'NONE',  ( 79.50000000000000000, 155.0000000000000000, -6.938893903907228378E-15 ) ) ;
#22107 = CARTESIAN_POINT ( 'NONE',  ( -2.517493886308901807, 199.4062855549015012, 47.90113791807857524 ) ) ;
#22108 = CARTESIAN_POINT ( 'NONE',  ( 8.062137200540822946, 212.9164362838583315, 45.69886208192143329 ) ) ;
#22109 = CARTESIAN_POINT ( 'NONE',  ( 71.87499999726881583, 171.3844434931184253, -7.942151717890134290E-15 ) ) ;
#22110 = ORIENTED_EDGE ( 'NONE', *, *, #7897, .F. ) ;
#22111 = AXIS2_PLACEMENT_3D ( 'NONE', #3974, #27151, #2106 ) ;
#22112 = FACE_OUTER_BOUND ( 'NONE', #19963, .T. ) ;
#22113 = CARTESIAN_POINT ( 'NONE',  ( 4.000000000000000000, 0.000000000000000000, -25.03750572909317285 ) ) ;
#22114 = CARTESIAN_POINT ( 'NONE',  ( 86.61132485994281183, 159.8737954434933499, 15.00000000000019895 ) ) ;
#22115 = CARTESIAN_POINT ( 'NONE',  ( -2.426778023690076225, 199.3768101843759553, 13.89886208192143613 ) ) ;
#22116 = CARTESIAN_POINT ( 'NONE',  ( 0.05014649552810505201, 217.5146222423826714, 61.25113791807856245 ) ) ;
#22117 = CARTESIAN_POINT ( 'NONE',  ( -10.00000000000000711, 207.0476921513413515, 51.50113791807857666 ) ) ;
#22118 = FACE_OUTER_BOUND ( 'NONE', #14404, .T. ) ;
#22119 = CARTESIAN_POINT ( 'NONE',  ( -8.101690028313589309, 224.0100459381558267, 105.4832055762867782 ) ) ;
#22120 = CARTESIAN_POINT ( 'NONE',  ( 44.72499999726881015, 140.1801316387863778, -4.815267126137194431 ) ) ;
#22121 = SURFACE_STYLE_USAGE ( .BOTH. , #11734 ) ;
#22122 = CARTESIAN_POINT ( 'NONE',  ( 87.50000000000000000, 153.6504441981042532, -15.26259659777053912 ) ) ;
#22123 = CARTESIAN_POINT ( 'NONE',  ( 3.662846001190051659, 195.5725841191953691, 23.60113791807857098 ) ) ;
#22124 = DIRECTION ( 'NONE',  ( -1.000000000000000000, -0.000000000000000000, -0.000000000000000000 ) ) ;
#22125 = CARTESIAN_POINT ( 'NONE',  ( 3.044812012440130555, 197.4746971517856764, 71.60113791807857808 ) ) ;
#22126 = CARTESIAN_POINT ( 'NONE',  ( 8.118202686958039038, 212.8392687619912635, 37.70113791807857240 ) ) ;
#22127 = CARTESIAN_POINT ( 'NONE',  ( 76.78867513459483973, 155.0000000000000000, -15.00000000000002487 ) ) ;
#22128 = CARTESIAN_POINT ( 'NONE',  ( -63.50000000000004263, 215.0000000000000000, 0.000000000000000000 ) ) ;
#22129 = CARTESIAN_POINT ( 'NONE',  ( -7.456977232089471386, 217.1783343296987709, 2.948862081921434175 ) ) ;
#22130 = CARTESIAN_POINT ( 'NONE',  ( 8.062137200540822946, 212.9164362838583315, 21.69886208192143684 ) ) ;
#22131 = CARTESIAN_POINT ( 'NONE',  ( 67.89999999453763735, 150.2886644046228639, -14.50000000000000888 ) ) ;
#22132 = ORIENTED_EDGE ( 'NONE', *, *, #26000, .T. ) ;
#22133 = CARTESIAN_POINT ( 'NONE',  ( -9.680171189290831535, 214.0920067884431148, 51.80113791807857382 ) ) ;
#22134 = CARTESIAN_POINT ( 'NONE',  ( -0.05014649552807731031, 198.5883022060938572, 65.75113791807856956 ) ) ;
#22135 = CARTESIAN_POINT ( 'NONE',  ( 3.135527875058981895, 197.5041725223112792, 31.59886208192143187 ) ) ;
#22136 = CARTESIAN_POINT ( 'NONE',  ( 45.41132485994281609, 142.2402378747194405, -9.270509831248439525 ) ) ;
#22137 = CONICAL_SURFACE ( 'NONE', #4183, 37.00000000000000711, 0.7853981633974482790 ) ;
#22138 = EDGE_LOOP ( 'NONE', ( #19266, #10840, #1154, #14223 ) ) ;
#22139 = CARTESIAN_POINT ( 'NONE',  ( -6.220909254589537696, 198.5229672870051161, 87.05113791807856671 ) ) ;
#22140 = ORIENTED_EDGE ( 'NONE', *, *, #30412, .T. ) ;
#22141 = CARTESIAN_POINT ( 'NONE',  ( 87.49999999999997158, 168.5097963921330120, -7.831877679450401253 ) ) ;
#22142 = CARTESIAN_POINT ( 'NONE',  ( -1.994931997373328159E-14, -8.660254037844390851, -1.000000000000000888 ) ) ;
#22143 = ORIENTED_EDGE ( 'NONE', *, *, #24249, .T. ) ;
#22144 = CARTESIAN_POINT ( 'NONE',  ( -2.426778023690262742, 214.6231898156240163, 25.10113791807856742 ) ) ;
#22145 = AXIS2_PLACEMENT_3D ( 'NONE', #2056, #1544, #32709 ) ;
#22146 = DIRECTION ( 'NONE',  ( -1.000000000000000000, 1.224646799147354686E-16, 0.000000000000000000 ) ) ;
#22147 = VECTOR ( 'NONE', #24794, 1000.000000000000227 ) ;
#22148 = CARTESIAN_POINT ( 'NONE',  ( -10.01549611932659722, 210.2015048109875011, 5.648862081921435241 ) ) ;
#22149 = CARTESIAN_POINT ( 'NONE',  ( 47.97499999726881015, 169.8198683612136222, 4.815267126137181997 ) ) ;
#22150 = VERTEX_POINT ( 'NONE', #19870 ) ;
#22151 = CARTESIAN_POINT ( 'NONE',  ( -0.05014649552807731031, 198.5883022060938572, 50.75113791807857666 ) ) ;
#22152 = DIRECTION ( 'NONE',  ( -0.000000000000000000, -0.000000000000000000, 1.000000000000000000 ) ) ;
#22153 = AXIS2_PLACEMENT_3D ( 'NONE', #1834, #14775, #22613 ) ;
#22154 = SURFACE_STYLE_USAGE ( .BOTH. , #27269 ) ;
#22155 = CARTESIAN_POINT ( 'NONE',  ( -16.09259079475562970, 22.46320317811876421, 1.931235119739804773E-15 ) ) ;
#22156 = CARTESIAN_POINT ( 'NONE',  ( -9.984503880673420539, 203.7031108863293980, 92.34886208192141055 ) ) ;
#22157 = CARTESIAN_POINT ( 'NONE',  ( 61.37499999726880873, 155.0000000000000000, -15.58253175000000823 ) ) ;
#22158 = CARTESIAN_POINT ( 'NONE',  ( 3.135527875058820690, 216.4958274776887492, 28.40113791807856813 ) ) ;
#22159 = CARTESIAN_POINT ( 'NONE',  ( 0.000000000000000000, 4.163799117101000559E-16, -3.299999999999999822 ) ) ;
#22160 = CARTESIAN_POINT ( 'NONE',  ( 12.00000000000000711, 207.0476921513415220, 75.99886208192144466 ) ) ;
#22161 = AXIS2_PLACEMENT_3D ( 'NONE', #13202, #23602, #9263 ) ;
#22162 = DIRECTION ( 'NONE',  ( 1.224646799147353207E-16, -4.064521778635712183E-50, -1.000000000000000000 ) ) ;
#22163 = CARTESIAN_POINT ( 'NONE',  ( 81.59999999999999432, 150.2886644046228639, 14.49999999999999645 ) ) ;
#22164 = CARTESIAN_POINT ( 'NONE',  ( -56.96409840163092753, 194.9506684299840913, -1.999309141333601492 ) ) ;
#22165 = CARTESIAN_POINT ( 'NONE',  ( 4.000000000000000000, 3.518949890710768802, -4.770489558936219510E-15 ) ) ;
#22166 = CARTESIAN_POINT ( 'NONE',  ( 9.984503880673470277, 203.7031108863295401, 95.15113791807854682 ) ) ;
#22167 = CARTESIAN_POINT ( 'NONE',  ( 117.5000000000000000, 155.0000000000000000, 112.0000000000000426 ) ) ;
#22168 = CARTESIAN_POINT ( 'NONE',  ( 47.67499999726880588, 168.2552932293087906, -9.630534252274385310 ) ) ;
#22169 = CARTESIAN_POINT ( 'NONE',  ( 10.01549611932653860, 210.2015048109876716, 34.85113791807856387 ) ) ;
#22170 = CARTESIAN_POINT ( 'NONE',  ( 82.02499999726879309, 160.0630714827496206, 15.58253174999999402 ) ) ;
#22171 = FACE_OUTER_BOUND ( 'NONE', #32406, .T. ) ;
#22172 = DIRECTION ( 'NONE',  ( -0.000000000000000000, -0.000000000000000000, -1.000000000000000000 ) ) ;
#22173 = CARTESIAN_POINT ( 'NONE',  ( 46.99999999453763166, 155.0000000000000000, 14.49999999999999467 ) ) ;
#22174 = ORIENTED_EDGE ( 'NONE', *, *, #7029, .T. ) ;
#22175 = SHAPE_REPRESENTATION ( 'socket head cap screw_iso_ISO 4762 M4 x 12 - 12N', ( #2404 ), #1885 ) ;
#22176 = CARTESIAN_POINT ( 'NONE',  ( -7.456977232089304408, 196.8216656703010301, 15.05113791807856849 ) ) ;
#22177 = AXIS2_PLACEMENT_3D ( 'NONE', #2740, #23505, #172 ) ;
#22178 = CARTESIAN_POINT ( 'NONE',  ( 60.71132485994280614, 155.0000000000000000, 15.00000000000001243 ) ) ;
#22179 = EDGE_CURVE ( 'NONE', #25924, #30416, #27598, .T. ) ;
#22180 = AXIS2_PLACEMENT_3D ( 'NONE', #3247, #18921, #29146 ) ;
#22181 = CARTESIAN_POINT ( 'NONE',  ( 66.51132485994278909, 163.8167787843871110, 12.13525491562421621 ) ) ;
#22182 = ORIENTED_EDGE ( 'NONE', *, *, #26661, .T. ) ;
#22183 = CARTESIAN_POINT ( 'NONE',  ( -12.01549611932659722, 210.8513442034533227, 41.64886208192143613 ) ) ;
#22184 = CARTESIAN_POINT ( 'NONE',  ( 3.135527875058820690, 216.4958274776887492, 1.401137918078565914 ) ) ;
#22185 = CARTESIAN_POINT ( 'NONE',  ( 3.135527875058820690, 216.4958274776887492, 61.40113791807857524 ) ) ;
#22186 = CARTESIAN_POINT ( 'NONE',  ( -8.000000000000008882, 206.9523078486584780, 11.49886208192143577 ) ) ;
#22187 = VECTOR ( 'NONE', #13954, 1000.000000000000000 ) ;
#22188 = CARTESIAN_POINT ( 'NONE',  ( 18.00000000000000000, 0.000000000000000000, 3.252606517456513302E-15 ) ) ;
#22189 = VERTEX_POINT ( 'NONE', #15269 ) ;
#22190 = CARTESIAN_POINT ( 'NONE',  ( -7.984503880673422316, 204.3529502787951628, 98.34886208192145318 ) ) ;
#22191 = CARTESIAN_POINT ( 'NONE',  ( 2.000000000000000000, -1.773042676681340524, 1.734723475976807094E-15 ) ) ;
#22192 = CARTESIAN_POINT ( 'NONE',  ( -2.426778023690262742, 214.6231898156240163, 40.10113791807857098 ) ) ;
#22193 = FACE_OUTER_BOUND ( 'NONE', #12895, .T. ) ;
#22194 = ORIENTED_EDGE ( 'NONE', *, *, #22411, .T. ) ;
#22195 = CARTESIAN_POINT ( 'NONE',  ( 36.22499999726881015, 149.9369285172503510, 15.58253174999999580 ) ) ;
#22196 = CARTESIAN_POINT ( 'NONE',  ( 103.4083388212532810, 155.0000000000000000, 0.000000000000000000 ) ) ;
#22197 = DIRECTION ( 'NONE',  ( 0.000000000000000000, 0.000000000000000000, 1.000000000000000000 ) ) ;
#22198 = AXIS2_PLACEMENT_3D ( 'NONE', #10650, #87, #8581 ) ;
#22199 = CARTESIAN_POINT ( 'NONE',  ( -8.062137200540822946, 201.0835637161416400, 59.19886208192144039 ) ) ;
#22200 = CARTESIAN_POINT ( 'NONE',  ( 43.57499999726881157, 164.1591823560292198, -12.60653300113719766 ) ) ;
#22201 = CARTESIAN_POINT ( 'NONE',  ( 0.000000000000000000, 0.000000000000000000, -10.00000000000000000 ) ) ;
#22202 = CARTESIAN_POINT ( 'NONE',  ( -3.135527875058821579, 197.5041725223112223, -0.09886208192143428053 ) ) ;
#22203 = PRODUCT ( 'hex flange nut gradea_iso_ISO - 4161 - M10 - N', 'hex flange nut gradea_iso_ISO - 4161 - M10 - N', '', ( #28120 ) ) ;
#22204 = AXIS2_PLACEMENT_3D ( 'NONE', #28781, #20264, #31014 ) ;
#22205 = CARTESIAN_POINT ( 'NONE',  ( 60.99999999999999289, 170.2462022514548323, -7.872454543227099337E-15 ) ) ;
#22206 = CARTESIAN_POINT ( 'NONE',  ( 0.000000000000000000, 0.000000000000000000, -18.00000000000000000 ) ) ;
#22207 = CARTESIAN_POINT ( 'NONE',  ( -8.000000000000008882, 206.9523078486584780, 80.49886208192144466 ) ) ;
#22208 = CARTESIAN_POINT ( 'NONE',  ( -4.927659837809095222, 206.3103720916592465, -5.504302862921502282 ) ) ;
#22209 = CARTESIAN_POINT ( 'NONE',  ( 99.30625411593993590, 155.0000000000000000, -12.00000000000001066 ) ) ;
#22210 = AXIS2_PLACEMENT_3D ( 'NONE', #14456, #24852, #11912 ) ;
#22211 = CARTESIAN_POINT ( 'NONE',  ( 66.42499999726879878, 141.7447067706911810, 9.630534252274376428 ) ) ;
#22213 = EDGE_LOOP ( 'NONE', ( #9914, #1368, #7287, #33293 ) ) ;
#22212 = CARTESIAN_POINT ( 'NONE',  ( -0.05014649552810635652, 196.4853777576173002, 23.75113791807856245 ) ) ;
#22214 = DIRECTION ( 'NONE',  ( 0.000000000000000000, 0.7071067811865442421, -0.7071067811865506814 ) ) ;
#22215 = CARTESIAN_POINT ( 'NONE',  ( 85.67499999726879878, 168.2552932293087906, -9.630534252274385310 ) ) ;
#22216 = CARTESIAN_POINT ( 'NONE',  ( -3.753561863808691168, 195.6020594897209435, 86.90113791807857524 ) ) ;
#22217 = CARTESIAN_POINT ( 'NONE',  ( 115.4999999999999858, 63.20130719884917170, -52.99999999999946709 ) ) ;
#22218 = EDGE_CURVE ( 'NONE', #24997, #4641, #2330, .T. ) ;
#22219 = ORIENTED_EDGE ( 'NONE', *, *, #3737, .T. ) ;
#22220 = CARTESIAN_POINT ( 'NONE',  ( 9.736236675708031640, 199.9851607334238963, 70.29886208192142760 ) ) ;
#22221 = CARTESIAN_POINT ( 'NONE',  ( 8.118202686958138514, 201.1607312380088501, 73.29886208192142760 ) ) ;
#22222 = CARTESIAN_POINT ( 'NONE',  ( -12.00000000000000711, 206.9523078486584780, 14.49886208192143577 ) ) ;
#22223 = CYLINDRICAL_SURFACE ( 'NONE', #2876, 15.00000000000001776 ) ;
#22224 = AXIS2_PLACEMENT_3D ( 'NONE', #142, #15968, #25867 ) ;
#22225 = CARTESIAN_POINT ( 'NONE',  ( 6.220909254589536808, 215.4770327129947702, 22.55113791807856671 ) ) ;
#22226 = CARTESIAN_POINT ( 'NONE',  ( -1.452965002680439266, 3.202582148906723436, -2.900000000000002132 ) ) ;
#22227 = CARTESIAN_POINT ( 'NONE',  ( 3.135527875058981895, 197.5041725223112792, 88.59886208192143897 ) ) ;
#22228 = CIRCLE ( 'NONE', #11895, 24.99999999999999289 ) ;
#22229 = EDGE_CURVE ( 'NONE', #12386, #6526, #12036, .T. ) ;
#22230 = CARTESIAN_POINT ( 'NONE',  ( -1.474514954580286030E-14, 206.9977241638431167, -6.000000000000014211 ) ) ;
#22231 = VERTEX_POINT ( 'NONE', #7103 ) ;
#22232 = DIRECTION ( 'NONE',  ( 1.000000000000000000, 0.000000000000000000, 0.000000000000000000 ) ) ;
#22233 = CARTESIAN_POINT ( 'NONE',  ( -8.000000000000008882, 206.9523078486584780, 74.49886208192144466 ) ) ;
#22234 = EDGE_LOOP ( 'NONE', ( #23164, #27008, #3166, #17252 ) ) ;
#22235 = CARTESIAN_POINT ( 'NONE',  ( 86.52499999726882152, 140.1801316387863778, 4.815267126137185549 ) ) ;
#22236 = ORIENTED_EDGE ( 'NONE', *, *, #15640, .F. ) ;
#22237 = CARTESIAN_POINT ( 'NONE',  ( 0.000000000000000000, 0.000000000000000000, -7.974599999999998801 ) ) ;
#22238 = CARTESIAN_POINT ( 'NONE',  ( 77.32499999726881867, 164.1591823560292198, -12.60653300113719766 ) ) ;
#22239 = ADVANCED_FACE ( 'NONE', ( #32814 ), #12852, .T. ) ;
#22240 = DIRECTION ( 'NONE',  ( 1.000000000000000000, 0.000000000000000000, 0.000000000000000000 ) ) ;
#22241 = CARTESIAN_POINT ( 'NONE',  ( -8.000000000000008882, 207.0476921513413515, 81.50113791807856956 ) ) ;
#22242 = CARTESIAN_POINT ( 'NONE',  ( 75.78867513459483973, 155.0000000000000000, 15.00000000000001243 ) ) ;
#22243 = CARTESIAN_POINT ( 'NONE',  ( 39.69999999999999574, 146.4771138417591203, 11.73074641843673227 ) ) ;
#22244 = CARTESIAN_POINT ( 'NONE',  ( 2.426778023690075337, 214.6231898156240447, 51.39886208192145745 ) ) ;
#22245 = VECTOR ( 'NONE', #3818, 1000.000000000000114 ) ;
#22246 = EDGE_CURVE ( 'NONE', #9697, #28610, #14754, .T. ) ;
#22247 = AXIS2_PLACEMENT_3D ( 'NONE', #12608, #17211, #27440 ) ;
#22248 = CARTESIAN_POINT ( 'NONE',  ( -6.220909254589537696, 198.5229672870051161, 30.05113791807856671 ) ) ;
#22249 = CARTESIAN_POINT ( 'NONE',  ( -0.3755270751584372513, 206.3102596154024297, 117.9458888342408898 ) ) ;
#22250 = CARTESIAN_POINT ( 'NONE',  ( 72.91132485994280898, 146.1832212156128890, 12.13525491562421976 ) ) ;
#22251 = DIRECTION ( 'NONE',  ( 1.000000000000000000, 0.000000000000000000, 0.000000000000000000 ) ) ;
#22252 = CARTESIAN_POINT ( 'NONE',  ( 54.12499999726881583, 155.0000000000000000, 15.58253174999999402 ) ) ;
#22253 = CARTESIAN_POINT ( 'NONE',  ( 65.57499999726881867, 164.1591823560292198, -12.60653300113719766 ) ) ;
#22254 = CARTESIAN_POINT ( 'NONE',  ( -7.375838497908182134, 217.2372850707499765, 54.95113791807855819 ) ) ;
#22255 = CARTESIAN_POINT ( 'NONE',  ( -125.6872233929727827, -5.250000000000002665, 35.00001199999999812 ) ) ;
#22256 = CARTESIAN_POINT ( 'NONE',  ( 3.135527875058820690, 216.4958274776887492, 100.4011379180785752 ) ) ;
#22257 = CARTESIAN_POINT ( 'NONE',  ( 10.00000000000000711, 206.9523078486586201, 80.00113791807856956 ) ) ;
#22258 = CIRCLE ( 'NONE', #13557, 0.9999999999999992228 ) ;
#22259 = CARTESIAN_POINT ( 'NONE',  ( 0.05014649552828288198, 194.3824533091408000, 40.74886208192143044 ) ) ;
#22260 = CARTESIAN_POINT ( 'NONE',  ( -10.00000000000000711, 206.9523078486584495, 47.49886208192143755 ) ) ;
#22261 = CARTESIAN_POINT ( 'NONE',  ( 84.49999999453764588, 170.2462022514548323, -7.872454543227099337E-15 ) ) ;
#22262 = CARTESIAN_POINT ( 'NONE',  ( -9.680171189290831535, 214.0920067884431148, 90.80113791807858092 ) ) ;
#22263 = CARTESIAN_POINT ( 'NONE',  ( -8.015496119326531499, 204.4483345814780364, 99.35113791807857808 ) ) ;
#22264 = CARTESIAN_POINT ( 'NONE',  ( 0.05014649552828275708, 196.4853777576173002, 64.74886208192143044 ) ) ;
#22265 = B_SPLINE_CURVE_WITH_KNOTS ( 'NONE', 3,
 ( #678, #1174, #3393, #521, #19070, #8507, #13788, #11571 ),
 .UNSPECIFIED., .F., .F.,
 ( 4, 2, 2, 4 ),
 ( 2.459764730912720885E-07, 0.001920659145285728234, 0.002880865729692047052, 0.003841072314098365435 ),
 .UNSPECIFIED. ) ;
#22266 = SURFACE_SIDE_STYLE ('',( #6254 ) ) ;
#22267 = ORIENTED_EDGE ( 'NONE', *, *, #10985, .F. ) ;
#22268 = CARTESIAN_POINT ( 'NONE',  ( 9.680171189290716072, 214.0920067884432854, 66.69886208192143329 ) ) ;
#22269 = ORIENTED_EDGE ( 'NONE', *, *, #6479, .T. ) ;
#22270 = CARTESIAN_POINT ( 'NONE',  ( 70.77499999726880731, 140.1801316387863778, 4.815267126137185549 ) ) ;
#22271 = CARTESIAN_POINT ( 'NONE',  ( -7.984503880673422316, 204.3529502787951628, 44.34886208192144608 ) ) ;
#22272 = EDGE_LOOP ( 'NONE', ( #20262, #24276, #21170, #3208 ) ) ;
#22273 = EDGE_CURVE ( 'NONE', #6680, #5826, #2520, .T. ) ;
#22274 = ADVANCED_FACE ( 'NONE', ( #25661 ), #30781, .T. ) ;
#22275 = CARTESIAN_POINT ( 'NONE',  ( 84.97499999726882436, 140.1801316387863778, -4.815267126137194431 ) ) ;
#22276 = CARTESIAN_POINT ( 'NONE',  ( -31.74999999999995737, 6.123233995736768255E-16, -5.000000000000001776 ) ) ;
#22277 = LINE ( 'NONE', #6443, #31261 ) ;
#22278 = CARTESIAN_POINT ( 'NONE',  ( -6.500168698208129925, 202.3363017425936050, 63.20113791807857240 ) ) ;
#22279 = ADVANCED_FACE ( 'NONE', ( #10171 ), #25393, .T. ) ;
#22280 = CARTESIAN_POINT ( 'NONE',  ( -3.755786496842903988E-16, -7.505553499465146494, -8.000000000000000000 ) ) ;
#22281 = CARTESIAN_POINT ( 'NONE',  ( -9.984503880673420539, 203.7031108863293980, 47.34886208192143187 ) ) ;
#22282 = EDGE_LOOP ( 'NONE', ( #11101, #1489, #17722, #22393 ) ) ;
#22283 = PLANE ( 'NONE',  #31428 ) ;
#22284 =( BOUNDED_CURVE ( )  B_SPLINE_CURVE ( 2, ( #7016, #6332, #3787, #12625, #33245, #33585, #25578, #18081, #30699, #12289, #25403 ),
 .UNSPECIFIED., .F., .F. ) 
 B_SPLINE_CURVE_WITH_KNOTS ( ( 3, 2, 2, 2, 2, 3 ),
 ( 0.3214285714285715634, 0.3250000000000000666, 0.3285714285714285698, 0.3321428571428571286, 0.3357142857142856318, 0.3392857142857141906 ),
 .UNSPECIFIED. ) 
 CURVE ( )  GEOMETRIC_REPRESENTATION_ITEM ( )  RATIONAL_B_SPLINE_CURVE ( ( 0.9999999999999984457, 0.9510565162951549745, 1.000000000000000000, 0.9510565162951534202, 1.000000000000000000, 0.9510565162951534202, 1.000000000000000000, 0.9510565162951534202, 1.000000000000000000, 0.9510565162951549745, 0.9999999999999984457 ) ) 
 REPRESENTATION_ITEM ( '' )  );
#22285 = DIRECTION ( 'NONE',  ( -1.000000000000000000, -0.000000000000000000, -0.000000000000000000 ) ) ;
#22286 = CARTESIAN_POINT ( 'NONE',  ( 86.11132485994279762, 169.2658477444273331, -4.635254915624224203 ) ) ;
#22287 = CARTESIAN_POINT ( 'NONE',  ( -7.984503880673422316, 204.3529502787951628, 23.34886208192143542 ) ) ;
#22288 = ADVANCED_FACE ( 'NONE', ( #16388 ), #2001, .T. ) ;
#22289 = CARTESIAN_POINT ( 'NONE',  ( -10.00000000000000711, 207.0476921513413515, 57.50113791807856956 ) ) ;
#22290 = CARTESIAN_POINT ( 'NONE',  ( -8.118202686958039038, 201.1607312380087080, 45.20113791807857240 ) ) ;
#22291 = CARTESIAN_POINT ( 'NONE',  ( 71.71132485994280614, 155.0000000000000000, -15.00000000000002487 ) ) ;
#22292 = CARTESIAN_POINT ( 'NONE',  ( 10.01549611932653860, 210.2015048109876716, 22.85113791807856742 ) ) ;
#22293 = CARTESIAN_POINT ( 'NONE',  ( -7.984503880673422316, 204.3529502787951628, 101.3488620819214390 ) ) ;
#22294 = CARTESIAN_POINT ( 'NONE',  ( 42.62499999726881583, 138.6155565068815463, -3.929120461958505118E-15 ) ) ;
#22295 = CARTESIAN_POINT ( 'NONE',  ( -5.450967621166011412, 4.358435876041001578, -0.3607371497494529233 ) ) ;
#22296 = CARTESIAN_POINT ( 'NONE',  ( 87.49999999999997158, 160.3090467171700482, -14.64008245857240276 ) ) ;
#22297 = CARTESIAN_POINT ( 'NONE',  ( -12.01549611932652972, 203.1486557965464499, 27.35113791807856742 ) ) ;
#22298 = CARTESIAN_POINT ( 'NONE',  ( 81.88867513459483405, 150.1262045565062806, 14.99999999999992006 ) ) ;
#22299 = CARTESIAN_POINT ( 'NONE',  ( -9.984503880673473830, 210.2968891136704315, 78.65113791807854682 ) ) ;
#22300 = CARTESIAN_POINT ( 'NONE',  ( -3.044812012440131443, 216.5253028482142952, 49.10113791807857808 ) ) ;
#22301 = DIRECTION ( 'NONE',  ( 1.000000000000000000, 0.000000000000000000, 0.000000000000000000 ) ) ;
#22302 = DIRECTION ( 'NONE',  ( -0.000000000000000000, -0.000000000000000000, 1.000000000000000000 ) ) ;
#22303 = CARTESIAN_POINT ( 'NONE',  ( 9.736236675708031640, 199.9851607334238963, 16.29886208192143471 ) ) ;
#22304 = CARTESIAN_POINT ( 'NONE',  ( 8.118202686958138514, 201.1607312380088501, 19.29886208192143471 ) ) ;
#22305 = CARTESIAN_POINT ( 'NONE',  ( 65.49999999453761745, 139.7537977485451393, -4.138211985947621020E-15 ) ) ;
#22306 = ORIENTED_EDGE ( 'NONE', *, *, #30591, .F. ) ;
#22307 = CARTESIAN_POINT ( 'NONE',  ( 7.456977232089302632, 217.1783343296989131, 58.55113791807858092 ) ) ;
#22308 = CARTESIAN_POINT ( 'NONE',  ( 2.517493886308900919, 214.5937144450984420, 67.40113791807856103 ) ) ;
#22309 = CARTESIAN_POINT ( 'NONE',  ( -6.139770520408224463, 198.4640165459539389, 32.04886208192143471 ) ) ;
#22310 = CARTESIAN_POINT ( 'NONE',  ( 5.979512004945807924, -4.053280633787082365, -0.5609245978742287697 ) ) ;
#22311 = ORIENTED_EDGE ( 'NONE', *, *, #20104, .F. ) ;
#22312 = CARTESIAN_POINT ( 'NONE',  ( -10.01549611932653860, 203.7984951890123284, 90.35113791807857808 ) ) ;
#22313 = VERTEX_POINT ( 'NONE', #26617 ) ;
#22314 = CARTESIAN_POINT ( 'NONE',  ( 16.00000000000000000, 0.000000000000000000, -1.400415076419418092 ) ) ;
#22315 = DIRECTION ( 'NONE',  ( 1.000000000000000000, 0.000000000000000000, 0.000000000000000000 ) ) ;
#22316 = ORIENTED_EDGE ( 'NONE', *, *, #7714, .T. ) ;
#22317 = CARTESIAN_POINT ( 'NONE',  ( -0.05014649552807731031, 198.5883022060938572, 32.75113791807856956 ) ) ;
#22318 = LINE ( 'NONE', #24715, #13986 ) ;
#22319 = CARTESIAN_POINT ( 'NONE',  ( 10.01549611932659545, 203.7984951890123853, 16.14886208192143613 ) ) ;
#22320 = CARTESIAN_POINT ( 'NONE',  ( 53.77499999726881441, 169.8198683612136222, -4.815267126137197984 ) ) ;
#22321 = ORIENTED_EDGE ( 'NONE', *, *, #25562, .T. ) ;
#22322 = CARTESIAN_POINT ( 'NONE',  ( 0.05014649552807626948, 215.4116977939061144, 52.25113791807857666 ) ) ;
#22323 = CARTESIAN_POINT ( 'NONE',  ( 66.91132485994280898, 146.1832212156128890, 12.13525491562421976 ) ) ;
#22324 = DIRECTION ( 'NONE',  ( -1.000000000000000000, 0.000000000000000000, 0.000000000000000000 ) ) ;
#22325 = CARTESIAN_POINT ( 'NONE',  ( -10.01549611932659722, 210.2015048109875011, 89.64886208192143613 ) ) ;
#22326 = CARTESIAN_POINT ( 'NONE',  ( 56.87499999726880162, 138.6155565068815463, -3.929120461958505118E-15 ) ) ;
#22327 = CARTESIAN_POINT ( 'NONE',  ( 10.01549611932653860, 210.2015048109876716, 31.85113791807857453 ) ) ;
#22328 = CARTESIAN_POINT ( 'NONE',  ( -6.837824896291515131, -3.947820044545435447, -6.564402953523717166 ) ) ;
#22329 = CARTESIAN_POINT ( 'NONE',  ( -10.01549611932653860, 203.7984951890123284, 15.35113791807856565 ) ) ;
#22330 = CARTESIAN_POINT ( 'NONE',  ( 121.5000000000000000, 48.99999999999998579, 7.263162560269298651E-13 ) ) ;
#22331 = CIRCLE ( 'NONE', #12563, 27.50000000000000355 ) ;
#22332 = CARTESIAN_POINT ( 'NONE',  ( 81.10000000000000853, 168.7903194862797420, 4.480746418436729606 ) ) ;
#22333 = FILL_AREA_STYLE_COLOUR ( '', #32839 ) ;
#22334 = CARTESIAN_POINT ( 'NONE',  ( 2.927447417349540615, -2.351289329882181534, -0.1217565302851272152 ) ) ;
#22335 = CARTESIAN_POINT ( 'NONE',  ( 6.139770520408368348, 198.4640165459539674, 101.4511379180785866 ) ) ;
#22336 = LINE ( 'NONE', #14835, #27103 ) ;
#22337 = CARTESIAN_POINT ( 'NONE',  ( 41.97499999726881015, 169.8198683612136222, 4.815267126137181997 ) ) ;
#22338 = CARTESIAN_POINT ( 'NONE',  ( -8.118202686958039038, 201.1607312380087080, 45.20113791807857240 ) ) ;
#22339 = CARTESIAN_POINT ( 'NONE',  ( 86.22499999726882436, 149.9369285172503510, 15.58253174999999580 ) ) ;
#22340 = DIRECTION ( 'NONE',  ( -0.000000000000000000, -0.000000000000000000, 1.000000000000000000 ) ) ;
#22341 = CARTESIAN_POINT ( 'NONE',  ( 5.000000000000000000, 2.342598717236900718, -4.057500000000001883 ) ) ;
#22342 = CARTESIAN_POINT ( 'NONE',  ( 47.59999999453763309, 141.2096805137202580, -4.480746418436742040 ) ) ;
#22343 = ORIENTED_EDGE ( 'NONE', *, *, #3635, .F. ) ;
#22344 = CARTESIAN_POINT ( 'NONE',  ( -9.680171189290831535, 214.0920067884431148, 21.80113791807856671 ) ) ;
#22345 = CARTESIAN_POINT ( 'NONE',  ( -11.00000000000000355, 207.1715494402557738, 103.3438596442687327 ) ) ;
#22346 = CYLINDRICAL_SURFACE ( 'NONE', #31903, 19.99999999999998934 ) ;
#22347 = VERTEX_POINT ( 'NONE', #8567 ) ;
#22348 = CARTESIAN_POINT ( 'NONE',  ( -9.680171189290716072, 199.9079932115567146, 44.19886208192143329 ) ) ;
#22349 = DIRECTION ( 'NONE',  ( 0.000000000000000000, -1.000000000000000000, 0.000000000000000000 ) ) ;
#22350 = CARTESIAN_POINT ( 'NONE',  ( 9.984503880673470277, 203.7031108863295401, 65.15113791807856103 ) ) ;
#22351 = CARTESIAN_POINT ( 'NONE',  ( -4.984841277089891776, 213.7757310962905990, 26.94886208192142973 ) ) ;
#22352 = FACE_OUTER_BOUND ( 'NONE', #3004, .T. ) ;
#22353 = AXIS2_PLACEMENT_3D ( 'NONE', #5241, #17686, #20919 ) ;
#22354 = ORIENTED_EDGE ( 'NONE', *, *, #8139, .T. ) ;
#22355 = CARTESIAN_POINT ( 'NONE',  ( 6.444103211791042618, 202.2591342207267644, 8.301137918078564937 ) ) ;
#22356 = FACE_OUTER_BOUND ( 'NONE', #34, .T. ) ;
#22357 = CARTESIAN_POINT ( 'NONE',  ( -7.456977232089471386, 217.1783343296987709, 89.94886208192144750 ) ) ;
#22358 = CARTESIAN_POINT ( 'NONE',  ( -52.50000000000002132, 120.3589838486224437, 20.00000000000000000 ) ) ;
#22359 = ORIENTED_EDGE ( 'NONE', *, *, #8963, .T. ) ;
#22360 = CARTESIAN_POINT ( 'NONE',  ( 37.62499999726880162, 171.3844434931184253, -7.942151717890132712E-15 ) ) ;
#22361 = FACE_OUTER_BOUND ( 'NONE', #22608, .T. ) ;
#22362 = CYLINDRICAL_SURFACE ( 'NONE', #1839, 8.000000000000000000 ) ;
#22363 = CARTESIAN_POINT ( 'NONE',  ( 0.05014649552828275708, 196.4853777576173002, 58.74886208192141623 ) ) ;
#22364 = CARTESIAN_POINT ( 'NONE',  ( 39.77499999726881441, 169.8198683612136222, -4.815267126137197984 ) ) ;
#22365 = CARTESIAN_POINT ( 'NONE',  ( 103.3032345859876102, 155.0000000000000000, -31.00000000000000000 ) ) ;
#22366 = CARTESIAN_POINT ( 'NONE',  ( -3.044812012440131443, 216.5253028482142952, 1.101137918078565869 ) ) ;
#22367 = DIRECTION ( 'NONE',  ( 0.000000000000000000, -0.7071067811865540120, -0.7071067811865411334 ) ) ;
#22368 = EDGE_CURVE ( 'NONE', #29364, #18797, #19122, .T. ) ;
#22369 = CARTESIAN_POINT ( 'NONE',  ( 58.50000000000000000, 155.0000000000000000, -14.50000000000000711 ) ) ;
#22370 = CARTESIAN_POINT ( 'NONE',  ( -27.50000000000000000, -13.28298644054430966, -1.741296657551681948 ) ) ;
#22371 = CARTESIAN_POINT ( 'NONE',  ( -2.426778023690076225, 199.3768101843759553, 85.89886208192143613 ) ) ;
#22372 = FACE_OUTER_BOUND ( 'NONE', #21214, .T. ) ;
#22373 = DIRECTION ( 'NONE',  ( 0.9945218953682777308, 1.280104479604719079E-17, 0.1045284632676113518 ) ) ;
#22374 = CARTESIAN_POINT ( 'NONE',  ( -12.00000000000000711, 206.9523078486584780, 83.49886208192144466 ) ) ;
#22375 = CARTESIAN_POINT ( 'NONE',  ( 63.42499999726881299, 168.2552932293087906, -9.630534252274385310 ) ) ;
#22377 = ORIENTED_EDGE ( 'NONE', *, *, #157, .T. ) ;
#22376 = CARTESIAN_POINT ( 'NONE',  ( -3.044812012440131443, 216.5253028482142952, 25.10113791807856742 ) ) ;
#22378 = FACE_OUTER_BOUND ( 'NONE', #4895, .T. ) ;
#22379 = CIRCLE ( 'NONE', #32172, 27.50000000000000355 ) ;
#22380 = CARTESIAN_POINT ( 'NONE',  ( 85.37499999726881583, 155.0000000000000000, -15.58253175000000823 ) ) ;
#22381 = B_SPLINE_CURVE_WITH_KNOTS ( 'NONE', 3,
 ( #9685, #22296, #29967, #30135, #24850, #24689, #19739, #17519, #1513, #27237, #11910, #22122, #20079, #32677, #6625, #30474, #9343, #12071, #25025, #19901 ),
 .UNSPECIFIED., .F., .F.,
 ( 4, 2, 2, 2, 2, 2, 2, 2, 2, 4 ),
 ( 0.000000000000000000, 0.002030509116170894305, 0.003045763674256341241, 0.004061018232341788610, 0.006091527348512682481, 0.007106781906598130284, 0.008122036464683577220, 0.01218305469702552456, 0.01421356381319653639, 0.01624407292936754996 ),
 .UNSPECIFIED. ) ;
#22382 = CARTESIAN_POINT ( 'NONE',  ( -0.05014649552807705357, 194.3824533091408000, 83.75113791807856956 ) ) ;
#22383 = CARTESIAN_POINT ( 'NONE',  ( 0.000000000000000000, 7.715274834628324392E-16, -6.099999999999999645 ) ) ;
#22384 = VERTEX_POINT ( 'NONE', #3281 ) ;
#22385 = CARTESIAN_POINT ( 'NONE',  ( -12.00000000000000711, 206.9523078486584780, 74.49886208192144466 ) ) ;
#22386 = CARTESIAN_POINT ( 'NONE',  ( -10.01549611932659545, 210.2015048109875011, 74.64886208192142192 ) ) ;
#22387 = CARTESIAN_POINT ( 'NONE',  ( -7.456977232089471386, 217.1783343296987709, 17.94886208192143684 ) ) ;
#22388 = DIRECTION ( 'NONE',  ( 1.000000000000000000, -0.000000000000000000, -0.000000000000000000 ) ) ;
#22389 = CARTESIAN_POINT ( 'NONE',  ( -10.01549611932653860, 203.7984951890123284, 36.35113791807857098 ) ) ;
#22390 = CARTESIAN_POINT ( 'NONE',  ( -125.0000000000000000, 0.000000000000000000, -20.00000000000000000 ) ) ;
#22391 = CARTESIAN_POINT ( 'NONE',  ( -10.01549611932659722, 210.2015048109875011, 98.64886208192143613 ) ) ;
#22392 = PLANE ( 'NONE',  #1290 ) ;
#22393 = ORIENTED_EDGE ( 'NONE', *, *, #29682, .F. ) ;
#22394 = DIRECTION ( 'NONE',  ( 0.000000000000000000, 0.000000000000000000, -1.000000000000000000 ) ) ;
#22395 = CARTESIAN_POINT ( 'NONE',  ( 8.015496119326595448, 204.4483345814782638, 67.14886208192143613 ) ) ;
#22396 = ORIENTED_EDGE ( 'NONE', *, *, #20375, .T. ) ;
#22397 = CARTESIAN_POINT ( 'NONE',  ( 81.92499999726882720, 164.1591823560292198, 12.60653300113718167 ) ) ;
#22398 = VERTEX_POINT ( 'NONE', #894 ) ;
#22399 = LINE ( 'NONE', #30074, #18331 ) ;
#22400 = CIRCLE ( 'NONE', #32736, 100.0000000000000000 ) ;
#22401 = CARTESIAN_POINT ( 'NONE',  ( 77.72499999726881015, 169.8198683612136222, 4.815267126137181997 ) ) ;
#22402 = CARTESIAN_POINT ( 'NONE',  ( -7.499999999999999112, 0.3744244963005040061, 1.590163186312071526E-15 ) ) ;
#22403 = CARTESIAN_POINT ( 'NONE',  ( -8.015496119326531499, 204.4483345814780364, 81.35113791807857808 ) ) ;
#22404 = CARTESIAN_POINT ( 'NONE',  ( 74.78867513459483973, 155.0000000000000000, -15.00000000000002487 ) ) ;
#22405 = ADVANCED_FACE ( 'NONE', ( #21680 ), #12391, .F. ) ;
#22407 = VECTOR ( 'NONE', #30208, 1000.000000000000000 ) ;
#22406 =( LENGTH_UNIT ( ) NAMED_UNIT ( * ) SI_UNIT ( .MILLI., .METRE. ) );
#22408 = CARTESIAN_POINT ( 'NONE',  ( 41.80000000000000426, 142.6655632788954620, 8.961492836873471646 ) ) ;
#22409 = CARTESIAN_POINT ( 'NONE',  ( -8.000000000000008882, 206.9523078486584780, 56.49886208192145176 ) ) ;
#22410 = EDGE_CURVE ( 'NONE', #5483, #258, #6959, .T. ) ;
#22411 = EDGE_CURVE ( 'NONE', #25547, #24712, #14681, .T. ) ;
#22412 = CARTESIAN_POINT ( 'NONE',  ( 0.000000000000000000, 0.000000000000000000, 20.00000000000000000 ) ) ;
#22413 = CARTESIAN_POINT ( 'NONE',  ( 77.88867513459483405, 150.1262045565060816, 14.99999999999978328 ) ) ;
#22414 = CARTESIAN_POINT ( 'NONE',  ( 32.50000000000000000, 155.0000000000000000, -6.938893903907228378E-15 ) ) ;
#22415 = CARTESIAN_POINT ( 'NONE',  ( 53.42499999726880588, 168.2552932293087906, -9.630534252274387086 ) ) ;
#22416 = CARTESIAN_POINT ( 'NONE',  ( 62.97499999726881015, 140.1801316387863778, -4.815267126137194431 ) ) ;
#22417 = CARTESIAN_POINT ( 'NONE',  ( 12.00000000000000711, 206.9523078486586485, 62.00113791807856956 ) ) ;
#22418 = DIRECTION ( 'NONE',  ( 0.8191520442889907994, 0.000000000000000000, 0.5735764363510474917 ) ) ;
#22419 = CARTESIAN_POINT ( 'NONE',  ( -12.01549611932652972, 203.1486557965464499, 0.3511379180785654808 ) ) ;
#22420 = CARTESIAN_POINT ( 'NONE',  ( 3.044812012440130555, 197.4746971517856764, 74.60113791807856387 ) ) ;
#22421 = CARTESIAN_POINT ( 'NONE',  ( -7.375838497908014268, 196.7627149292498530, 38.04886208192144181 ) ) ;
#22422 = AXIS2_PLACEMENT_3D ( 'NONE', #4441, #14830, #17052 ) ;
#22423 = CARTESIAN_POINT ( 'NONE',  ( -6.139770520408224463, 198.4640165459539105, 44.04886208192143471 ) ) ;
#22424 = CARTESIAN_POINT ( 'NONE',  ( -65.20000000000000284, -7.347880794884118356E-15, -19.30000000000003979 ) ) ;
#22425 = CARTESIAN_POINT ( 'NONE',  ( 9.736236675707914401, 214.0148392665762458, 91.70113791807857240 ) ) ;
#22426 = CARTESIAN_POINT ( 'NONE',  ( 8.118202686958039038, 212.8392687619912635, 1.701137918078565736 ) ) ;
#22427 = EDGE_CURVE ( 'NONE', #15312, #32873, #32435, .T. ) ;
#22428 = CARTESIAN_POINT ( 'NONE',  ( 8.118202686958138514, 201.1607312380088501, 55.29886208192144181 ) ) ;
#22429 = LINE ( 'NONE', #16814, #11795 ) ;
#22430 = EDGE_LOOP ( 'NONE', ( #5968, #2384, #6014, #12257 ) ) ;
#22431 = CARTESIAN_POINT ( 'NONE',  ( -7.456977232089471386, 217.1783343296987709, 71.94886208192144750 ) ) ;
#22432 = ORIENTED_EDGE ( 'NONE', *, *, #27883, .T. ) ;
#22433 = CARTESIAN_POINT ( 'NONE',  ( 69.37499999726881583, 155.0000000000000000, -15.58253175000000823 ) ) ;
#22434 = CARTESIAN_POINT ( 'NONE',  ( -2.426778023690076225, 199.3768101843759553, 40.89886208192144323 ) ) ;
#22435 = ADVANCED_FACE ( 'NONE', ( #24231 ), #32230, .F. ) ;
#22436 = VECTOR ( 'NONE', #26005, 1000.000000000000000 ) ;
#22437 = ORIENTED_EDGE ( 'NONE', *, *, #18761, .T. ) ;
#22438 = CARTESIAN_POINT ( 'NONE',  ( 86.37499999726881583, 155.0000000000000000, 15.58253174999999402 ) ) ;
#22439 = CARTESIAN_POINT ( 'NONE',  ( -10.39117206796836079, 0.000000000000000000, -8.499999999999998224 ) ) ;
#22440 = LINE ( 'NONE', #17336, #13229 ) ;
#22441 = CARTESIAN_POINT ( 'NONE',  ( -6.500168698208129925, 202.3363017425936050, 57.20113791807857240 ) ) ;
#22442 = LINE ( 'NONE', #9165, #5834 ) ;
#22443 = EDGE_CURVE ( 'NONE', #19467, #17270, #3117, .T. ) ;
#22444 = CARTESIAN_POINT ( 'NONE',  ( 3.135527875058981895, 197.5041725223112792, 43.59886208192143897 ) ) ;
#22445 = VERTEX_POINT ( 'NONE', #1230 ) ;
#22446 = DIRECTION ( 'NONE',  ( -1.000000000000000000, 0.000000000000000000, 0.000000000000000000 ) ) ;
#22447 = DIRECTION ( 'NONE',  ( 0.000000000000000000, 0.000000000000000000, -1.000000000000000000 ) ) ;
#22448 = DIRECTION ( 'NONE',  ( 0.000000000000000000, 0.000000000000000000, 1.000000000000000000 ) ) ;
#22449 = CARTESIAN_POINT ( 'NONE',  ( -6.444103211790928043, 202.2591342207265939, 26.19886208192144039 ) ) ;
#22450 = CARTESIAN_POINT ( 'NONE',  ( 8.118202686958039038, 212.8392687619912635, 58.70113791807857240 ) ) ;
#22451 = CARTESIAN_POINT ( 'NONE',  ( 6.220909254589536808, 215.4770327129947702, 46.55113791807856671 ) ) ;
#22452 = APPLICATION_CONTEXT ( 'automotive_design' ) ;
#22453 = DIRECTION ( 'NONE',  ( 0.000000000000000000, 0.000000000000000000, 1.000000000000000000 ) ) ;
#22454 = CARTESIAN_POINT ( 'NONE',  ( -8.118202686958039038, 201.1607312380087080, 18.20113791807856884 ) ) ;
#22455 = CARTESIAN_POINT ( 'NONE',  ( -4.984841277089726574, 200.2242689037092305, 6.051137918078566713 ) ) ;
#22456 = AXIS2_PLACEMENT_3D ( 'NONE', #25650, #25826, #7939 ) ;
#22457 = CARTESIAN_POINT ( 'NONE',  ( 45.02499999726880731, 149.9369285172503510, -15.58253175000000823 ) ) ;
#22458 = CARTESIAN_POINT ( 'NONE',  ( -5.979512004945809700, 4.053280633787070819, -0.5609245978742248839 ) ) ;
#22459 = CARTESIAN_POINT ( 'NONE',  ( 33.42499999726881299, 168.2552932293087906, -9.630534252274387086 ) ) ;
#22460 = CARTESIAN_POINT ( 'NONE',  ( -3.662846001190052991, 218.4274158808045740, 31.10113791807856742 ) ) ;
#22461 = DIRECTION ( 'NONE',  ( -1.000000000000000000, 0.000000000000000000, 0.000000000000000000 ) ) ;
#22462 = VECTOR ( 'NONE', #29184, 1000.000000000000000 ) ;
#22463 = EDGE_CURVE ( 'NONE', #26026, #20653, #15534, .T. ) ;
#22464 = CARTESIAN_POINT ( 'NONE',  ( -8.118202686958039038, 201.1607312380087080, 75.20113791807857240 ) ) ;
#22465 = CARTESIAN_POINT ( 'NONE',  ( 3.044812012440130555, 197.4746971517856764, 44.60113791807857098 ) ) ;
#22466 = AXIS2_PLACEMENT_3D ( 'NONE', #26021, #22027, #14191 ) ;
#22467 = CARTESIAN_POINT ( 'NONE',  ( 6.288404560131952259, 5.029641972278931839, -0.4504974108211943773 ) ) ;
#22468 = LINE ( 'NONE', #14460, #10883 ) ;
#22469 = CARTESIAN_POINT ( 'NONE',  ( 3.662846001189864698, 218.4274158808046593, 18.39886208192143613 ) ) ;
#22470 = CARTESIAN_POINT ( 'NONE',  ( 8.062137200540822946, 212.9164362838583315, 15.69886208192143506 ) ) ;
#22471 = CARTESIAN_POINT ( 'NONE',  ( 64.49999999453764588, 170.2462022514548323, -7.872454543227099337E-15 ) ) ;
#22472 = ORIENTED_EDGE ( 'NONE', *, *, #23457, .T. ) ;
#22473 = CARTESIAN_POINT ( 'NONE',  ( 7.375838497908181246, 196.7627149292499666, 53.45113791807857240 ) ) ;
#22474 = CARTESIAN_POINT ( 'NONE',  ( -0.05014649552807731031, 198.5883022060938572, 71.75113791807856956 ) ) ;
#22475 = ADVANCED_FACE ( 'NONE', ( #6684 ), #22346, .T. ) ;
#22476 = CARTESIAN_POINT ( 'NONE',  ( -3.135527875058982783, 216.4958274776886924, 30.09886208192143897 ) ) ;
#22477 = CARTESIAN_POINT ( 'NONE',  ( 91.60208470531341618, 155.0000000000000000, 0.000000000000000000 ) ) ;
#22478 = ORIENTED_EDGE ( 'NONE', *, *, #9801, .F. ) ;
#22479 = AXIS2_PLACEMENT_3D ( 'NONE', #27518, #22071, #27689 ) ;
#22480 = ORIENTED_EDGE ( 'NONE', *, *, #9577, .T. ) ;
#22481 = ADVANCED_FACE ( 'NONE', ( #24573 ), #4293, .T. ) ;
#22482 = ORIENTED_EDGE ( 'NONE', *, *, #26207, .F. ) ;
#22483 = PRODUCT ( 'socket head cap screw_iso_ISO 4762 M10 x 90 - 32N', 'socket head cap screw_iso_ISO 4762 M10 x 90 - 32N', '', ( #25568 ) ) ;
#22484 = CARTESIAN_POINT ( 'NONE',  ( 58.58867513459482268, 146.1832212156128890, -12.13525491562423042 ) ) ;
#22485 = CARTESIAN_POINT ( 'NONE',  ( 99.99999999999998579, 0.000000000000000000, 0.000000000000000000 ) ) ;
#22486 = VERTEX_POINT ( 'NONE', #29859 ) ;
#22487 = AXIS2_PLACEMENT_3D ( 'NONE', #9427, #15041, #17430 ) ;
#22488 =( BOUNDED_CURVE ( )  B_SPLINE_CURVE ( 2, ( #3095, #549, #708, #11270, #29329, #29488, #29662, #29156, #13485, #21489, #6311 ),
 .UNSPECIFIED., .F., .T. ) 
 B_SPLINE_CURVE_WITH_KNOTS ( ( 3, 2, 2, 2, 2, 3 ),
 ( 0.4642857142857141906, 0.4678571428571428603, 0.4714285714285714191, 0.4749999999999999223, 0.4785714285714284810, 0.4821428571428570398 ),
 .UNSPECIFIED. ) 
 CURVE ( )  GEOMETRIC_REPRESENTATION_ITEM ( )  RATIONAL_B_SPLINE_CURVE ( ( 1.000000000000000000, 0.9510565162951534202, 1.000000000000000000, 0.9510565162951534202, 1.000000000000000000, 0.9510565162951534202, 1.000000000000000000, 0.9510565162951534202, 1.000000000000000000, 0.9510565162951541973, 0.9999999999999992228 ) ) 
 REPRESENTATION_ITEM ( '' )  );
#22489 = CARTESIAN_POINT ( 'NONE',  ( 6.500168698208129925, 211.6636982574063381, 28.70113791807857240 ) ) ;
#22490 = VECTOR ( 'NONE', #7921, 1000.000000000000000 ) ;
#22491 = CARTESIAN_POINT ( 'NONE',  ( -5.007715329123872641E-16, -8.660254037844399733, -10.00000000000000000 ) ) ;
#22492 = CARTESIAN_POINT ( 'NONE',  ( 9.984503880673420539, 210.2968891136705167, 12.84886208192143187 ) ) ;
#22493 = AXIS2_PLACEMENT_3D ( 'NONE', #19456, #25244, #3949 ) ;
#22494 = CARTESIAN_POINT ( 'NONE',  ( 55.87499999726882294, 171.3844434931184253, -7.942151717890134290E-15 ) ) ;
#22495 = VERTEX_POINT ( 'NONE', #7025 ) ;
#22496 = CARTESIAN_POINT ( 'NONE',  ( -8.000000000000008882, 207.0476921513413515, 54.50113791807857666 ) ) ;
#22497 = CARTESIAN_POINT ( 'NONE',  ( 117.5000000000000142, 155.0000000000000000, -6.938893903907228378E-15 ) ) ;
#22498 = CARTESIAN_POINT ( 'NONE',  ( 57.51132485994281041, 146.1832212156128890, -12.13525491562423042 ) ) ;
#22499 = CARTESIAN_POINT ( 'NONE',  ( -8.062137200540822946, 201.0835637161416400, 104.1988620819214475 ) ) ;
#22500 = CARTESIAN_POINT ( 'NONE',  ( 68.17499999726881299, 164.1591823560292198, 12.60653300113718167 ) ) ;
#22501 = CARTESIAN_POINT ( 'NONE',  ( -6.220909254589537696, 198.5229672870051161, 30.05113791807856671 ) ) ;
#22502 = PRESENTATION_STYLE_ASSIGNMENT (( #12111 ) ) ;
#22503 = CARTESIAN_POINT ( 'NONE',  ( 10.01549611932653860, 210.2015048109876716, 13.85113791807856742 ) ) ;
#22504 = CARTESIAN_POINT ( 'NONE',  ( 121.5000000000000000, 229.9533188057749555, 74.95331880577313655 ) ) ;
#22505 = COLOUR_RGB ( '', 0.40784314, 0.44705882, 0.49803922) ;
#22506 = CARTESIAN_POINT ( 'NONE',  ( 82.30000000000001137, 146.4771138417591203, -11.73074641843674470 ) ) ;
#22507 = CARTESIAN_POINT ( 'NONE',  ( -56.00013514549282689, 194.9999915534094725, -0.1669880218061202404 ) ) ;
#22508 = LINE ( 'NONE', #27955, #15310 ) ;
#22509 = CARTESIAN_POINT ( 'NONE',  ( 10.00000000000000711, 206.9523078486586201, 101.0011379180785696 ) ) ;
#22510 = CARTESIAN_POINT ( 'NONE',  ( -52.50000000000002132, -95.00000000000000000, 270.4495957273638282 ) ) ;
#22511 = CARTESIAN_POINT ( 'NONE',  ( 48.37499999726880873, 155.0000000000000000, 15.58253174999999402 ) ) ;
#22512 = CARTESIAN_POINT ( 'NONE',  ( 9.984503880673470277, 203.7031108863295401, 47.15113791807857524 ) ) ;
#22513 = EDGE_CURVE ( 'NONE', #26329, #14311, #4459, .T. ) ;
#22514 = CARTESIAN_POINT ( 'NONE',  ( 82.12499999726881583, 155.0000000000000000, 15.58253174999999402 ) ) ;
#22515 = DIRECTION ( 'NONE',  ( 0.9945218953682719576, 1.280104479605391614E-17, 0.1045284632676662384 ) ) ;
#22516 = DIRECTION ( 'NONE',  ( 0.000000000000000000, 0.000000000000000000, 1.000000000000000000 ) ) ;
#22517 = CONICAL_SURFACE ( 'NONE', #23054, 27.50000000000000355, 1.047197551196595411 ) ;
#22518 = CARTESIAN_POINT ( 'NONE',  ( 48.79999999453762882, 163.5228861582408797, 11.73074641843673049 ) ) ;
#22519 = EDGE_LOOP ( 'NONE', ( #13384, #28528 ) ) ;
#22520 = CARTESIAN_POINT ( 'NONE',  ( -9.680171189290831535, 214.0920067884431148, 27.80113791807857027 ) ) ;
#22521 = EDGE_CURVE ( 'NONE', #24528, #17836, #14180, .T. ) ;
#22522 = VECTOR ( 'NONE', #8858, 1000.000000000000000 ) ;
#22523 = ADVANCED_FACE ( 'NONE', ( #27461 ), #30362, .F. ) ;
#22524 = DIRECTION ( 'NONE',  ( 0.000000000000000000, 0.000000000000000000, 1.000000000000000000 ) ) ;
#22525 = CARTESIAN_POINT ( 'NONE',  ( -8.062137200540822946, 201.0835637161416400, 5.198862081921435063 ) ) ;
#22526 = CARTESIAN_POINT ( 'NONE',  ( 65.91132485994280898, 163.8167787843871110, -12.13525491562423397 ) ) ;
#22527 = ORIENTED_EDGE ( 'NONE', *, *, #8750, .F. ) ;
#22528 = DIRECTION ( 'NONE',  ( -1.000000000000000000, -0.000000000000000000, -0.000000000000000000 ) ) ;
#22529 = CARTESIAN_POINT ( 'NONE',  ( -6.139770520408369237, 215.5359834540460042, 57.95113791807856529 ) ) ;
#22530 = CARTESIAN_POINT ( 'NONE',  ( 2.517493886309087436, 199.4062855549015865, 19.59886208192143897 ) ) ;
#22531 = TOROIDAL_SURFACE ( 'NONE', #5122, 10.12668159690567649, 0.7733184030943209830 ) ;
#22532 = DIRECTION ( 'NONE',  ( -1.000000000000000000, 0.000000000000000000, 0.000000000000000000 ) ) ;
#22533 = ORIENTED_EDGE ( 'NONE', *, *, #20796, .T. ) ;
#22534 = CARTESIAN_POINT ( 'NONE',  ( 2.517493886308900919, 214.5937144450984420, 4.401137918078566358 ) ) ;
#22535 = DIRECTION ( 'NONE',  ( 0.000000000000000000, 1.000000000000000000, 0.000000000000000000 ) ) ;
#22536 = CARTESIAN_POINT ( 'NONE',  ( 9.680171189290716072, 214.0920067884432854, 87.69886208192144750 ) ) ;
#22537 = CARTESIAN_POINT ( 'NONE',  ( 39.97499999726881015, 169.8198683612136222, 4.815267126137181997 ) ) ;
#22538 = ORIENTED_EDGE ( 'NONE', *, *, #27673, .F. ) ;
#22539 = CARTESIAN_POINT ( 'NONE',  ( 46.02499999726880731, 160.0630714827496206, 15.58253174999999402 ) ) ;
#22540 = DIRECTION ( 'NONE',  ( -1.000000000000000000, -0.000000000000000000, -0.000000000000000000 ) ) ;
#22541 = CARTESIAN_POINT ( 'NONE',  ( -3.044812012440131443, 216.5253028482142952, 1.101137918078565869 ) ) ;
#22542 = STYLED_ITEM ( 'NONE', ( #30134 ), #12954 ) ;
#22543 = CARTESIAN_POINT ( 'NONE',  ( 6.220909254589681581, 198.5229672870052582, 70.44886208192144750 ) ) ;
#22544 = CARTESIAN_POINT ( 'NONE',  ( 48.97499999726881725, 140.1801316387863778, -4.815267126137194431 ) ) ;
#22545 = FACE_OUTER_BOUND ( 'NONE', #19878, .T. ) ;
#22546 = CARTESIAN_POINT ( 'NONE',  ( 0.05014649552810505201, 217.5146222423826714, 1.251137918078566003 ) ) ;
#22547 = CARTESIAN_POINT ( 'NONE',  ( 6.499999999999997335, 1.286902272306391870, -0.09436334093186085625 ) ) ;
#22548 = CARTESIAN_POINT ( 'NONE',  ( 59.40000000000000568, 159.7113355953771077, 14.49999999999999289 ) ) ;
#22549 = CARTESIAN_POINT ( 'NONE',  ( 6.220909254589536808, 215.4770327129947702, 91.55113791807858092 ) ) ;
#22550 = LINE ( 'NONE', #9945, #14762 ) ;
#22551 = CARTESIAN_POINT ( 'NONE',  ( 6.444103211790928043, 211.7408657792734061, 81.69886208192144750 ) ) ;
#22552 = CARTESIAN_POINT ( 'NONE',  ( -67.50000000000000000, 0.000000000000000000, 17.00000000000001421 ) ) ;
#22553 = CARTESIAN_POINT ( 'NONE',  ( 5.000000000000000000, 4.685197434473814759, -5.637851296924623057E-15 ) ) ;
#22554 = CARTESIAN_POINT ( 'NONE',  ( -7.456977232089471386, 217.1783343296987709, 83.94886208192144750 ) ) ;
#22555 = CARTESIAN_POINT ( 'NONE',  ( 67.32499999726881867, 164.1591823560292198, -12.60653300113719766 ) ) ;
#22557 = ORIENTED_EDGE ( 'NONE', *, *, #14492, .F. ) ;
#22556 = CARTESIAN_POINT ( 'NONE',  ( 0.05014649552810506589, 217.5146222423826714, 16.25113791807856600 ) ) ;
#22558 = CARTESIAN_POINT ( 'NONE',  ( -4.506125120515189764, 29.15265225409785543, -1.090893241169164529 ) ) ;
#22559 = CARTESIAN_POINT ( 'NONE',  ( 80.87499999726881583, 138.6155565068815463, -3.929120461958505118E-15 ) ) ;
#22560 = CARTESIAN_POINT ( 'NONE',  ( 9.680171189290831535, 199.9079932115568852, 86.30113791807858092 ) ) ;
#22561 = LINE ( 'NONE', #32946, #19202 ) ;
#22562 = VERTEX_POINT ( 'NONE', #27130 ) ;
#22563 = CARTESIAN_POINT ( 'NONE',  ( 7.456977232089471386, 196.8216656703012006, 67.44886208192143329 ) ) ;
#22564 = CARTESIAN_POINT ( 'NONE',  ( 6.139770520408223575, 215.5359834540460611, 75.54886208192142760 ) ) ;
#22565 = CARTESIAN_POINT ( 'NONE',  ( 3.753561863808876797, 195.6020594897209719, 10.59886208192143542 ) ) ;
#22566 = CARTESIAN_POINT ( 'NONE',  ( 32.50000000000000000, 155.0000000000000000, -15.00000000000002487 ) ) ;
#22567 = CARTESIAN_POINT ( 'NONE',  ( -10.01549611932653860, 203.7984951890123284, 30.35113791807856742 ) ) ;
#22568 = CARTESIAN_POINT ( 'NONE',  ( 77.50000000000000000, 155.0000000000000000, -13.50000000000001776 ) ) ;
#22569 = CARTESIAN_POINT ( 'NONE',  ( 6.220909254589681581, 198.5229672870052582, 97.44886208192143329 ) ) ;
#22570 = DIRECTION ( 'NONE',  ( -1.000000000000000000, -0.000000000000000000, -0.000000000000000000 ) ) ;
#22571 = ORIENTED_EDGE ( 'NONE', *, *, #8545, .F. ) ;
#22572 = CARTESIAN_POINT ( 'NONE',  ( -13.75000000000001243, -23.81569860407206107, -18.00000000000000000 ) ) ;
#22573 = CARTESIAN_POINT ( 'NONE',  ( -8.015496119326597224, 209.5516654185217362, 77.64886208192143613 ) ) ;
#22574 = VERTEX_POINT ( 'NONE', #14508 ) ;
#22575 = CARTESIAN_POINT ( 'NONE',  ( 115.4999999999999858, 155.0000000000000000, -112.0000000000000426 ) ) ;
#22576 = VERTEX_POINT ( 'NONE', #24908 ) ;
#22577 = DIRECTION ( 'NONE',  ( 0.000000000000000000, 0.000000000000000000, -1.000000000000000000 ) ) ;
#22578 = CARTESIAN_POINT ( 'NONE',  ( 76.52499999726880731, 140.1801316387863778, 4.815267126137185549 ) ) ;
#22579 = CARTESIAN_POINT ( 'NONE',  ( 32.50000000000000000, 155.0000000000000000, -6.938893903907228378E-15 ) ) ;
#22580 = CARTESIAN_POINT ( 'NONE',  ( -8.015496119326531499, 204.4483345814780364, 78.35113791807857808 ) ) ;
#22581 = CARTESIAN_POINT ( 'NONE',  ( 125.0000000000000000, 25.00000000000004619, 35.00000000000000000 ) ) ;
#22582 = CARTESIAN_POINT ( 'NONE',  ( 44.29999999999999716, 146.4771138417591203, -11.73074641843674470 ) ) ;
#22583 = CARTESIAN_POINT ( 'NONE',  ( 4.903702542908435547, 213.8346818373419751, 57.54886208192142760 ) ) ;
#22584 = CYLINDRICAL_SURFACE ( 'NONE', #28456, 15.00000000000001776 ) ;
#22585 = DIRECTION ( 'NONE',  ( -0.000000000000000000, -0.000000000000000000, 1.000000000000000000 ) ) ;
#22586 = DIRECTION ( 'NONE',  ( -1.000000000000000000, 0.000000000000000000, 0.000000000000000000 ) ) ;
#22587 = CARTESIAN_POINT ( 'NONE',  ( 49.52499999726880731, 169.8198683612136222, -4.815267126137197984 ) ) ;
#22588 = CARTESIAN_POINT ( 'NONE',  ( 61.77499999726881441, 169.8198683612136222, -4.815267126137197984 ) ) ;
#22589 = CARTESIAN_POINT ( 'NONE',  ( 3.753561863808689836, 218.3979405102790565, 55.40113791807858235 ) ) ;
#22590 = CYLINDRICAL_SURFACE ( 'NONE', #5366, 5.250000000000004441 ) ;
#22591 = CARTESIAN_POINT ( 'NONE',  ( 9.736236675707914401, 214.0148392665762458, 1.701137918078565736 ) ) ;
#22592 = CARTESIAN_POINT ( 'NONE',  ( 6.220909254589536808, 215.4770327129947987, 82.55113791807858092 ) ) ;
#22593 = CARTESIAN_POINT ( 'NONE',  ( 3.753561863808876797, 195.6020594897209719, 43.59886208192143897 ) ) ;
#22594 = CARTESIAN_POINT ( 'NONE',  ( -6.220909254589682469, 215.4770327129947134, 47.94886208192143329 ) ) ;
#22595 = CARTESIAN_POINT ( 'NONE',  ( 127.5000000000000000, 261.0000000000000000, 0.000000000000000000 ) ) ;
#22596 = CARTESIAN_POINT ( 'NONE',  ( -3.753561863808691168, 195.6020594897209435, 89.90113791807857524 ) ) ;
#22597 = CARTESIAN_POINT ( 'NONE',  ( -9.984503880673473830, 210.2968891136704315, 3.651137918078565026 ) ) ;
#22598 = CARTESIAN_POINT ( 'NONE',  ( 10.00000000000000711, 207.0476921513415220, 66.99886208192143044 ) ) ;
#22599 = EDGE_CURVE ( 'NONE', #534, #19849, #24820, .T. ) ;
#22600 = FACE_OUTER_BOUND ( 'NONE', #30671, .T. ) ;
#22602 = ORIENTED_EDGE ( 'NONE', *, *, #29527, .F. ) ;
#22601 = B_SPLINE_CURVE_WITH_KNOTS ( 'NONE', 3,
 ( #24133, #11029, #11190, #27022 ),
 .UNSPECIFIED., .F., .F.,
 ( 4, 4 ),
 ( 0.000000000000000000, 0.004600009204204574646 ),
 .UNSPECIFIED. ) ;
#22603 = CARTESIAN_POINT ( 'NONE',  ( 3.662846001189864698, 218.4274158808046593, 75.39886208192143613 ) ) ;
#22604 = VERTEX_POINT ( 'NONE', #1730 ) ;
#22605 = CARTESIAN_POINT ( 'NONE',  ( 75.17499999726881299, 145.8408176439707802, -12.60653300113719588 ) ) ;
#22606 = CARTESIAN_POINT ( 'NONE',  ( -8.015496119326597224, 209.5516654185217362, 50.64886208192145034 ) ) ;
#22607 = EDGE_CURVE ( 'NONE', #9574, #13603, #11848, .T. ) ;
#22608 = EDGE_LOOP ( 'NONE', ( #9717, #14140, #29032, #1994 ) ) ;
#22609 = CARTESIAN_POINT ( 'NONE',  ( 84.37499999726881583, 155.0000000000000000, 15.58253174999999402 ) ) ;
#22610 = DIRECTION ( 'NONE',  ( 0.000000000000000000, 0.000000000000000000, -1.000000000000000000 ) ) ;
#22611 = DIRECTION ( 'NONE',  ( -1.000000000000000000, 0.000000000000000000, 0.000000000000000000 ) ) ;
#22612 = CARTESIAN_POINT ( 'NONE',  ( 55.92499999726881299, 164.1591823560292198, 12.60653300113718167 ) ) ;
#22613 = DIRECTION ( 'NONE',  ( 0.000000000000000000, 0.000000000000000000, -1.000000000000000000 ) ) ;
#22614 = CARTESIAN_POINT ( 'NONE',  ( 8.062137200540822946, 212.9164362838583315, 42.69886208192143329 ) ) ;
#22615 = ORIENTED_EDGE ( 'NONE', *, *, #22678, .F. ) ;
#22616 = FACE_OUTER_BOUND ( 'NONE', #8216, .T. ) ;
#22617 = CARTESIAN_POINT ( 'NONE',  ( 4.574783636564889733, -5.228990388888015595, -6.171384342982775273 ) ) ;
#22618 = DIRECTION ( 'NONE',  ( 1.000000000000000000, 0.000000000000000000, 0.000000000000000000 ) ) ;
#22619 = CARTESIAN_POINT ( 'NONE',  ( -8.015496119326597224, 209.5516654185217362, 26.64886208192143968 ) ) ;
#22620 = CARTESIAN_POINT ( 'NONE',  ( 6.220909254589536808, 215.4770327129947702, 58.55113791807858092 ) ) ;
#22621 = CARTESIAN_POINT ( 'NONE',  ( -10.00000000000000711, 207.0476921513413515, 42.50113791807856956 ) ) ;
#22622 = CARTESIAN_POINT ( 'NONE',  ( 3.044812012440130555, 197.4746971517856764, 20.60113791807856742 ) ) ;
#22623 = CARTESIAN_POINT ( 'NONE',  ( 2.517493886308900919, 214.5937144450984420, 7.401137918078566358 ) ) ;
#22624 = CARTESIAN_POINT ( 'NONE',  ( 49.62499999726880873, 171.3844434931184253, -7.942151717890132712E-15 ) ) ;
#22625 = LINE ( 'NONE', #33013, #6211 ) ;
#22626 = CARTESIAN_POINT ( 'NONE',  ( 60.00000000000000000, 7.347880794884118356E-15, -35.00000000000000000 ) ) ;
#22627 = CARTESIAN_POINT ( 'NONE',  ( -0.05014649552807705357, 194.3824533091408000, 29.75113791807856956 ) ) ;
#22628 = CARTESIAN_POINT ( 'NONE',  ( 32.50000000000000000, 155.0000000000000000, -15.00000000000002487 ) ) ;
#22629 = ADVANCED_FACE ( 'NONE', ( #6848 ), #27795, .T. ) ;
#22630 =( BOUNDED_CURVE ( )  B_SPLINE_CURVE ( 3, ( #1644, #12717, #32983, #22424 ),
 .UNSPECIFIED., .F., .F. ) 
 B_SPLINE_CURVE_WITH_KNOTS ( ( 4, 4 ),
 ( 2.616713720088120532, 3.141592653589793116 ),
 .UNSPECIFIED. ) 
 CURVE ( )  GEOMETRIC_REPRESENTATION_ITEM ( )  RATIONAL_B_SPLINE_CURVE ( ( 1.000000000000000000, 0.9771733092046011038, 0.9771733092046011038, 1.000000000000000000 ) ) 
 REPRESENTATION_ITEM ( '' )  );
#22631 = CARTESIAN_POINT ( 'NONE',  ( 0.05014649552810505201, 217.5146222423826714, 79.25113791807856956 ) ) ;
#22632 = CARTESIAN_POINT ( 'NONE',  ( 6.220909254589536808, 215.4770327129947987, 46.55113791807856671 ) ) ;
#22633 = UNCERTAINTY_MEASURE_WITH_UNIT (LENGTH_MEASURE( 1.000000000000000082E-05 ), #506, 'distance_accuracy_value', 'NONE');
#22634 = CARTESIAN_POINT ( 'NONE',  ( 4.250000000000000000, 0.000000000000000000, -10.00000000000000000 ) ) ;
#22635 = LINE ( 'NONE', #4587, #16845 ) ;
#22636 = CARTESIAN_POINT ( 'NONE',  ( -9.680171189290716072, 199.9079932115567146, 14.19886208192143684 ) ) ;
#22637 = CARTESIAN_POINT ( 'NONE',  ( -8.062137200540822946, 201.0835637161416400, 17.19886208192143684 ) ) ;
#22638 = CARTESIAN_POINT ( 'NONE',  ( 72.99999999453763166, 155.0000000000000000, 14.49999999999999467 ) ) ;
#22639 = ORIENTED_EDGE ( 'NONE', *, *, #16373, .F. ) ;
#22640 = CARTESIAN_POINT ( 'NONE',  ( -9.680171189290831535, 214.0920067884431148, 57.80113791807857382 ) ) ;
#22641 = CARTESIAN_POINT ( 'NONE',  ( -0.05014649552807731031, 198.5883022060938572, 83.75113791807856956 ) ) ;
#22642 = CARTESIAN_POINT ( 'NONE',  ( -3.135527875058982783, 216.4958274776886924, 45.09886208192143897 ) ) ;
#22643 = EDGE_CURVE ( 'NONE', #7575, #19301, #30192, .T. ) ;
#22644 = AXIS2_PLACEMENT_3D ( 'NONE', #22041, #17266, #27655 ) ;
#22645 = DIRECTION ( 'NONE',  ( -1.000000000000000000, 0.000000000000000000, 0.000000000000000000 ) ) ;
#22646 = ORIENTED_EDGE ( 'NONE', *, *, #15535, .F. ) ;
#22647 = CLOSED_SHELL ( 'NONE', ( #21045, #31754, #25134, #31438, #24360, #21375, #10190, #18746, #33131 ) ) ;
#22648 = ORIENTED_EDGE ( 'NONE', *, *, #30401, .F. ) ;
#22649 = EDGE_LOOP ( 'NONE', ( #10016, #31123, #16861, #6816, #20850, #29474 ) ) ;
#22650 = CIRCLE ( 'NONE', #32980, 27.50000000000000355 ) ;
#22651 = CARTESIAN_POINT ( 'NONE',  ( 58.78867513459481842, 155.0000000000000000, -15.00000000000002487 ) ) ;
#22652 = EDGE_CURVE ( 'NONE', #9110, #6991, #25929, .T. ) ;
#22653 = DIRECTION ( 'NONE',  ( 0.000000000000000000, 0.4999999999999990563, -0.8660254037844391517 ) ) ;
#22654 = ORIENTED_EDGE ( 'NONE', *, *, #25009, .F. ) ;
#22655 = CARTESIAN_POINT ( 'NONE',  ( -2.426778023690262742, 214.6231898156240163, 34.10113791807857098 ) ) ;
#22656 = DIRECTION ( 'NONE',  ( 1.000000000000000000, 0.000000000000000000, 0.000000000000000000 ) ) ;
#22657 = CARTESIAN_POINT ( 'NONE',  ( -10.00000000000000711, 206.9523078486584495, 14.49886208192143577 ) ) ;
#22658 = CARTESIAN_POINT ( 'NONE',  ( 54.57499999726881157, 145.8408176439707802, 12.60653300113718345 ) ) ;
#22659 = VERTEX_POINT ( 'NONE', #9748 ) ;
#22660 = CARTESIAN_POINT ( 'NONE',  ( 0.05014649552807626948, 215.4116977939061144, 49.25113791807856956 ) ) ;
#22661 = DIRECTION ( 'NONE',  ( -1.000000000000000000, 0.000000000000000000, 0.000000000000000000 ) ) ;
#22662 = FILL_AREA_STYLE_COLOUR ( '', #21431 ) ;
#22663 = DIRECTION ( 'NONE',  ( 0.000000000000000000, 0.000000000000000000, -1.000000000000000000 ) ) ;
#22664 = CARTESIAN_POINT ( 'NONE',  ( -3.044812012439970683, 197.4746971517856196, 97.89886208192145034 ) ) ;
#22665 = CARTESIAN_POINT ( 'NONE',  ( 65.77499999726880731, 169.8198683612136222, -4.815267126137197984 ) ) ;
#22666 = CARTESIAN_POINT ( 'NONE',  ( 8.062137200540920645, 201.0835637161417822, 32.30113791807857382 ) ) ;
#22667 = CARTESIAN_POINT ( 'NONE',  ( 127.5000000000000000, 80.04668119422552763, -74.95331880577366235 ) ) ;
#22668 = EDGE_CURVE ( 'NONE', #18640, #12511, #18845, .T. ) ;
#22669 = CARTESIAN_POINT ( 'NONE',  ( -10.00000000000000711, 207.0476921513413515, 15.50113791807856600 ) ) ;
#22670 = CIRCLE ( 'NONE', #4694, 3.500000000000000000 ) ;
#22671 = CARTESIAN_POINT ( 'NONE',  ( 132.3999999999999773, 155.0000000000010800, 106.0000000000000142 ) ) ;
#22672 = CARTESIAN_POINT ( 'NONE',  ( 81.39999999999999147, 159.7113355953771077, 14.49999999999999289 ) ) ;
#22673 = CARTESIAN_POINT ( 'NONE',  ( -4.336808689942017736E-14, -31.75426480542944319, -2.456200930618646971 ) ) ;
#22674 = CARTESIAN_POINT ( 'NONE',  ( -5.357619327558936585E-16, 7.505553499465138501, -6.177802698399433190 ) ) ;
#22675 = CARTESIAN_POINT ( 'NONE',  ( 7.375838497908181246, 196.7627149292499666, 2.451137918078565736 ) ) ;
#22676 = CARTESIAN_POINT ( 'NONE',  ( 48.58867513459482268, 146.1832212156128890, -12.13525491562423042 ) ) ;
#22677 = CARTESIAN_POINT ( 'NONE',  ( 47.87499999726880162, 171.3844434931184253, -7.942151717890132712E-15 ) ) ;
#22678 = EDGE_CURVE ( 'NONE', #10286, #8044, #9918, .T. ) ;
#22679 = CARTESIAN_POINT ( 'NONE',  ( 0.05014649552810505201, 217.5146222423826714, 46.25113791807855534 ) ) ;
#22680 = CIRCLE ( 'NONE', #18356, 40.00000000000000711 ) ;
#22681 = CARTESIAN_POINT ( 'NONE',  ( 82.62499999726881583, 138.6155565068815463, -3.929120461958505118E-15 ) ) ;
#22682 = CARTESIAN_POINT ( 'NONE',  ( 41.71132485994280614, 155.0000000000000000, -15.00000000000002487 ) ) ;
#22683 = DIRECTION ( 'NONE',  ( 0.000000000000000000, 0.000000000000000000, 1.000000000000000000 ) ) ;
#22684 = CARTESIAN_POINT ( 'NONE',  ( 52.99999999453762456, 155.0000000000000000, 14.49999999999999467 ) ) ;
#22685 = ORIENTED_EDGE ( 'NONE', *, *, #16373, .T. ) ;
#22686 = CARTESIAN_POINT ( 'NONE',  ( 12.00000000000000711, 206.9523078486586485, 32.00113791807856956 ) ) ;
#22687 = DIRECTION ( 'NONE',  ( 1.000000000000000000, 0.000000000000000000, 0.000000000000000000 ) ) ;
#22688 = CARTESIAN_POINT ( 'NONE',  ( 6.139770520408223575, 215.5359834540460611, 3.548862081921434708 ) ) ;
#22689 = CARTESIAN_POINT ( 'NONE',  ( -31.74999999999995737, 0.000000000000000000, 6.500000000000000000 ) ) ;
#22690 = EDGE_LOOP ( 'NONE', ( #29312, #8096, #8482, #28365 ) ) ;
#22691 = CARTESIAN_POINT ( 'NONE',  ( 54.75000000000000711, 7.990820364436479461E-15, -35.00000000000000000 ) ) ;
#22692 = CARTESIAN_POINT ( 'NONE',  ( 8.118202686958039038, 212.8392687619912635, 61.70113791807857240 ) ) ;
#22693 = CIRCLE ( 'NONE', #12355, 5.250000000000004441 ) ;
#22694 = ORIENTED_EDGE ( 'NONE', *, *, #27047, .F. ) ;
#22695 = CARTESIAN_POINT ( 'NONE',  ( -8.015496119326597224, 209.5516654185217362, 20.64886208192143613 ) ) ;
#22696 =( GEOMETRIC_REPRESENTATION_CONTEXT ( 3 ) GLOBAL_UNCERTAINTY_ASSIGNED_CONTEXT ( ( #18842 ) ) GLOBAL_UNIT_ASSIGNED_CONTEXT ( ( #10239, #18560, #20946 ) ) REPRESENTATION_CONTEXT ( 'NONE', 'WORKASPACE' ) );
#22697 = DIRECTION ( 'NONE',  ( 0.000000000000000000, 0.000000000000000000, -1.000000000000000000 ) ) ;
#22698 = ORIENTED_EDGE ( 'NONE', *, *, #28326, .F. ) ;
#22699 = CARTESIAN_POINT ( 'NONE',  ( -6.500168698208129925, 202.3363017425936050, 0.2011379180785659582 ) ) ;
#22700 = ADVANCED_FACE ( 'NONE', ( #23375 ), #1438, .F. ) ;
#22701 = EDGE_CURVE ( 'NONE', #33266, #17976, #23027, .T. ) ;
#22702 = DIRECTION ( 'NONE',  ( 0.000000000000000000, 0.000000000000000000, -1.000000000000000000 ) ) ;
#22703 = CARTESIAN_POINT ( 'NONE',  ( -3.753561863808878130, 218.3979405102790281, 90.09886208192143897 ) ) ;
#22704 = CARTESIAN_POINT ( 'NONE',  ( 37.07499999726881157, 141.7447067706911810, -9.630534252274387086 ) ) ;
#22706 = ORIENTED_EDGE ( 'NONE', *, *, #21622, .F. ) ;
#22705 = VECTOR ( 'NONE', #31239, 1000.000000000000000 ) ;
#22707 = CARTESIAN_POINT ( 'NONE',  ( 43.12499999726881583, 155.0000000000000000, -15.58253175000000823 ) ) ;
#22708 = CARTESIAN_POINT ( 'NONE',  ( 38.78867513459481842, 155.0000000000000000, -15.00000000000002487 ) ) ;
#22709 = CARTESIAN_POINT ( 'NONE',  ( 3.044812012440130555, 197.4746971517856764, 2.601137918078566091 ) ) ;
#22710 = CARTESIAN_POINT ( 'NONE',  ( 9.984503880673420539, 210.2968891136705167, 66.84886208192141055 ) ) ;
#22711 = CARTESIAN_POINT ( 'NONE',  ( 44.47499999726879594, 149.9369285172503510, 15.58253174999999580 ) ) ;
#22712 = DIRECTION ( 'NONE',  ( 0.000000000000000000, 0.000000000000000000, -1.000000000000000000 ) ) ;
#22713 = CARTESIAN_POINT ( 'NONE',  ( 10.01549611932653860, 210.2015048109876716, 1.851137918078565203 ) ) ;
#22714 = CARTESIAN_POINT ( 'NONE',  ( 117.5000000000000000, 52.61186241335891367, 27.43481878086798176 ) ) ;
#22715 = EDGE_CURVE ( 'NONE', #1780, #16312, #22102, .T. ) ;
#22716 = CARTESIAN_POINT ( 'NONE',  ( 60.00000000000000000, 139.7537977485451393, -4.138211985947621020E-15 ) ) ;
#22717 = CARTESIAN_POINT ( 'NONE',  ( -9.984503880673473830, 210.2968891136704315, 90.65113791807854682 ) ) ;
#22718 = LINE ( 'NONE', #7217, #26726 ) ;
#22719 = CARTESIAN_POINT ( 'NONE',  ( -3.135527875058821579, 197.5041725223112223, 74.90113791807857524 ) ) ;
#22720 = VECTOR ( 'NONE', #3014, 1000.000000000000000 ) ;
#22721 = CARTESIAN_POINT ( 'NONE',  ( -5.088535779737005882, 5.722386535631696525, -7.491772860716161553 ) ) ;
#22722 = DIRECTION ( 'NONE',  ( 0.5773502691896268413, -0.5773502691896268413, -0.5773502691896235106 ) ) ;
#22723 = EDGE_CURVE ( 'NONE', #3615, #20973, #13284, .T. ) ;
#22724 = CARTESIAN_POINT ( 'NONE',  ( -7.456977232089471386, 217.1783343296987709, 89.94886208192144750 ) ) ;
#22725 = MECHANICAL_DESIGN_GEOMETRIC_PRESENTATION_REPRESENTATION (  '', ( #9655 ), #3116 ) ;
#22726 = CARTESIAN_POINT ( 'NONE',  ( 66.12499999726881583, 155.0000000000000000, 15.58253174999999402 ) ) ;
#22728 = EDGE_LOOP ( 'NONE', ( #18753, #29066, #20052, #17942 ) ) ;
#22727 = CARTESIAN_POINT ( 'NONE',  ( 10.01549611932653860, 210.2015048109876716, 19.85113791807856742 ) ) ;
#22729 = CARTESIAN_POINT ( 'NONE',  ( -18.00000000000000355, 2.204364238465235822E-15, -18.00000000000000000 ) ) ;
#22730 = CARTESIAN_POINT ( 'NONE',  ( 81.47499999726879594, 160.0630714827496206, -15.58253175000000823 ) ) ;
#22731 = CARTESIAN_POINT ( 'NONE',  ( -9.680171189290831535, 214.0920067884431148, 90.80113791807858092 ) ) ;
#22732 = CARTESIAN_POINT ( 'NONE',  ( 72.48867513459484258, 142.2402378747194405, -9.270509831248439525 ) ) ;
#22733 = AXIS2_PLACEMENT_3D ( 'NONE', #22208, #6023, #919 ) ;
#22734 = VERTEX_POINT ( 'NONE', #31208 ) ;
#22735 = CARTESIAN_POINT ( 'NONE',  ( -7.375838497908014268, 196.7627149292498530, 74.04886208192142760 ) ) ;
#22736 = CARTESIAN_POINT ( 'NONE',  ( -10.00000000000000711, 206.9523078486584495, 89.49886208192144466 ) ) ;
#22737 = CARTESIAN_POINT ( 'NONE',  ( -9.736236675708031640, 214.0148392665760753, 11.79886208192143648 ) ) ;
#22738 = CARTESIAN_POINT ( 'NONE',  ( 107.5000000000000000, 155.0000000000000000, -98.00000000000000000 ) ) ;
#22739 = CARTESIAN_POINT ( 'NONE',  ( 8.118202686958039038, 212.8392687619912635, 31.70113791807856884 ) ) ;
#22740 = PLANE ( 'NONE',  #902 ) ;
#22741 = CARTESIAN_POINT ( 'NONE',  ( 10.01549611932659545, 203.7984951890123853, 100.1488620819214077 ) ) ;
#22742 = CARTESIAN_POINT ( 'NONE',  ( 7.500000000000000000, -4.330127018922199866, -10.00000000000000000 ) ) ;
#22743 = VERTEX_POINT ( 'NONE', #12981 ) ;
#22744 = CARTESIAN_POINT ( 'NONE',  ( -67.50000000000000000, 0.000000000000000000, 270.4495957273638282 ) ) ;
#22745 = CARTESIAN_POINT ( 'NONE',  ( -2.426778023690076225, 199.3768101843759553, 76.89886208192143613 ) ) ;
#22746 = AXIS2_PLACEMENT_3D ( 'NONE', #12858, #9622, #12688 ) ;
#22747 = ORIENTED_EDGE ( 'NONE', *, *, #28534, .F. ) ;
#22748 = DIRECTION ( 'NONE',  ( 0.000000000000000000, 0.000000000000000000, -1.000000000000000000 ) ) ;
#22749 = VERTEX_POINT ( 'NONE', #7705 ) ;
#22750 = CARTESIAN_POINT ( 'NONE',  ( 6.523606932381168733, 4.893847819346807348, -7.213065638943126245 ) ) ;
#22751 =( GEOMETRIC_REPRESENTATION_CONTEXT ( 3 ) GLOBAL_UNCERTAINTY_ASSIGNED_CONTEXT ( ( #29072 ) ) GLOBAL_UNIT_ASSIGNED_CONTEXT ( ( #16114, #5725, #16618 ) ) REPRESENTATION_CONTEXT ( 'NONE', 'WORKASPACE' ) );
#22752 = CARTESIAN_POINT ( 'NONE',  ( 73.37499999726881583, 155.0000000000000000, -15.58253175000000823 ) ) ;
#22753 = CARTESIAN_POINT ( 'NONE',  ( 79.82499999726881867, 168.2552932293087906, 9.630534252274372875 ) ) ;
#22754 = CARTESIAN_POINT ( 'NONE',  ( 0.000000000000000000, 0.000000000000000000, -8.499999999999998224 ) ) ;
#22755 = CARTESIAN_POINT ( 'NONE',  ( 8.000000000000008882, 206.9523078486586485, 83.00113791807856956 ) ) ;
#22756 = DIRECTION ( 'NONE',  ( -0.7071067811865331398, 0.000000000000000000, 0.7071067811865620056 ) ) ;
#22757 = CIRCLE ( 'NONE', #14036, 16.00000000000000000 ) ;
#22758 =( LENGTH_UNIT ( ) NAMED_UNIT ( * ) SI_UNIT ( .MILLI., .METRE. ) );
#22759 = CARTESIAN_POINT ( 'NONE',  ( 39.20000000000000284, 167.3344367211045096, 8.961492836873468093 ) ) ;
#22760 = CARTESIAN_POINT ( 'NONE',  ( -2.426778023690076225, 199.3768101843759553, 49.89886208192144323 ) ) ;
#22761 = CARTESIAN_POINT ( 'NONE',  ( 6.837824896291514243, 3.947820044545427454, -6.564402953523716278 ) ) ;
#22762 = DIRECTION ( 'NONE',  ( 0.000000000000000000, 0.000000000000000000, -1.000000000000000000 ) ) ;
#22763 = CARTESIAN_POINT ( 'NONE',  ( -122.3560003530527638, 4.587378538859855581, 35.00001199999999812 ) ) ;
#22764 = CARTESIAN_POINT ( 'NONE',  ( 56.12499999726880873, 155.0000000000000000, 15.58253174999999402 ) ) ;
#22765 = CARTESIAN_POINT ( 'NONE',  ( 65.67499999726881299, 168.2552932293087906, -9.630534252274385310 ) ) ;
#22766 = CARTESIAN_POINT ( 'NONE',  ( 3.662846001190051659, 195.5725841191953691, 56.60113791807857808 ) ) ;
#22767 = CARTESIAN_POINT ( 'NONE',  ( 46.11132485994280472, 169.2658477444273331, -4.635254915624224203 ) ) ;
#22768 = AXIS2_PLACEMENT_3D ( 'NONE', #7608, #10503, #5205 ) ;
#22769 = CARTESIAN_POINT ( 'NONE',  ( -9.680171189290831535, 214.0920067884431148, 3.801137918078565825 ) ) ;
#22770 = CARTESIAN_POINT ( 'NONE',  ( 10.01549611932653860, 210.2015048109876716, 73.85113791807857808 ) ) ;
#22771 = AXIS2_PLACEMENT_3D ( 'NONE', #28940, #8172, #26383 ) ;
#22772 = CARTESIAN_POINT ( 'NONE',  ( -7.375838497908014268, 196.7627149292498530, 47.04886208192144181 ) ) ;
#22773 = CARTESIAN_POINT ( 'NONE',  ( -8.118202686958138514, 212.8392687619910930, 47.79886208192143471 ) ) ;
#22774 = CARTESIAN_POINT ( 'NONE',  ( 0.000000000000000000, 0.000000000000000000, -25.03750572909317285 ) ) ;
#22775 = CARTESIAN_POINT ( 'NONE',  ( -7.456977232089304408, 196.8216656703010301, 87.05113791807856671 ) ) ;
#22776 = CARTESIAN_POINT ( 'NONE',  ( 42.49999999999999289, -72.99999999999998579, -20.00000000000000000 ) ) ;
#22777 = CARTESIAN_POINT ( 'NONE',  ( -6.139770520408369237, 215.5359834540460042, 6.951137918078566180 ) ) ;
#22778 = CARTESIAN_POINT ( 'NONE',  ( 6.139770520408223575, 215.5359834540460611, 72.54886208192144181 ) ) ;
#22779 = PLANE ( 'NONE',  #23809 ) ;
#22780 = CONICAL_SURFACE ( 'NONE', #22210, 32.00000000000002842, 0.1047197551196217685 ) ;
#22781 = EDGE_LOOP ( 'NONE', ( #32989, #19257 ) ) ;
#22782 = CARTESIAN_POINT ( 'NONE',  ( -12.00000000000000711, 206.9523078486584780, 74.49886208192144466 ) ) ;
#22783 = EDGE_LOOP ( 'NONE', ( #22478, #32697, #27982, #16404 ) ) ;
#22784 = CARTESIAN_POINT ( 'NONE',  ( 79.17499999726881299, 145.8408176439707802, -12.60653300113719588 ) ) ;
#22785 = CARTESIAN_POINT ( 'NONE',  ( 2.517493886309087436, 199.4062855549015865, 49.59886208192143897 ) ) ;
#22786 = EDGE_LOOP ( 'NONE', ( #23173, #14470, #28097, #1924 ) ) ;
#22787 = CARTESIAN_POINT ( 'NONE',  ( 68.32499999726881867, 145.8408176439707802, 12.60653300113718345 ) ) ;
#22788 = CARTESIAN_POINT ( 'NONE',  ( 6.815964470354069604, -1.383691465878164717, -6.173460172893482145 ) ) ;
#22789 = DIRECTION ( 'NONE',  ( 0.000000000000000000, 0.9988620819214347746, -0.04769215134146093105 ) ) ;
#22790 = VECTOR ( 'NONE', #10664, 1000.000000000000000 ) ;
#22791 = CARTESIAN_POINT ( 'NONE',  ( 63.42499999726881299, 168.2552932293087906, -9.630534252274385310 ) ) ;
#22792 = DIRECTION ( 'NONE',  ( 0.1045284632676459352, 1.217938055844715641E-16, 0.9945218953682740670 ) ) ;
#22793 = CARTESIAN_POINT ( 'NONE',  ( -9.984503880673420539, 203.7031108863293980, 38.34886208192143897 ) ) ;
#22794 = ORIENTED_EDGE ( 'NONE', *, *, #14090, .F. ) ;
#22795 = DIRECTION ( 'NONE',  ( -0.000000000000000000, -0.000000000000000000, 1.000000000000000000 ) ) ;
#22796 = AXIS2_PLACEMENT_3D ( 'NONE', #14155, #29663, #24721 ) ;
#22797 = CARTESIAN_POINT ( 'NONE',  ( 6.878751942472530523, -3.924677726130933575, -6.573129608219091757 ) ) ;
#22798 = CARTESIAN_POINT ( 'NONE',  ( 86.01132485994283172, 167.7597621252805880, -9.270509831248443078 ) ) ;
#22799 = CARTESIAN_POINT ( 'NONE',  ( -4.984841277089891776, 213.7757310962905990, 20.94886208192143684 ) ) ;
#22800 = CARTESIAN_POINT ( 'NONE',  ( -10.00000000000000711, 207.0476921513413515, 75.50113791807858377 ) ) ;
#22801 = CARTESIAN_POINT ( 'NONE',  ( 32.50000000000000000, 155.0000000000000000, -6.938893903907228378E-15 ) ) ;
#22802 = EDGE_CURVE ( 'NONE', #32112, #2182, #22670, .T. ) ;
#22803 = CARTESIAN_POINT ( 'NONE',  ( 10.01549611932653860, 210.2015048109876716, 46.85113791807856387 ) ) ;
#22804 = CARTESIAN_POINT ( 'NONE',  ( -8.062137200540920645, 212.9164362838581894, 15.80113791807856849 ) ) ;
#22805 = CARTESIAN_POINT ( 'NONE',  ( 2.426778023690261410, 199.3768101843759837, 2.601137918078566535 ) ) ;
#22806 = CARTESIAN_POINT ( 'NONE',  ( 60.00000000000000000, 7.347880794884118356E-15, 35.00000000000000000 ) ) ;
#22807 = CARTESIAN_POINT ( 'NONE',  ( 37.12499999726881583, 155.0000000000000000, -15.58253175000000823 ) ) ;
#22808 = CARTESIAN_POINT ( 'NONE',  ( 3.662846001190051659, 195.5725841191953691, 26.60113791807856742 ) ) ;
#22809 = FACE_OUTER_BOUND ( 'NONE', #32827, .T. ) ;
#22810 = CARTESIAN_POINT ( 'NONE',  ( 10.01549611932653860, 210.2015048109876716, 73.85113791807857808 ) ) ;
#22811 = CARTESIAN_POINT ( 'NONE',  ( -10.00000000000000711, 207.0476921513413515, 48.50113791807856956 ) ) ;
#22812 = CARTESIAN_POINT ( 'NONE',  ( 104.9083388212530537, 155.0000000000000000, -32.00000000000000000 ) ) ;
#22813 = CARTESIAN_POINT ( 'NONE',  ( 34.88867513459481984, 159.8737954434937478, -14.99999999999993072 ) ) ;
#22814 = CARTESIAN_POINT ( 'NONE',  ( 9.736236675708031640, 199.9851607334238963, 13.29886208192143826 ) ) ;
#22815 = CARTESIAN_POINT ( 'NONE',  ( 3.044812012439969795, 216.5253028482143520, 21.39886208192143613 ) ) ;
#22816 = CARTESIAN_POINT ( 'NONE',  ( 70.19999999453763451, 163.5228861582408797, -11.73074641843674470 ) ) ;
#22817 = ORIENTED_EDGE ( 'NONE', *, *, #32617, .T. ) ;
#22818 = CARTESIAN_POINT ( 'NONE',  ( 12.00000000000000711, 206.9523078486586485, 56.00113791807856956 ) ) ;
#22819 = CIRCLE ( 'NONE', #21731, 7.500000000000001776 ) ;
#22820 = CARTESIAN_POINT ( 'NONE',  ( -7.984503880673488041, 209.6470497212046098, 81.65113791807856103 ) ) ;
#22821 = CARTESIAN_POINT ( 'NONE',  ( 3.135527875058981895, 197.5041725223112792, 40.59886208192143187 ) ) ;
#22822 = DIRECTION ( 'NONE',  ( 0.000000000000000000, 0.000000000000000000, -1.000000000000000000 ) ) ;
#22823 = ORIENTED_EDGE ( 'NONE', *, *, #6664, .F. ) ;
#22824 = EDGE_LOOP ( 'NONE', ( #2766, #28248, #26143, #31703 ) ) ;
#22825 = ORIENTED_EDGE ( 'NONE', *, *, #12519, .T. ) ;
#22826 = DIRECTION ( 'NONE',  ( 0.000000000000000000, 0.000000000000000000, 1.000000000000000000 ) ) ;
#22827 = CARTESIAN_POINT ( 'NONE',  ( 6.837824896291514243, 3.947820044545427454, -6.564402953523716278 ) ) ;
#22828 = ORIENTED_EDGE ( 'NONE', *, *, #32504, .F. ) ;
#22829 = CARTESIAN_POINT ( 'NONE',  ( 0.05014649552807626948, 215.4116977939061144, 28.25113791807856245 ) ) ;
#22830 = CARTESIAN_POINT ( 'NONE',  ( -8.331345277524542681, 1.020295532671184640E-15, -7.381345277524544279 ) ) ;
#22831 = CARTESIAN_POINT ( 'NONE',  ( -9.984503880673420539, 203.7031108863293980, 14.34886208192143542 ) ) ;
#22832 = CARTESIAN_POINT ( 'NONE',  ( 57.37499999726880873, 155.0000000000000000, -15.58253175000000823 ) ) ;
#22833 = EDGE_LOOP ( 'NONE', ( #26967, #31020, #4423, #23347 ) ) ;
#22834 = CARTESIAN_POINT ( 'NONE',  ( -8.015496119326531499, 204.4483345814780364, 57.35113791807857098 ) ) ;
#22835 = CARTESIAN_POINT ( 'NONE',  ( 3.250000000000001332, -5.629165124598862313, -5.592027715088713435 ) ) ;
#22836 = CARTESIAN_POINT ( 'NONE',  ( 4.000000000000003553, 0.000000000000000000, 3.500000000000000000 ) ) ;
#22837 = CARTESIAN_POINT ( 'NONE',  ( -8.062137200540822946, 201.0835637161416400, 101.1988620819214475 ) ) ;
#22838 = CARTESIAN_POINT ( 'NONE',  ( 67.27499999726879309, 149.9369285172503510, -15.58253175000000823 ) ) ;
#22839 = CARTESIAN_POINT ( 'NONE',  ( 3.044812012440130555, 197.4746971517856764, 44.60113791807857098 ) ) ;
#22840 = CARTESIAN_POINT ( 'NONE',  ( -6.815830331203685866, -0.6619522098568484392, -6.171384342982615401 ) ) ;
#22841 =( BOUNDED_SURFACE ( )  B_SPLINE_SURFACE ( 3, 2, ( 
 ( #15240, #12179, #20180 ),
 ( #4680, #19843, #28192 ),
 ( #17973, #12520, #4850 ),
 ( #27839, #1779, #22908 ),
 ( #33302, #4509, #25631 ),
 ( #24962, #30239, #5020 ) ),
 .UNSPECIFIED., .F., .F., .T. ) 
 B_SPLINE_SURFACE_WITH_KNOTS ( ( 4, 2, 4 ),
 ( 3, 3 ),
 ( 0.003190620565844220352, 0.007281897438794486706, 0.01137317431174475306 ),
 ( 0.000000000000000000, 1.000000000000000000 ),
 .UNSPECIFIED. ) 
 GEOMETRIC_REPRESENTATION_ITEM ( )  RATIONAL_B_SPLINE_SURFACE ( (
 ( 1.000000000000000000, 0.8047731410850402778, 1.000000000000000000),
 ( 1.000000000000000000, 0.8125552299142427826, 1.000000000000000000),
 ( 1.000000000000000000, 0.8191520442908248878, 1.000000000000000000),
 ( 1.000000000000000000, 0.8191520442871482732, 1.000000000000000000),
 ( 1.000000000000000000, 0.8125552299170040182, 1.000000000000000000),
 ( 1.000000000000000000, 0.8047731410850399447, 1.000000000000000000) ) ) 
 REPRESENTATION_ITEM ( '' )  SURFACE ( )  );
#22842 = EDGE_CURVE ( 'NONE', #4349, #20988, #28142, .T. ) ;
#22843 = CARTESIAN_POINT ( 'NONE',  ( -10.00000000000000711, 207.0476921513413515, 18.50113791807856956 ) ) ;
#22844 = CARTESIAN_POINT ( 'NONE',  ( -59.99999999999998579, -6.938893903907228378E-15, -45.00000000000000711 ) ) ;
#22845 = CARTESIAN_POINT ( 'NONE',  ( 85.20000000000000284, 167.3344367211045096, 8.961492836873468093 ) ) ;
#22846 = DIRECTION ( 'NONE',  ( -0.000000000000000000, -0.000000000000000000, 1.000000000000000000 ) ) ;
#22847 = FACE_OUTER_BOUND ( 'NONE', #28313, .T. ) ;
#22848 = CARTESIAN_POINT ( 'NONE',  ( -9.736236675707914401, 199.9851607334237542, 3.201137918078565736 ) ) ;
#22849 = DIRECTION ( 'NONE',  ( -1.000000000000000000, 0.000000000000000000, 0.000000000000000000 ) ) ;
#22850 = CARTESIAN_POINT ( 'NONE',  ( 53.37499999726881583, 155.0000000000000000, -15.58253175000000823 ) ) ;
#22851 = CARTESIAN_POINT ( 'NONE',  ( -8.118202686958039038, 201.1607312380087080, 51.20113791807857240 ) ) ;
#22852 = CARTESIAN_POINT ( 'NONE',  ( 84.82499999726880446, 141.7447067706911810, -9.630534252274385310 ) ) ;
#22853 = ADVANCED_FACE ( 'NONE', ( #18257 ), #10098, .F. ) ;
#22854 = DIRECTION ( 'NONE',  ( 0.5000000000000006661, 0.8660254037844383745, -0.000000000000000000 ) ) ;
#22855 = CARTESIAN_POINT ( 'NONE',  ( -6.250000000000000000, -5.051814855409233473, -7.198902722707430257 ) ) ;
#22856 = CARTESIAN_POINT ( 'NONE',  ( 54.19999999453763451, 163.5228861582408797, -11.73074641843674470 ) ) ;
#22857 = ORIENTED_EDGE ( 'NONE', *, *, #14160, .T. ) ;
#22858 = CARTESIAN_POINT ( 'NONE',  ( -9.680171189290831535, 214.0920067884431148, 33.80113791807856671 ) ) ;
#22859 = CARTESIAN_POINT ( 'NONE',  ( 61.61132485994281893, 150.1262045565064227, -15.00000000000002665 ) ) ;
#22860 = CARTESIAN_POINT ( 'NONE',  ( -6.139770520408224463, 198.4640165459539389, 14.04886208192143648 ) ) ;
#22861 = CARTESIAN_POINT ( 'NONE',  ( 7.894787914004607998, 1.243647571710251278E-13, -7.591390474663425536 ) ) ;
#22862 = ORIENTED_EDGE ( 'NONE', *, *, #19558, .F. ) ;
#22863 = CARTESIAN_POINT ( 'NONE',  ( 9.984503880673470277, 203.7031108863295401, 11.15113791807856636 ) ) ;
#22864 = CARTESIAN_POINT ( 'NONE',  ( -10.01549611932653860, 203.7984951890123284, 57.35113791807856387 ) ) ;
#22865 = EDGE_CURVE ( 'NONE', #32282, #26009, #23742, .T. ) ;
#22866 = EDGE_LOOP ( 'NONE', ( #5843, #18673 ) ) ;
#22867 = CARTESIAN_POINT ( 'NONE',  ( 6.444103211790928043, 211.7408657792734061, 21.69886208192144039 ) ) ;
#22868 = CARTESIAN_POINT ( 'NONE',  ( 125.5000000000000000, 152.8500000000011028, 106.0000000000000426 ) ) ;
#22869 = ORIENTED_EDGE ( 'NONE', *, *, #17904, .T. ) ;
#22870 = CARTESIAN_POINT ( 'NONE',  ( -7.984503880673488041, 209.6470497212046098, 6.651137918078566358 ) ) ;
#22871 = EDGE_CURVE ( 'NONE', #29320, #26329, #5259, .T. ) ;
#22872 = CARTESIAN_POINT ( 'NONE',  ( 4.000000000000000000, 4.506943796211476502E-15, 3.047499999999998543 ) ) ;
#22873 = CARTESIAN_POINT ( 'NONE',  ( 3.662846001189864698, 218.4274158808046593, 90.39886208192143613 ) ) ;
#22874 = CARTESIAN_POINT ( 'NONE',  ( 36.97499999726881015, 140.1801316387863778, -4.815267126137194431 ) ) ;
#22875 = ORIENTED_EDGE ( 'NONE', *, *, #31845, .F. ) ;
#22876 = CARTESIAN_POINT ( 'NONE',  ( 44.02499999726881441, 160.0630714827496206, 15.58253174999999402 ) ) ;
#22877 = FACE_OUTER_BOUND ( 'NONE', #16186, .T. ) ;
#22878 = CARTESIAN_POINT ( 'NONE',  ( 54.01132485994280330, 167.7597621252805880, -9.270509831248443078 ) ) ;
#22879 = CARTESIAN_POINT ( 'NONE',  ( -6.220909254589682469, 215.4770327129946850, 68.94886208192140487 ) ) ;
#22880 = CARTESIAN_POINT ( 'NONE',  ( 44.67499999726881299, 141.7447067706911810, 9.630534252274376428 ) ) ;
#22881 = CARTESIAN_POINT ( 'NONE',  ( -67.50001199999999812, 142.1924241995298246, 11.23405475987244095 ) ) ;
#22882 = CARTESIAN_POINT ( 'NONE',  ( 10.00000000000000711, 206.9523078486586201, 5.001137918078565114 ) ) ;
#22883 = CARTESIAN_POINT ( 'NONE',  ( -25.25629716696160543, -17.17253483735097674, -1.708299986272441284 ) ) ;
#22884 = CARTESIAN_POINT ( 'NONE',  ( 67.80000000000001137, 142.6655632788954620, 8.961492836873471646 ) ) ;
#22885 = CARTESIAN_POINT ( 'NONE',  ( -3.044812012440131443, 216.5253028482142952, 88.10113791807857808 ) ) ;
#22886 = DIRECTION ( 'NONE',  ( -1.000000000000000000, 0.000000000000000000, 0.000000000000000000 ) ) ;
#22887 = CARTESIAN_POINT ( 'NONE',  ( -6.139770520408369237, 215.5359834540460042, 78.95113791807858661 ) ) ;
#22888 = FACE_OUTER_BOUND ( 'NONE', #23291, .T. ) ;
#22889 = CARTESIAN_POINT ( 'NONE',  ( 34.57499999726881157, 145.8408176439707802, 12.60653300113718345 ) ) ;
#22890 = CARTESIAN_POINT ( 'NONE',  ( 12.00000000000000711, 207.0476921513415220, 87.99886208192144466 ) ) ;
#22891 = CARTESIAN_POINT ( 'NONE',  ( 62.22499999726881725, 149.9369285172503510, 15.58253174999999580 ) ) ;
#22893 = ORIENTED_EDGE ( 'NONE', *, *, #11675, .T. ) ;
#22892 = CARTESIAN_POINT ( 'NONE',  ( 8.118202686958039038, 212.8392687619912635, 34.70113791807857240 ) ) ;
#22894 = DIRECTION ( 'NONE',  ( 0.000000000000000000, 0.000000000000000000, -1.000000000000000000 ) ) ;
#22895 = CARTESIAN_POINT ( 'NONE',  ( 87.37499999726880162, 155.0000000000000000, -15.58253175000000823 ) ) ;
#22896 = CARTESIAN_POINT ( 'NONE',  ( -11.98450388067348804, 210.9467285061362247, 93.65113791807857524 ) ) ;
#22897 = EDGE_CURVE ( 'NONE', #27493, #29612, #13395, .T. ) ;
#22898 = ADVANCED_FACE ( 'NONE', ( #7874 ), #17929, .F. ) ;
#22899 = CARTESIAN_POINT ( 'NONE',  ( -10.67684754974910888, 206.2195024190491210, 104.1863779807122370 ) ) ;
#22900 = EDGE_LOOP ( 'NONE', ( #9922, #7415, #29105, #5356, #16596, #20181, #23819 ) ) ;
#22901 = CARTESIAN_POINT ( 'NONE',  ( -3.135527875058982783, 216.4958274776886924, 90.09886208192143897 ) ) ;
#22902 = CARTESIAN_POINT ( 'NONE',  ( -7.375838497908014268, 196.7627149292498530, 26.04886208192144181 ) ) ;
#22903 = CARTESIAN_POINT ( 'NONE',  ( -47.49999999999998579, 155.0000000000000000, 11.99999999999999645 ) ) ;
#22904 = CARTESIAN_POINT ( 'NONE',  ( 3.044812012440130555, 197.4746971517856764, 32.60113791807857098 ) ) ;
#22905 = CARTESIAN_POINT ( 'NONE',  ( 65.88867513459484826, 150.1262045565062806, 14.99999999999992006 ) ) ;
#22906 = ADVANCED_FACE ( 'NONE', ( #25411 ), #3069, .T. ) ;
#22907 = CARTESIAN_POINT ( 'NONE',  ( 3.135527875058981895, 197.5041725223112792, 97.59886208192143897 ) ) ;
#22908 = CARTESIAN_POINT ( 'NONE',  ( 2.241046694639346804, 6.576374040526301812, -6.171384342982712212 ) ) ;
#22909 = VERTEX_POINT ( 'NONE', #22861 ) ;
#22910 = CARTESIAN_POINT ( 'NONE',  ( 117.5000000000000000, 126.0449016395812691, -103.9084171661922369 ) ) ;
#22911 = CARTESIAN_POINT ( 'NONE',  ( -6.444103211790928043, 202.2591342207265939, 83.19886208192144750 ) ) ;
#22912 = ADVANCED_FACE ( 'NONE', ( #33252 ), #11239, .T. ) ;
#22913 = VERTEX_POINT ( 'NONE', #2424 ) ;
#22914 = APPLICATION_CONTEXT ( 'automotive_design' ) ;
#22915 = CYLINDRICAL_SURFACE ( 'NONE', #17315, 112.0000000000000711 ) ;
#22916 = ORIENTED_EDGE ( 'NONE', *, *, #23137, .T. ) ;
#22917 = DIRECTION ( 'NONE',  ( 0.000000000000000000, 0.000000000000000000, 1.000000000000000000 ) ) ;
#22918 = CARTESIAN_POINT ( 'NONE',  ( 79.62499999726881583, 171.3844434931184253, -7.942151717890132712E-15 ) ) ;
#22919 = FACE_BOUND ( 'NONE', #18225, .T. ) ;
#22920 = CARTESIAN_POINT ( 'NONE',  ( -0.05014649552807731031, 198.5883022060938572, 80.75113791807856956 ) ) ;
#22921 = DIRECTION ( 'NONE',  ( -1.000000000000000000, 0.000000000000000000, 0.000000000000000000 ) ) ;
#22922 = AXIS2_PLACEMENT_3D ( 'NONE', #30555, #7391, #15219 ) ;
#22923 = CARTESIAN_POINT ( 'NONE',  ( 40.79999999999999716, 167.3344367211045096, -8.961492836873482304 ) ) ;
#22924 = CARTESIAN_POINT ( 'NONE',  ( -8.000000000000008882, 206.9523078486584780, 50.49886208192144466 ) ) ;
#22925 = CARTESIAN_POINT ( 'NONE',  ( 8.062137200540920645, 201.0835637161417822, -0.6988620819214342861 ) ) ;
#22926 = CARTESIAN_POINT ( 'NONE',  ( -6.500000000000000888, 4.012863338656273982, -6.470131626772281486 ) ) ;
#22927 = CARTESIAN_POINT ( 'NONE',  ( -130.2500000000000000, 6.429395695523609083E-16, 35.00000599999999906 ) ) ;
#22928 = CARTESIAN_POINT ( 'NONE',  ( 55.22499999726880304, 160.0630714827496206, -15.58253175000000823 ) ) ;
#22929 = CARTESIAN_POINT ( 'NONE',  ( 71.67499999726881299, 168.2552932293087906, -9.630534252274385310 ) ) ;
#22930 = CARTESIAN_POINT ( 'NONE',  ( 9.736236675707914401, 214.0148392665762458, 67.70113791807857240 ) ) ;
#22931 = FACE_BOUND ( 'NONE', #17755, .T. ) ;
#22932 = CARTESIAN_POINT ( 'NONE',  ( -3.662846001190052991, 218.4274158808045740, 10.10113791807856742 ) ) ;
#22933 = ADVANCED_FACE ( 'NONE', ( #690, #21474 ), #26418, .T. ) ;
#22934 = CARTESIAN_POINT ( 'NONE',  ( -6.220909254589537696, 198.5229672870051445, 75.05113791807858092 ) ) ;
#22935 = CARTESIAN_POINT ( 'NONE',  ( -12.00000000000000711, 206.9523078486584780, 44.49886208192143755 ) ) ;
#22936 = CARTESIAN_POINT ( 'NONE',  ( 3.135527875058981895, 197.5041725223112792, 55.59886208192143187 ) ) ;
#22937 = DIRECTION ( 'NONE',  ( 1.000000000000000000, 0.000000000000000000, 0.000000000000000000 ) ) ;
#22938 = CARTESIAN_POINT ( 'NONE',  ( 12.01549611932652972, 210.8513442034534933, 88.85113791807857808 ) ) ;
#22939 = CARTESIAN_POINT ( 'NONE',  ( -52.50000000000002132, 155.0000000000000000, -6.938893903907228378E-15 ) ) ;
#22940 = CARTESIAN_POINT ( 'NONE',  ( -0.05014649552810635652, 196.4853777576173002, 5.751137918078563338 ) ) ;
#22941 = EDGE_CURVE ( 'NONE', #20617, #29364, #15869, .T. ) ;
#22942 = CARTESIAN_POINT ( 'NONE',  ( -3.044812012439970683, 197.4746971517856196, 67.89886208192143613 ) ) ;
#22943 = DIRECTION ( 'NONE',  ( 1.000000000000000000, -0.000000000000000000, -0.000000000000000000 ) ) ;
#22944 = ORIENTED_EDGE ( 'NONE', *, *, #5023, .F. ) ;
#22945 = CARTESIAN_POINT ( 'NONE',  ( -12.00000000000000711, 206.9523078486584780, 68.49886208192144466 ) ) ;
#22946 = AXIS2_PLACEMENT_3D ( 'NONE', #3105, #26605, #3602 ) ;
#22947 = CARTESIAN_POINT ( 'NONE',  ( 8.062137200540920645, 201.0835637161417822, 92.30113791807858092 ) ) ;
#22948 = ORIENTED_EDGE ( 'NONE', *, *, #32658, .F. ) ;
#22949 = CARTESIAN_POINT ( 'NONE',  ( 80.27499999726879309, 160.0630714827496206, 15.58253174999999402 ) ) ;
#22950 = CARTESIAN_POINT ( 'NONE',  ( 8.000000000000008882, 207.0476921513415220, 51.99886208192144466 ) ) ;
#22951 = VERTEX_POINT ( 'NONE', #3243 ) ;
#22952 = CARTESIAN_POINT ( 'NONE',  ( 69.62499999726881583, 171.3844434931184253, -7.942151717890134290E-15 ) ) ;
#22953 = PLANE ( 'NONE',  #995 ) ;
#22954 = CARTESIAN_POINT ( 'NONE',  ( -6.288404560131954923, -5.029641972278938944, -0.4504974108212008721 ) ) ;
#22955 = AXIS2_PLACEMENT_3D ( 'NONE', #2778, #15035, #33268 ) ;
#22956 = CARTESIAN_POINT ( 'NONE',  ( 62.92499999726880588, 145.8408176439707802, -12.60653300113719588 ) ) ;
#22957 = DIRECTION ( 'NONE',  ( 0.000000000000000000, 0.000000000000000000, -1.000000000000000000 ) ) ;
#22958 = CARTESIAN_POINT ( 'NONE',  ( -9.984503880673420539, 203.7031108863293980, 56.34886208192141765 ) ) ;
#22959 = ORIENTED_EDGE ( 'NONE', *, *, #4396, .F. ) ;
#22960 = CARTESIAN_POINT ( 'NONE',  ( 92.60208470531341618, 155.0000000000000000, 32.00000000000001421 ) ) ;
#22961 = CARTESIAN_POINT ( 'NONE',  ( 112.4999999999999858, 155.0000000000000000, 11.99999999999999645 ) ) ;
#22962 = CARTESIAN_POINT ( 'NONE',  ( 115.4999999999999858, 207.9999999999998010, -89.64869280115065919 ) ) ;
#22963 = CARTESIAN_POINT ( 'NONE',  ( -8.015496119326597224, 209.5516654185217362, 23.64886208192143968 ) ) ;
#22964 = CARTESIAN_POINT ( 'NONE',  ( -6.220909254589537696, 198.5229672870051161, 66.05113791807858092 ) ) ;
#22965 = DIRECTION ( 'NONE',  ( 0.000000000000000000, -1.000000000000000000, 0.000000000000000000 ) ) ;
#22966 = CARTESIAN_POINT ( 'NONE',  ( -10.00000000000000711, 207.0476921513413515, 60.50113791807857666 ) ) ;
#22967 = CARTESIAN_POINT ( 'NONE',  ( 6.220909254589536808, 215.4770327129947702, 28.55113791807855961 ) ) ;
#22968 = CIRCLE ( 'NONE', #15817, 27.50000000000000355 ) ;
#22969 = CARTESIAN_POINT ( 'NONE',  ( -4.984841277089726574, 200.2242689037092305, 9.051137918078564937 ) ) ;
#22970 = DIRECTION ( 'NONE',  ( 0.000000000000000000, 0.000000000000000000, 1.000000000000000000 ) ) ;
#22971 = CARTESIAN_POINT ( 'NONE',  ( 36.62499999726881583, 138.6155565068815747, -3.929120461958505118E-15 ) ) ;
#22972 = CARTESIAN_POINT ( 'NONE',  ( -11.98450388067348804, 210.9467285061362247, 33.65113791807856813 ) ) ;
#22973 = FACE_OUTER_BOUND ( 'NONE', #2077, .T. ) ;
#22974 = CARTESIAN_POINT ( 'NONE',  ( -6.220909254589537696, 198.5229672870051161, 87.05113791807856671 ) ) ;
#22975 = CARTESIAN_POINT ( 'NONE',  ( -6.220909254589537696, 198.5229672870051445, 51.05113791807856671 ) ) ;
#22976 = CARTESIAN_POINT ( 'NONE',  ( 0.000000000000000000, 1.759474945355386399, 3.047499999999995879 ) ) ;
#22977 = CARTESIAN_POINT ( 'NONE',  ( -7.456977232089471386, 217.1783343296987709, 8.948862081921433287 ) ) ;
#22978 = CARTESIAN_POINT ( 'NONE',  ( -6.220909254589682469, 215.4770327129947134, 29.94886208192143329 ) ) ;
#22979 = CARTESIAN_POINT ( 'NONE',  ( 75.89999999453763735, 150.2886644046228639, -14.50000000000000888 ) ) ;
#22980 = AXIS2_PLACEMENT_3D ( 'NONE', #32046, #8218, #5486 ) ;
#22981 = ORIENTED_EDGE ( 'NONE', *, *, #4756, .T. ) ;
#22982 = CARTESIAN_POINT ( 'NONE',  ( -9.736236675707914401, 199.9851607334237542, 57.20113791807856529 ) ) ;
#22983 = CARTESIAN_POINT ( 'NONE',  ( -0.05014649552807731031, 198.5883022060938572, 77.75113791807856956 ) ) ;
#22984 = CIRCLE ( 'NONE', #12108, 2.500000000000000000 ) ;
#22985 = CARTESIAN_POINT ( 'NONE',  ( 6.139770520408223575, 215.5359834540460611, 39.54886208192143471 ) ) ;
#22986 = CARTESIAN_POINT ( 'NONE',  ( 104.9083388212530537, 155.0000000000000000, 0.000000000000000000 ) ) ;
#22987 = EDGE_LOOP ( 'NONE', ( #18604, #19006, #31573, #32619 ) ) ;
#22988 = CARTESIAN_POINT ( 'NONE',  ( -9.680171189290716072, 199.9079932115567146, 41.19886208192144039 ) ) ;
#22989 = VERTEX_POINT ( 'NONE', #29311 ) ;
#22990 = ORIENTED_EDGE ( 'NONE', *, *, #19529, .F. ) ;
#22991 = ADVANCED_FACE ( 'NONE', ( #31858 ), #24363, .T. ) ;
#22992 = LINE ( 'NONE', #10064, #6962 ) ;
#22993 = AXIS2_PLACEMENT_3D ( 'NONE', #22671, #30509, #7174 ) ;
#22994 = CARTESIAN_POINT ( 'NONE',  ( 0.000000000000000000, -2.342598717236903383, 4.057500000000001883 ) ) ;
#22995 = VERTEX_POINT ( 'NONE', #16350 ) ;
#22996 = CARTESIAN_POINT ( 'NONE',  ( 4.903702542908601636, 200.1653181626581102, 32.45113791807857240 ) ) ;
#22997 = CARTESIAN_POINT ( 'NONE',  ( -52.50000000000002132, 0.000000000000000000, 20.00000000000001776 ) ) ;
#22998 = CARTESIAN_POINT ( 'NONE',  ( -9.984503880673420539, 203.7031108863293980, 17.34886208192143542 ) ) ;
#22999 = CARTESIAN_POINT ( 'NONE',  ( 57.57499999726881157, 164.1591823560292198, -12.60653300113719766 ) ) ;
#23000 = ORIENTED_EDGE ( 'NONE', *, *, #16996, .F. ) ;
#23001 = CARTESIAN_POINT ( 'NONE',  ( 2.517493886308900919, 214.5937144450984420, 61.40113791807856813 ) ) ;
#23002 = CARTESIAN_POINT ( 'NONE',  ( 68.48867513459484258, 142.2402378747194405, -9.270509831248439525 ) ) ;
#23003 = AXIS2_PLACEMENT_3D ( 'NONE', #23068, #8079, #10472 ) ;
#23004 = CARTESIAN_POINT ( 'NONE',  ( 57.41132485994281609, 142.2402378747194405, -9.270509831248439525 ) ) ;
#23005 = CARTESIAN_POINT ( 'NONE',  ( 8.062137200540822946, 212.9164362838583315, 99.69886208192144750 ) ) ;
#23006 = CIRCLE ( 'NONE', #27327, 17.00000000000000355 ) ;
#23007 = CARTESIAN_POINT ( 'NONE',  ( 66.97499999726881015, 140.1801316387863778, -4.815267126137194431 ) ) ;
#23008 = CARTESIAN_POINT ( 'NONE',  ( 0.05014649552810505201, 217.5146222423826714, 46.25113791807855534 ) ) ;
#23009 = CARTESIAN_POINT ( 'NONE',  ( 3.135527875058820690, 216.4958274776887492, 22.40113791807856458 ) ) ;
#23010 = CARTESIAN_POINT ( 'NONE',  ( 10.00000000000000711, 207.0476921513415220, 99.99886208192143044 ) ) ;
#23011 = SHAPE_DEFINITION_REPRESENTATION ( #32809, #16299 ) ;
#23012 = CARTESIAN_POINT ( 'NONE',  ( 87.10000000000000853, 168.7903194862797420, 4.480746418436729606 ) ) ;
#23013 = CARTESIAN_POINT ( 'NONE',  ( 0.000000000000000000, 3.518949890710768802, -4.770489558936219510E-15 ) ) ;
#23014 = DIRECTION ( 'NONE',  ( 0.000000000000000000, -0.000000000000000000, 1.000000000000000000 ) ) ;
#23015 = CARTESIAN_POINT ( 'NONE',  ( 9.736236675707914401, 214.0148392665762458, 1.701137918078565736 ) ) ;
#23016 = CARTESIAN_POINT ( 'NONE',  ( 47.97499999726881015, 169.8198683612136222, 4.815267126137181997 ) ) ;
#23017 = CARTESIAN_POINT ( 'NONE',  ( -10.00000000000000711, 207.0476921513413515, 42.50113791807856956 ) ) ;
#23018 = CARTESIAN_POINT ( 'NONE',  ( 98.19869130599479945, 155.0000000000000000, 0.000000000000000000 ) ) ;
#23019 = VECTOR ( 'NONE', #12076, 1000.000000000000227 ) ;
#23020 = CARTESIAN_POINT ( 'NONE',  ( 33.12499999726880873, 155.0000000000000000, -15.58253175000000823 ) ) ;
#23021 = DIRECTION ( 'NONE',  ( 0.000000000000000000, 0.000000000000000000, 1.000000000000000000 ) ) ;
#23022 = CARTESIAN_POINT ( 'NONE',  ( 56.99999999453763166, 155.0000000000000000, 14.49999999999999467 ) ) ;
#23023 = EDGE_LOOP ( 'NONE', ( #17577, #15319, #31870, #5298, #17744 ) ) ;
#23024 = CARTESIAN_POINT ( 'NONE',  ( 12.00000000000000711, 206.9523078486586485, 26.00113791807856600 ) ) ;
#23025 = CARTESIAN_POINT ( 'NONE',  ( 37.48867513459482836, 167.7597621252805880, 9.270509831248428867 ) ) ;
#23026 = CARTESIAN_POINT ( 'NONE',  ( 10.00000000000000711, 207.0476921513415220, 9.998862081921435774 ) ) ;
#23027 = LINE ( 'NONE', #20132, #27545 ) ;
#23028 = ORIENTED_EDGE ( 'NONE', *, *, #629, .T. ) ;
#23029 = AXIS2_PLACEMENT_3D ( 'NONE', #28666, #15715, #13164 ) ;
#23030 = CARTESIAN_POINT ( 'NONE',  ( -10.01549611932653860, 203.7984951890123284, 9.351137918078569200 ) ) ;
#23031 = CARTESIAN_POINT ( 'NONE',  ( -10.00000000000000711, 207.0476921513413515, 66.50113791807856956 ) ) ;
#23032 = EDGE_LOOP ( 'NONE', ( #25329, #20567, #8011, #11177, #19417, #12170 ) ) ;
#23033 = CARTESIAN_POINT ( 'NONE',  ( -2.426778023690076225, 199.3768101843759553, 19.89886208192143613 ) ) ;
#23034 = EDGE_CURVE ( 'NONE', #30624, #1916, #5473, .T. ) ;
#23035 = CARTESIAN_POINT ( 'NONE',  ( 3.250000000000004441, 5.629165124598849879, 0.000000000000000000 ) ) ;
#23036 = EDGE_LOOP ( 'NONE', ( #5882, #24627, #3217, #9246, #778, #29113 ) ) ;
#23037 = CARTESIAN_POINT ( 'NONE',  ( 0.05014649552807626948, 215.4116977939061144, 4.251137918078566891 ) ) ;
#23038 = EDGE_CURVE ( 'NONE', #14731, #28067, #13802, .T. ) ;
#23039 = CARTESIAN_POINT ( 'NONE',  ( 3.662846001189864698, 218.4274158808046593, 84.39886208192143613 ) ) ;
#23040 = CARTESIAN_POINT ( 'NONE',  ( 37.27499999726880731, 149.9369285172503510, -15.58253175000000823 ) ) ;
#23041 = ORIENTED_EDGE ( 'NONE', *, *, #28138, .T. ) ;
#23042 = CARTESIAN_POINT ( 'NONE',  ( 42.62499999726881583, 138.6155565068815463, -3.929120461958505118E-15 ) ) ;
#23043 = CARTESIAN_POINT ( 'NONE',  ( 7.500000000000000888, 1.489914625144004523, -0.1187923833806749097 ) ) ;
#23044 = EDGE_CURVE ( 'NONE', #18472, #19014, #26129, .T. ) ;
#23045 = CARTESIAN_POINT ( 'NONE',  ( 6.139770520408368348, 198.4640165459539674, 11.45113791807856707 ) ) ;
#23046 = VECTOR ( 'NONE', #15139, 1000.000000000000000 ) ;
#23047 = COLOUR_RGB ( '', 0.40784314, 0.44705882, 0.49803922) ;
#23048 = CARTESIAN_POINT ( 'NONE',  ( 6.139770520408223575, 215.5359834540460611, 69.54886208192142760 ) ) ;
#23049 = CARTESIAN_POINT ( 'NONE',  ( 44.07499999726881157, 168.2552932293087906, 9.630534252274372875 ) ) ;
#23050 = CARTESIAN_POINT ( 'NONE',  ( -67.50001199999996970, 142.1924241995297677, -11.23405475987242674 ) ) ;
#23051 = CARTESIAN_POINT ( 'NONE',  ( -0.05014649552810635652, 196.4853777576173002, 17.75113791807856245 ) ) ;
#23052 = PRODUCT ( 'spring', 'spring', '', ( #13782 ) ) ;
#23053 = CARTESIAN_POINT ( 'NONE',  ( 115.4999999999999858, 182.4348187808683690, 102.3881375866409513 ) ) ;
#23054 = AXIS2_PLACEMENT_3D ( 'NONE', #32004, #13442, #26551 ) ;
#23055 = CARTESIAN_POINT ( 'NONE',  ( 69.40000000000001990, 159.7113355953771077, 14.49999999999999289 ) ) ;
#23056 = CARTESIAN_POINT ( 'NONE',  ( -6.220909254589537696, 198.5229672870051161, 102.0511379180785383 ) ) ;
#23057 = CARTESIAN_POINT ( 'NONE',  ( 1.750000000000014211, 3.031088913245526317, -2.899999999999999911 ) ) ;
#23058 = CARTESIAN_POINT ( 'NONE',  ( 6.220909254589536808, 215.4770327129947702, 76.55113791807855250 ) ) ;
#23059 = CIRCLE ( 'NONE', #2368, 32.00000000000002842 ) ;
#23060 = DIRECTION ( 'NONE',  ( 0.000000000000000000, 0.000000000000000000, -1.000000000000000000 ) ) ;
#23061 = CARTESIAN_POINT ( 'NONE',  ( 3.753561863808876797, 195.6020594897209719, 85.59886208192143897 ) ) ;
#23062 = CARTESIAN_POINT ( 'NONE',  ( 72.72499999726881015, 140.1801316387863778, -4.815267126137194431 ) ) ;
#23063 = EDGE_LOOP ( 'NONE', ( #16278, #22096, #30967, #15831 ) ) ;
#23064 = CARTESIAN_POINT ( 'NONE',  ( -59.75243488385262225, 194.9412087183787037, 2.169815710172075196 ) ) ;
#23065 = CARTESIAN_POINT ( 'NONE',  ( 35.79999999453762882, 146.4771138417591203, -11.73074641843674470 ) ) ;
#23066 = CARTESIAN_POINT ( 'NONE',  ( -12.01549611932652972, 203.1486557965464499, 99.35113791807857808 ) ) ;
#23067 = EDGE_CURVE ( 'NONE', #7672, #3615, #7828, .T. ) ;
#23068 = CARTESIAN_POINT ( 'NONE',  ( 92.70168066101555837, 155.0000000000000000, 0.000000000000000000 ) ) ;
#23069 = ORIENTED_EDGE ( 'NONE', *, *, #30538, .T. ) ;
#23070 = CARTESIAN_POINT ( 'NONE',  ( -9.984503880673420539, 203.7031108863293980, 83.34886208192142476 ) ) ;
#23071 = CARTESIAN_POINT ( 'NONE',  ( 3.753561863808876797, 195.6020594897209719, 22.59886208192143542 ) ) ;
#23072 = DIRECTION ( 'NONE',  ( 1.000000000000000000, -0.000000000000000000, -0.000000000000000000 ) ) ;
#23073 = CARTESIAN_POINT ( 'NONE',  ( 0.05014649552810505201, 217.5146222423826714, 28.25113791807855890 ) ) ;
#23074 = ORIENTED_EDGE ( 'NONE', *, *, #19952, .T. ) ;
#23075 = CARTESIAN_POINT ( 'NONE',  ( -10.01549611932659722, 210.2015048109875011, 95.64886208192140771 ) ) ;
#23076 = EDGE_CURVE ( 'NONE', #23340, #16267, #16521, .T. ) ;
#23077 = CARTESIAN_POINT ( 'NONE',  ( 4.000000000000000000, 1.759474945355386399, 3.047499999999995879 ) ) ;
#23078 = AXIS2_PLACEMENT_3D ( 'NONE', #14964, #4065, #1347 ) ;
#23079 = ORIENTED_EDGE ( 'NONE', *, *, #23649, .T. ) ;
#23080 = DIRECTION ( 'NONE',  ( 0.000000000000000000, 0.000000000000000000, 1.000000000000000000 ) ) ;
#23081 = CARTESIAN_POINT ( 'NONE',  ( -8.000000000000008882, 206.9523078486584780, 80.49886208192144466 ) ) ;
#23082 =( BOUNDED_CURVE ( )  B_SPLINE_CURVE ( 2, ( #1806, #4029, #12203, #32309, #29756, #27199, #3855, #14247, #28561, #15595, #12541 ),
 .UNSPECIFIED., .F., .T. ) 
 B_SPLINE_CURVE_WITH_KNOTS ( ( 3, 2, 2, 2, 2, 3 ),
 ( 0.1249999999999999722, 0.1285714285714285310, 0.1321428571428571175, 0.1357142857142857040, 0.1392857142857142905, 0.1428571428571428492 ),
 .UNSPECIFIED. ) 
 CURVE ( )  GEOMETRIC_REPRESENTATION_ITEM ( )  RATIONAL_B_SPLINE_CURVE ( ( 1.000000000000000444, 0.9510565162951530871, 1.000000000000000000, 0.9510565162951534202, 1.000000000000000000, 0.9510565162951534202, 1.000000000000000000, 0.9510565162951534202, 1.000000000000000000, 0.9510565162951534202, 1.000000000000000000 ) ) 
 REPRESENTATION_ITEM ( '' )  );
#23083 = VECTOR ( 'NONE', #6990, 1000.000000000000000 ) ;
#23084 = ORIENTED_EDGE ( 'NONE', *, *, #17645, .F. ) ;
#23085 = CARTESIAN_POINT ( 'NONE',  ( 125.0000000000000000, -24.99999999999995737, -20.00000000000000000 ) ) ;
#23086 = ORIENTED_EDGE ( 'NONE', *, *, #5025, .T. ) ;
#23087 = CARTESIAN_POINT ( 'NONE',  ( 92.70168066101555837, 155.0000000000000000, 13.00000000000003908 ) ) ;
#23088 = EDGE_CURVE ( 'NONE', #10286, #7343, #16760, .T. ) ;
#23089 = CARTESIAN_POINT ( 'NONE',  ( -4.984841277089726574, 200.2242689037092305, 63.05113791807858092 ) ) ;
#23090 = CARTESIAN_POINT ( 'NONE',  ( 84.62499999726880162, 138.6155565068815463, -3.929120461958505118E-15 ) ) ;
#23091 = CARTESIAN_POINT ( 'NONE',  ( -31.74999999999995737, 0.000000000000000000, 0.000000000000000000 ) ) ;
#23092 = CARTESIAN_POINT ( 'NONE',  ( -4.903702542908602524, 213.8346818373418898, 90.95113791807855819 ) ) ;
#23093 = DIRECTION ( 'NONE',  ( 0.000000000000000000, 0.000000000000000000, 1.000000000000000000 ) ) ;
#23094 =( NAMED_UNIT ( * ) PLANE_ANGLE_UNIT ( ) SI_UNIT ( $, .RADIAN. ) );
#23095 = CARTESIAN_POINT ( 'NONE',  ( 50.60000000000000142, 159.7113355953771077, -14.50000000000000888 ) ) ;
#23096 = CARTESIAN_POINT ( 'NONE',  ( -8.000000000000008882, 206.9523078486584780, 65.49886208192144466 ) ) ;
#23097 = CARTESIAN_POINT ( 'NONE',  ( 67.58867513459482268, 163.8167787843871110, 12.13525491562421621 ) ) ;
#23098 = EDGE_CURVE ( 'NONE', #25974, #6680, #11780, .T. ) ;
#23099 = CARTESIAN_POINT ( 'NONE',  ( 10.00000000000000711, 206.9523078486586201, -0.9988620819214343305 ) ) ;
#23100 = DIRECTION ( 'NONE',  ( 0.000000000000000000, 0.000000000000000000, -1.000000000000000000 ) ) ;
#23101 = VECTOR ( 'NONE', #29251, 1000.000000000000114 ) ;
#23102 = DIRECTION ( 'NONE',  ( -1.000000000000000000, -0.000000000000000000, -0.000000000000000000 ) ) ;
#23103 = CARTESIAN_POINT ( 'NONE',  ( 58.82499999726881867, 141.7447067706911810, -9.630534252274387086 ) ) ;
#23104 = CARTESIAN_POINT ( 'NONE',  ( 71.97499999726881015, 169.8198683612136222, 4.815267126137181997 ) ) ;
#23105 = CARTESIAN_POINT ( 'NONE',  ( 12.00000000000000711, 206.9523078486586485, 68.00113791807856956 ) ) ;
#23106 = FACE_BOUND ( 'NONE', #32161, .T. ) ;
#23107 = CARTESIAN_POINT ( 'NONE',  ( 9.736236675707914401, 214.0148392665762458, 7.701137918078567068 ) ) ;
#23108 = CARTESIAN_POINT ( 'NONE',  ( 8.062137200540920645, 201.0835637161417822, 86.30113791807856671 ) ) ;
#23109 = CARTESIAN_POINT ( 'NONE',  ( -3.662846001189865142, 195.5725841191952838, 52.89886208192143613 ) ) ;
#23110 = CARTESIAN_POINT ( 'NONE',  ( 8.062137200540822946, 212.9164362838583315, 57.69886208192144039 ) ) ;
#23111 = CARTESIAN_POINT ( 'NONE',  ( 0.000000000000000000, 0.000000000000000000, 0.000000000000000000 ) ) ;
#23112 = CARTESIAN_POINT ( 'NONE',  ( 12.00000000000000711, 206.9523078486586485, 98.00113791807856956 ) ) ;
#23113 = CYLINDRICAL_SURFACE ( 'NONE', #8840, 12.99999999999999822 ) ;
#23114 = CARTESIAN_POINT ( 'NONE',  ( -8.062137200540920645, 212.9164362838581894, 0.8011379180785658249 ) ) ;
#23115 = CARTESIAN_POINT ( 'NONE',  ( -3.044812012439970683, 197.4746971517856196, 70.89886208192143613 ) ) ;
#23116 = CARTESIAN_POINT ( 'NONE',  ( 27.50000000000000355, 0.000000000000000000, 0.000000000000000000 ) ) ;
#23117 = EDGE_LOOP ( 'NONE', ( #28574, #12091, #19491, #21553 ) ) ;
#23118 = CARTESIAN_POINT ( 'NONE',  ( -7.375838497908014268, 196.7627149292498530, 77.04886208192142760 ) ) ;
#23119 = CARTESIAN_POINT ( 'NONE',  ( -3.135527875058821579, 197.5041725223112223, 89.90113791807857524 ) ) ;
#23120 = ORIENTED_EDGE ( 'NONE', *, *, #227, .F. ) ;
#23121 = CARTESIAN_POINT ( 'NONE',  ( 80.37499999726881583, 155.0000000000000000, 15.58253174999999402 ) ) ;
#23122 = CARTESIAN_POINT ( 'NONE',  ( -4.903702542908436435, 200.1653181626580249, 50.04886208192144181 ) ) ;
#23123 = ORIENTED_EDGE ( 'NONE', *, *, #17707, .T. ) ;
#23124 = CARTESIAN_POINT ( 'NONE',  ( 73.12499999726881583, 155.0000000000000000, -15.58253175000000823 ) ) ;
#23125 = CARTESIAN_POINT ( 'NONE',  ( 0.000000000000000000, 0.000000000000000000, 0.000000000000000000 ) ) ;
#23126 = CARTESIAN_POINT ( 'NONE',  ( -56.51255670714900248, 194.9711358487265613, -1.525379346234926992 ) ) ;
#23127 = CARTESIAN_POINT ( 'NONE',  ( 64.72499999726881015, 140.1801316387863778, -4.815267126137194431 ) ) ;
#23128 = ADVANCED_FACE ( 'NONE', ( #4420 ), #24534, .T. ) ;
#23129 = CARTESIAN_POINT ( 'NONE',  ( -7.499999999999650058, -0.7583608255766450812, -7.446489218764574147 ) ) ;
#23130 = EDGE_CURVE ( 'NONE', #27498, #25537, #33082, .T. ) ;
#23131 = CARTESIAN_POINT ( 'NONE',  ( 10.00000000000000711, 207.0476921513415220, 48.99886208192143044 ) ) ;
#23132 = VERTEX_POINT ( 'NONE', #12088 ) ;
#23133 = DIRECTION ( 'NONE',  ( 1.000000000000000000, 0.000000000000000000, 0.000000000000000000 ) ) ;
#23134 =( NAMED_UNIT ( * ) PLANE_ANGLE_UNIT ( ) SI_UNIT ( $, .RADIAN. ) );
#23135 = CARTESIAN_POINT ( 'NONE',  ( 13.75000000000002487, 23.81569860407205397, 0.000000000000000000 ) ) ;
#23136 = CARTESIAN_POINT ( 'NONE',  ( 6.444103211790928043, 211.7408657792734061, 33.69886208192144039 ) ) ;
#23137 = EDGE_CURVE ( 'NONE', #31501, #18054, #2548, .T. ) ;
#23138 = CARTESIAN_POINT ( 'NONE',  ( 8.118202686958039038, 212.8392687619912635, 67.70113791807858661 ) ) ;
#23139 = DIRECTION ( 'NONE',  ( 4.625929269271484928E-16, 1.000000000000000000, -0.000000000000000000 ) ) ;
#23140 = EDGE_CURVE ( 'NONE', #17299, #210, #29189, .T. ) ;
#23141 = CARTESIAN_POINT ( 'NONE',  ( -6.139770520408369237, 215.5359834540460042, 54.95113791807856529 ) ) ;
#23142 = CARTESIAN_POINT ( 'NONE',  ( 10.00000000000000711, 206.9523078486586201, 26.00113791807856956 ) ) ;
#23143 = CARTESIAN_POINT ( 'NONE',  ( -8.015496119326531499, 204.4483345814780364, 9.351137918078563871 ) ) ;
#23144 = CARTESIAN_POINT ( 'NONE',  ( -6.663120783604270514, 3.846954578056913654, -6.460786012259833733 ) ) ;
#23145 = PLANE ( 'NONE',  #22000 ) ;
#23146 = CARTESIAN_POINT ( 'NONE',  ( 40.22499999726881015, 149.9369285172503510, 15.58253174999999580 ) ) ;
#23147 = CARTESIAN_POINT ( 'NONE',  ( -7.456977232089304408, 196.8216656703010301, 39.05113791807855961 ) ) ;
#23148 = LINE ( 'NONE', #20245, #29289 ) ;
#23149 = CARTESIAN_POINT ( 'NONE',  ( -10.00000000000000711, 207.0476921513413515, 87.50113791807858377 ) ) ;
#23150 = CARTESIAN_POINT ( 'NONE',  ( -0.05014649552810635652, 196.4853777576173002, 62.75113791807856956 ) ) ;
#23151 = DIRECTION ( 'NONE',  ( -1.000000000000000000, 0.000000000000000000, 0.000000000000000000 ) ) ;
#23152 = CARTESIAN_POINT ( 'NONE',  ( 12.00000000000000711, 207.0476921513415220, 27.99886208192144110 ) ) ;
#23153 = CARTESIAN_POINT ( 'NONE',  ( -8.118202686958138514, 212.8392687619910930, 29.79886208192143826 ) ) ;
#23154 = CARTESIAN_POINT ( 'NONE',  ( 75.69999999453764872, 142.6655632788954620, -8.961492836873480528 ) ) ;
#23155 = MANIFOLD_SOLID_BREP ( '\X2\00d8\X0\8.4 (8.4) Diameter Hole2', #12314 ) ;
#23156 = ORIENTED_EDGE ( 'NONE', *, *, #15365, .T. ) ;
#23157 = CARTESIAN_POINT ( 'NONE',  ( 7.456977232089302632, 217.1783343296989131, 67.55113791807856671 ) ) ;
#23158 = CARTESIAN_POINT ( 'NONE',  ( 8.000000000000008882, 206.9523078486586485, 83.00113791807856956 ) ) ;
#23159 = CARTESIAN_POINT ( 'NONE',  ( 3.135527875058981895, 197.5041725223112792, 37.59886208192143187 ) ) ;
#23160 = CARTESIAN_POINT ( 'NONE',  ( 70.71132485994280614, 155.0000000000000000, 15.00000000000001243 ) ) ;
#23161 = ORIENTED_EDGE ( 'NONE', *, *, #20920, .F. ) ;
#23162 = CARTESIAN_POINT ( 'NONE',  ( 12.00000000000000711, 207.0476921513415220, 42.99886208192143044 ) ) ;
#23163 = VERTEX_POINT ( 'NONE', #14139 ) ;
#23164 = ORIENTED_EDGE ( 'NONE', *, *, #23707, .F. ) ;
#23165 = CARTESIAN_POINT ( 'NONE',  ( 89.50000000000002842, 155.0000000000000000, -32.00000000000002842 ) ) ;
#23166 = CARTESIAN_POINT ( 'NONE',  ( -7.922281120364393914, 4.573931137438271399, -8.047472243342930653 ) ) ;
#23167 = VERTEX_POINT ( 'NONE', #19253 ) ;
#23168 = CARTESIAN_POINT ( 'NONE',  ( 7.984503880673485376, 204.3529502787953902, 44.15113791807857524 ) ) ;
#23169 = B_SPLINE_CURVE_WITH_KNOTS ( 'NONE', 3,
 ( #19090, #3759, #11429, #21806 ),
 .UNSPECIFIED., .F., .F.,
 ( 4, 4 ),
 ( 2.380739282171097332E-07, 0.002044882221487550125 ),
 .UNSPECIFIED. ) ;
#23170 = SURFACE_SIDE_STYLE ('',( #12779 ) ) ;
#23171 = CARTESIAN_POINT ( 'NONE',  ( -0.05014649552828403384, 217.5146222423826714, 21.24886208192143400 ) ) ;
#23172 = CARTESIAN_POINT ( 'NONE',  ( 62.37499999726880873, 155.0000000000000000, 15.58253174999999402 ) ) ;
#23173 = ORIENTED_EDGE ( 'NONE', *, *, #5202, .F. ) ;
#23174 = LINE ( 'NONE', #20779, #5830 ) ;
#23175 = CARTESIAN_POINT ( 'NONE',  ( -5.274401269815139237, -6.074457022762090652, -7.633824513837113912 ) ) ;
#23176 = CARTESIAN_POINT ( 'NONE',  ( 2.517493886309087436, 199.4062855549015865, 4.598862081921435419 ) ) ;
#23177 = CARTESIAN_POINT ( 'NONE',  ( 10.00000000000000711, 206.9523078486586201, 38.00113791807857666 ) ) ;
#23178 = CYLINDRICAL_SURFACE ( 'NONE', #29589, 15.00000000000001776 ) ;
#23179 = CARTESIAN_POINT ( 'NONE',  ( 3.044812012440130555, 197.4746971517856764, 23.60113791807857098 ) ) ;
#23180 = CARTESIAN_POINT ( 'NONE',  ( -9.662634960638639470, 203.2645104739510771, 104.3237470305089403 ) ) ;
#23181 = CARTESIAN_POINT ( 'NONE',  ( -0.05014649552828365914, 215.4116977939061144, 81.24886208192143044 ) ) ;
#23182 = CARTESIAN_POINT ( 'NONE',  ( 34.32499999726881157, 145.8408176439707802, 12.60653300113718345 ) ) ;
#23183 = LINE ( 'NONE', #23013, #5659 ) ;
#23184 = LINE ( 'NONE', #18074, #15332 ) ;
#23185 = CARTESIAN_POINT ( 'NONE',  ( -9.736236675707914401, 199.9851607334237542, 12.20113791807856707 ) ) ;
#23186 = DIRECTION ( 'NONE',  ( 1.000000000000000000, 0.000000000000000000, -0.000000000000000000 ) ) ;
#23187 = CARTESIAN_POINT ( 'NONE',  ( 51.17499999726880588, 145.8408176439707802, -12.60653300113719588 ) ) ;
#23188 = CARTESIAN_POINT ( 'NONE',  ( 10.01549611932653860, 210.2015048109876716, 58.85113791807856387 ) ) ;
#23189 = CIRCLE ( 'NONE', #7970, 4.000000000000000000 ) ;
#23190 = CARTESIAN_POINT ( 'NONE',  ( 0.000000000000000000, -0.8865213383406685965, 1.535500000000000531 ) ) ;
#23191 = CARTESIAN_POINT ( 'NONE',  ( 78.21132485994282035, 170.7719333635740497, -7.904646289410545231E-15 ) ) ;
#23192 = CARTESIAN_POINT ( 'NONE',  ( 65.21132485994280614, 139.2280666364260071, -4.041636747397287284E-15 ) ) ;
#23193 = CARTESIAN_POINT ( 'NONE',  ( 53.49999999453762456, 139.7537977485451393, -4.138211985947621020E-15 ) ) ;
#23194 = ORIENTED_EDGE ( 'NONE', *, *, #7734, .F. ) ;
#23195 = CARTESIAN_POINT ( 'NONE',  ( 7.456977232089302632, 217.1783343296989131, 40.55113791807856671 ) ) ;
#23196 = DIRECTION ( 'NONE',  ( 0.000000000000000000, 0.000000000000000000, -1.000000000000000000 ) ) ;
#23197 = CARTESIAN_POINT ( 'NONE',  ( -3.135527875058982783, 216.4958274776886924, 9.098862081921435419 ) ) ;
#23198 = CARTESIAN_POINT ( 'NONE',  ( 60.51132485994280330, 163.8167787843871110, 12.13525491562421621 ) ) ;
#23199 = ORIENTED_EDGE ( 'NONE', *, *, #12518, .F. ) ;
#23200 = CARTESIAN_POINT ( 'NONE',  ( -8.062137200540920645, 212.9164362838581894, 6.801137918078565825 ) ) ;
#23201 = CARTESIAN_POINT ( 'NONE',  ( 10.01549611932653860, 210.2015048109876716, 70.85113791807854966 ) ) ;
#23202 = B_SPLINE_CURVE_WITH_KNOTS ( 'NONE', 3,
 ( #14535, #24937, #22370, #23223, #31072, #62, #8226, #33618 ),
 .UNSPECIFIED., .F., .F.,
 ( 4, 2, 2, 4 ),
 ( 0.02832689070575898985, 0.03234239231761927569, 0.03635789392947955806, 0.04438889715320012280 ),
 .UNSPECIFIED. ) ;
#23203 = ORIENTED_EDGE ( 'NONE', *, *, #21211, .F. ) ;
#23204 = CARTESIAN_POINT ( 'NONE',  ( -8.015496119326597224, 209.5516654185217362, 35.64886208192143613 ) ) ;
#23205 = CARTESIAN_POINT ( 'NONE',  ( 80.48867513459481415, 142.2402378747194405, -9.270509831248439525 ) ) ;
#23206 = CARTESIAN_POINT ( 'NONE',  ( 77.17499999726881299, 145.8408176439707802, -12.60653300113719588 ) ) ;
#23207 = ORIENTED_EDGE ( 'NONE', *, *, #7291, .F. ) ;
#23208 = CARTESIAN_POINT ( 'NONE',  ( -6.500168698208129925, 202.3363017425936050, 12.20113791807856707 ) ) ;
#23209 = VECTOR ( 'NONE', #12807, 1000.000000000000000 ) ;
#23210 = CARTESIAN_POINT ( 'NONE',  ( -12.01549611932659722, 210.8513442034533227, 95.64886208192143613 ) ) ;
#23211 = CARTESIAN_POINT ( 'NONE',  ( 34.37499999726881583, 155.0000000000000000, 15.58253174999999402 ) ) ;
#23212 = ORIENTED_EDGE ( 'NONE', *, *, #6640, .F. ) ;
#23213 = CARTESIAN_POINT ( 'NONE',  ( 42.72499999726881015, 140.1801316387863778, -4.815267126137194431 ) ) ;
#23214 = CARTESIAN_POINT ( 'NONE',  ( -10.00000000000000711, 207.0476921513413515, 9.501137918078566003 ) ) ;
#23215 = CARTESIAN_POINT ( 'NONE',  ( -0.05014649552828403384, 217.5146222423826714, 75.24886208192144466 ) ) ;
#23216 = CARTESIAN_POINT ( 'NONE',  ( 48.77499999726880731, 140.1801316387863778, 4.815267126137185549 ) ) ;
#23217 = CARTESIAN_POINT ( 'NONE',  ( -67.50001199999998391, 137.9999999999999432, -1.112647398146382471 ) ) ;
#23218 = CARTESIAN_POINT ( 'NONE',  ( 8.062137200540920645, 201.0835637161417822, 14.30113791807856671 ) ) ;
#23219 = LINE ( 'NONE', #17950, #31211 ) ;
#23220 = VECTOR ( 'NONE', #9173, 1000.000000000000000 ) ;
#23221 = CARTESIAN_POINT ( 'NONE',  ( 69.09999999999999432, 168.7903194862797420, 4.480746418436729606 ) ) ;
#23222 = CARTESIAN_POINT ( 'NONE',  ( -3.135527875058821579, 197.5041725223112223, 101.9011379180785752 ) ) ;
#23223 = CARTESIAN_POINT ( 'NONE',  ( -27.50000000000000000, -10.64700562007355344, -1.134120025693880596 ) ) ;
#23224 = CARTESIAN_POINT ( 'NONE',  ( -3.044812012440131443, 216.5253028482142952, 79.10113791807857808 ) ) ;
#23225 = CARTESIAN_POINT ( 'NONE',  ( 3.500000000000004441, 0.3416723310689536164, -2.988332237913170807E-15 ) ) ;
#23226 = CARTESIAN_POINT ( 'NONE',  ( 99.99999999999998579, 0.000000000000000000, 4.171999999999999709 ) ) ;
#23227 = CARTESIAN_POINT ( 'NONE',  ( 11.98450388067341876, 210.9467285061363953, 99.84886208192143897 ) ) ;
#23228 = EDGE_CURVE ( 'NONE', #26026, #28157, #9026, .T. ) ;
#23229 = CARTESIAN_POINT ( 'NONE',  ( 69.32499999726881867, 164.1591823560292198, -12.60653300113719766 ) ) ;
#23230 = ORIENTED_EDGE ( 'NONE', *, *, #1394, .F. ) ;
#23231 = CARTESIAN_POINT ( 'NONE',  ( 43.41132485994280898, 142.2402378747194405, -9.270509831248439525 ) ) ;
#23232 = CARTESIAN_POINT ( 'NONE',  ( 87.77499999726882152, 169.8198683612136222, -4.815267126137197984 ) ) ;
#23233 = CARTESIAN_POINT ( 'NONE',  ( 9.736236675707914401, 214.0148392665762458, 94.70113791807858661 ) ) ;
#23234 = DIRECTION ( 'NONE',  ( 1.000000000000000000, 0.000000000000000000, 0.000000000000000000 ) ) ;
#23235 = AXIS2_PLACEMENT_3D ( 'NONE', #17708, #2041, #10392 ) ;
#23236 = EDGE_LOOP ( 'NONE', ( #17041, #19086, #12214, #1116, #15494, #20814 ) ) ;
#23237 = AXIS2_PLACEMENT_3D ( 'NONE', #13640, #29150, #10935 ) ;
#23238 = CARTESIAN_POINT ( 'NONE',  ( 8.118202686958138514, 201.1607312380088501, 88.29886208192142760 ) ) ;
#23239 = B_SPLINE_CURVE_WITH_KNOTS ( 'NONE', 3,
 ( #31800, #11363, #963, #26856, #6065, #21571, #26519, #16459, #3684 ),
 .UNSPECIFIED., .F., .F.,
 ( 4, 2, 1, 2, 4 ),
 ( 0.000000000000000000, 0.002165063509461097498, 0.004330127018922194995, 0.006495190528383292493, 0.008660254037844389990 ),
 .UNSPECIFIED. ) ;
#23240 = CARTESIAN_POINT ( 'NONE',  ( 7.456977232089471386, 196.8216656703012006, 19.44886208192143329 ) ) ;
#23241 = CARTESIAN_POINT ( 'NONE',  ( -1.604619215278546562E-14, -7.505553499465138501, -0.8000000000000003775 ) ) ;
#23242 = CARTESIAN_POINT ( 'NONE',  ( 8.118202686958039038, 212.8392687619912635, 43.70113791807857240 ) ) ;
#23243 = ORIENTED_EDGE ( 'NONE', *, *, #22026, .T. ) ;
#23244 = CARTESIAN_POINT ( 'NONE',  ( 8.015496119326595448, 204.4483345814782638, 4.148862081921435241 ) ) ;
#23245 = VECTOR ( 'NONE', #21028, 1000.000000000000000 ) ;
#23246 = CARTESIAN_POINT ( 'NONE',  ( 1.517883041479706208E-15, 4.041451884327390331, -0.3126073911696551910 ) ) ;
#23247 = ORIENTED_EDGE ( 'NONE', *, *, #19318, .F. ) ;
#23248 = CARTESIAN_POINT ( 'NONE',  ( -4.903702542908436435, 200.1653181626580249, 77.04886208192142760 ) ) ;
#23249 = ORIENTED_EDGE ( 'NONE', *, *, #22941, .F. ) ;
#23250 = CARTESIAN_POINT ( 'NONE',  ( -65.20000000000000284, -7.347880794884118356E-15, 19.29999999999998295 ) ) ;
#23251 = VERTEX_POINT ( 'NONE', #3908 ) ;
#23252 = DIRECTION ( 'NONE',  ( 0.000000000000000000, 0.000000000000000000, -1.000000000000000000 ) ) ;
#23253 = CARTESIAN_POINT ( 'NONE',  ( 0.05014649552807626948, 215.4116977939061144, 64.25113791807856956 ) ) ;
#23254 = CARTESIAN_POINT ( 'NONE',  ( 82.62499999726881583, 138.6155565068815463, -3.929120461958505118E-15 ) ) ;
#23255 = LINE ( 'NONE', #7600, #27925 ) ;
#23256 = CARTESIAN_POINT ( 'NONE',  ( 6.500168698208129925, 211.6636982574063381, 88.70113791807857240 ) ) ;
#23257 = CARTESIAN_POINT ( 'NONE',  ( -0.3755270751584372513, 206.3102596154024297, 117.9458888342408898 ) ) ;
#23258 = AXIS2_PLACEMENT_3D ( 'NONE', #12551, #22943, #4887 ) ;
#23259 = VECTOR ( 'NONE', #20573, 1000.000000000000114 ) ;
#23260 = CIRCLE ( 'NONE', #22644, 5.200000000000002842 ) ;
#23261 = CARTESIAN_POINT ( 'NONE',  ( 48.50000000000000000, 155.0000000000000000, -14.50000000000000711 ) ) ;
#23262 = CARTESIAN_POINT ( 'NONE',  ( -2.426778023690076225, 199.3768101843759553, 64.89886208192143613 ) ) ;
#23263 = EDGE_CURVE ( 'NONE', #6991, #546, #12428, .T. ) ;
#23264 = AXIS2_PLACEMENT_3D ( 'NONE', #32220, #19444, #720 ) ;
#23265 = CARTESIAN_POINT ( 'NONE',  ( 49.12499999726880873, 155.0000000000000000, -15.58253175000000823 ) ) ;
#23266 = CARTESIAN_POINT ( 'NONE',  ( 3.135527875058820690, 216.4958274776887492, 1.401137918078565914 ) ) ;
#23267 = DIRECTION ( 'NONE',  ( 0.000000000000000000, 1.000000000000000000, -1.478898702612462246E-15 ) ) ;
#23268 = CARTESIAN_POINT ( 'NONE',  ( 60.12499999726880873, 155.0000000000000000, 15.58253174999999402 ) ) ;
#23269 = CARTESIAN_POINT ( 'NONE',  ( 67.57499999726881867, 164.1591823560292198, -12.60653300113719766 ) ) ;
#23270 = CARTESIAN_POINT ( 'NONE',  ( -11.98450388067348804, 210.9467285061362247, 69.65113791807856103 ) ) ;
#23271 = FACE_OUTER_BOUND ( 'NONE', #25204, .T. ) ;
#23272 = CARTESIAN_POINT ( 'NONE',  ( -0.05014649552807705357, 194.3824533091408000, 5.751137918078564226 ) ) ;
#23273 = CARTESIAN_POINT ( 'NONE',  ( 9.984503880673473830, 203.7031108863295401, 83.15113791807856103 ) ) ;
#23274 = EDGE_CURVE ( 'NONE', #31983, #32748, #15491, .T. ) ;
#23275 = CARTESIAN_POINT ( 'NONE',  ( -11.98450388067341876, 203.0532714938636047, 53.34886208192144608 ) ) ;
#23276 = CARTESIAN_POINT ( 'NONE',  ( -8.118202686958138514, 212.8392687619910930, 53.79886208192143471 ) ) ;
#23277 = CARTESIAN_POINT ( 'NONE',  ( -3.295171437451516638, -7.213553046160524396, -7.590212325761481971 ) ) ;
#23278 = CARTESIAN_POINT ( 'NONE',  ( 12.00000000000000711, 206.9523078486586485, 92.00113791807858377 ) ) ;
#23279 =( BOUNDED_SURFACE ( )  B_SPLINE_SURFACE ( 1, 2, ( 
 ( #24636, #31793, #13728, #27016, #16621, #8789, #29409, #23963, #3511, #3846, #24127, #796, #32460, #1303, #29580, #13903, #11521, #626, #11693, #27190, #11185, #14238, #31957, #21564, #24287, #11024, #14068, #957, #13572, #26849, #29244, #3677, #5894, #29745, #19525, #3341, #21902, #8625, #21405, #8460, #19021, #24466, #16290, #32299, #22074, #26680, #16790, #9128, #11354, #19185, #29921, #6059, #21737, #32127, #6232, #8960, #19351, #16451, #6409, #6575, #26511, #3180, #30766, #9467, #17469, #20194, #11859, #22759, #19855, #4020, #9633, #15082, #22243, #4181, #27854, #7087, #32967, #30252, #14412, #27692, #28030, #14576, #24976, #22923, #25477, #20029, #4356, #1971, #24805, #2149, #17643, #1629, #4692, #22408, #12021, #14740, #1462, #12533, #32799, #25307, #20373, #6914, #17306, #14917, #33316, #17135, #16959, #30428, #9295, #25132, #12362, #27353, #9986, #1795, #4526, #32633, #33151, #12195, #22582, #19689, #9815, #30081, #6746, #27521, #30595, #7259, #17810, #12699, #5367, #18315, #4865, #15917, #422, #30940, #2982, #26315, #15254, #21033, #20876, #10496, #31275, #13200, #2657, #28708, #7935, #10152, #15754, #7603, #18486, #25647, #25821, #26150, #2485, #20535, #28869, #21198, #28208, #5527, #12867, #7425, #23261, #18157, #13362, #2314, #17986, #2817, #28378, #5035, #10659, #23600, #265, #15425, #13040, #7766, #33655, #10332, #23431, #20704, #31434, #28552, #33484, #23095, #8104, #95, #23757, #10824, #31104, #5198, #15583, #25986, #32092, #11154, #32255, #19313, #31593, #13864, #26973, #11654, #24086, #5855, #3143, #21862, #16254, #3471, #29376, #29702, #1259, #754, #31757, #6360, #18986, #13531, #6021, #21528, #3302, #23922, #8259, #8754, #31917, #16412, #27154, #8589, #26807, #24250, #29203, #29538, #917, #24598, #8424, #26640, #16755, #8922, #19142, #587, #10982, #11316, #21701, #14201, #6194, #3636, #24429, #1092, #18810, #16583, #14032, #18649, #11484, #29040, #3811, #5693, #16082, #13686, #26474, #21360, #30387, #1933, #14534, #32932, #30217, #7215, #22369, #9085, #4483, #17431, #27651, #20155, #15043, #4318, #12322, #22548, #9592, #19822, #19653, #6873, #17602, #22716, #32420, #7050, #11816, #27993, #24936, #17101, #9772, #25435, #1593, #22205, #30552, #9430, #3978, #17261, #11983, #27486, #27315, #2111, #19986, #32758, #14703, #4659, #25095, #1755, #12154, #30043, #27815, #14874, #22037, #32594, #6709, #19483, #33106, #25268, #14377, #24768, #29884, #6538, #16918, #1424, #9260, #4141, #15718, #12657, #13004, #5162, #15882, #31235, #12495, #20673, #5326, #60, #7566, #18279, #13165, #20832, #26117, #4997, #23396, #31070, #31396, #12829, #33276, #28668, #7898, #18114, #10623, #5493, #28512, #2785, #10457, #23559, #10297, #10118, #7728, #8064, #229, #22884, #20998, #2273, #18450, #15385, #17952, #28837, #26277, #9943, #20329, #30900, #30729, #28342, #23221, #7389, #17770, #23055, #28166, #33447, #20499, #4826, #15217, #25608, #25781, #15549, #33616, #2449, #25942, #2616, #16212, #16374, #13654, #29000, #18613, #19109, #31882, #29498, #3431, #23720, #21825, #6152, #16546, #13828, #26603, #3600, #24390, #2948, #18942, #32056, #16714, #29165, #10947, #8224, #26941, #21322, #8549, #716, #29339, #1057, #29669, #5986, #13994, #24218, #882, #11119, #554, #21495, #32216, #11446, #13329, #11278, #26438, #8881, #5817, #31719, #19277, #383, #10785, #6321, #8391, #21160, #18778, #24047, #31557, #5660, #3103, #21661, #3266, #8718, #16048, #13491, #23886, #26766, #17393, #12280, #4102, #19782, #9728, #6667, #14494, #32719, #24892, #25062, #1552, #30006, #9553, #14334, #27779, #30177, #7176, #19615, #27607, #30344, #22001, #32893, #17054, #14164, #6834, #25230, #32384, #24731, #4274, #17220, #9386, #27448, #24558, #11950, #4443, #1385, #11773, #33059, #1893, #14667, #22332, #12115, #1214, #22672, #14831, #22163, #20118, #32550, #9225, #1715, #11611, #30511, #22506, #19945, #27115, #7007, #3777, #9048, #19440, #27278, #29843, #6503, #16881, #3935, #12963, #20961, #2750, #7524, #10255, #15004, #23358, #15176, #17909, #28631, #20460, #10583, #26080, #31354, #30691, #18072, #27953, #22845, #15512, #28467, #25394, #13124, #17560, #7354, #23517, #185, #2066, #31191, #4622, #10083, #17734, #15679, #4957, #33237, #15344, #30860, #23012, #9903, #12453, #5124, #28302 ),
 ( #20285, #25735, #21, #28122, #4783, #2406, #20631, #25569, #10418, #2233, #12792, #5286, #23182, #12617, #33409, #33576, #31031, #25904, #7689, #2576, #20790, #7857, #18242, #16503, #1010, #31520, #3560, #26902, #5456, #21616, #21457, #11076, #31839, #13784, #3226, #29292, #8504, #10742, #18897, #8190, #19066, #15843, #26401, #16334, #3060, #21123, #5943, #16168, #28800, #8350, #340, #26728, #18575, #11229, #11405, #28960, #3389, #8023, #13449, #23843, #18739, #24180, #26232, #841, #29455, #5617, #32011, #13950, #29125, #674, #24341, #21286, #5772, #13614, #26557, #8674, #24010, #10909, #6106, #16009, #21783, #18408, #2903, #516, #13289, #23680, #31680, #4229, #24687, #19236, #24848, #30298, #3730, #19398, #32676, #22294, #14453, #1346, #29631, #14119, #14627, #27402, #25023, #9342, #6278, #17355, #1676, #12069, #19737, #11733, #32849, #19899, #32174, #1512, #27563, #12238, #22120, #6460, #24513, #22457, #16841, #4064, #29965, #6966, #1848, #32511, #32345, #27740, #19572, #1171, #6623, #9183, #3889, #11567, #8834, #30133, #17008, #11909, #4403, #6791, #17179, #9512, #29799, #14788, #25180, #16671, #9009, #27235, #27068, #21955, #14284, #28381, #25825, #26154, #28715, #5696, #7938, #28874, #15921, #26319, #23265, #23603, #15759, #26478, #8108, #22624, #31278, #2985, #10662, #18160, #5530, #23760, #31441, #13365, #15588, #268, #18320, #8263, #23434, #9683, #426, #18491, #5371, #21203, #16085, #2820, #10828, #21037, #31598, #20879, #20707, #13204, #18653, #29043, #33012, #3147, #12872, #20077, #25991, #28555, #30472, #7134, #17518, #5039, #7770, #15428, #5203, #98, #2489, #33660, #10336, #31108, #2661, #13044, #10501, #11489, #6369, #3306, #8757, #13868, #8593, #758, #19146, #26813, #26978, #24253, #5859, #921, #29207, #11320, #3475, #18989, #18813, #27320, #14037, #21704, #32095, #9092, #29544, #6198, #16586, #11157, #21867, #3642, #6543, #13690, #31922, #11659, #14206, #1098, #16257, #26643, #24434, #32261, #29889, #8928, #19319, #16761, #27159, #24091, #29708, #3815, #16925, #24603, #13534, #1266, #22043, #32426, #29379, #19489, #23928, #591, #10986, #6024, #21365, #31760, #8427, #21532, #16416, #20163, #33114, #9601, #2120, #30737, #19994, #28000, #4491, #25275, #1762, #1599, #12163, #22891, #4666, #14383, #12329, #27491, #9950, #6879, #32764, #15050, #17777, #24773, #12502, #22375, #3986, #9438, #14709, #33283, #14883, #7222, #25444, #9265, #11990, #17613, #1940, #30560, #4146, #32940, #4325, #19828, #24942, #30395, #17268, #17438, #25102, #30048, #19658, #20338, #7056, #7396, #22726, #1429, #11823, #22211, #32600, #9779, #27658, #6716, #17106, #14541, #27821, #30224, #22555, #20680, #2456, #33454, #18458, #12837, #67, #25950, #15889, #31564, #31078, #28350, #26283, #20840, #8232, #13172, #28176, #2626, #21005, #15727, #23229, #238, #28845, #2792, #8073, #7736, #5335, #13012, #13336, #28520, #15225, #10630, #23569, #10466, #2957, #21169, #31243, #5500, #28675, #26124, #23404, #25791, #7905, #23727, #390, #4835, #31403, #17960, #10794, #18121, #33625, #25614, #2280, #12664, #23062, #10304, #10126, #5169, #15555, #20506, #30909, #7574, #5004, #15392, #18286, #21832, #16554, #11453, #8399, #13836, #18952, #13661, #5825, #24225, #31889, #32065, #29346, #10954, #561, #1065, #888, #32223, #19115, #5668, #3785, #8888, #19284, #29505, #8557, #29676, #6330, #18620, #11285, #14001, #32391, #11127, #26610, #23894, #16721, #3273, #21672, #16381, #27124, #22008, #21502, #18786, #14172, #5993, #21330, #26773, #3438, #24054, #31726, #29007, #6159, #8725, #26949, #24565, #3608, #24400, #1222, #16220, #11620, #16057, #26446, #29175, #725, #3110, #13500, #30351, #14342, #11782, #12122, #14674, #25402, #27614, #14838, #1902, #12288, #9232, #9560, #19622, #27454, #7183, #9736, #7014, #24738, #22170, #22514, #25068, #2073, #4284, #25237, #22681, #33067, #30013, #19954, #1722, #12461, #27786, #9055, #17228, #20124, #17400, #4108, #30518, #17567, #4450, #27960, #1561, #4629, #32902, #15013, #9394, #29852, #22852, #19448, #6510, #16889, #27287, #3942, #1392, #32560, #6675, #6841, #17062, #14501, #24899, #11956, #22339, #32726, #19791, #30185, #2413, #28309, #10592, #13297, #20292, #31363, #17918, #33244, #4965, #10263, #18416, #30, #2756, #194, #4791, #30869 ) ),
 .UNSPECIFIED., .F., .F., .T. ) 
 B_SPLINE_SURFACE_WITH_KNOTS ( ( 2, 2 ),
 ( 3, 2, 2, 2, 2, 2, 2, 2, 2, 2, 2, 2, 2, 2, 2, 2, 2, 2, 2, 2, 2, 2, 2, 2, 2, 2, 2, 2, 2, 2, 2, 2, 2, 2, 2, 2, 2, 2, 2, 2, 2, 2, 2, 2, 2, 2, 2, 2, 2, 2, 2, 2, 2, 2, 2, 2, 2, 2, 2, 2, 2, 2, 2, 2, 2, 2, 2, 2, 2, 2, 2, 2, 2, 2, 2, 2, 2, 2, 2, 2, 2, 2, 2, 2, 2, 2, 2, 2, 2, 2, 2, 2, 2, 2, 2, 2, 2, 2, 2, 2, 2, 2, 2, 2, 2, 2, 2, 2, 2, 2, 2, 2, 2, 2, 2, 2, 2, 2, 2, 2, 2, 2, 2, 2, 2, 2, 2, 2, 2, 2, 2, 2, 2, 2, 2, 2, 2, 2, 2, 2, 2, 2, 2, 2, 2, 2, 2, 2, 2, 2, 2, 2, 2, 2, 2, 2, 2, 2, 2, 2, 2, 2, 2, 2, 2, 2, 2, 2, 2, 2, 2, 2, 2, 2, 2, 2, 2, 2, 2, 2, 2, 2, 2, 2, 2, 2, 2, 2, 2, 2, 2, 2, 2, 2, 2, 2, 2, 2, 2, 2, 2, 2, 2, 2, 2, 2, 2, 2, 2, 2, 2, 2, 2, 2, 2, 2, 2, 2, 2, 2, 2, 2, 2, 2, 2, 2, 2, 2, 2, 2, 2, 2, 2, 2, 2, 2, 2, 2, 2, 2, 2, 2, 2, 2, 2, 2, 2, 2, 2, 2, 2, 2, 2, 2, 2, 2, 2, 2, 2, 2, 2, 2, 2, 2, 2, 2, 2, 2, 2, 2, 2, 2, 2, 2, 2, 3 ),
 ( 0.000000000000000000, 1.000000000000000000 ),
 ( 0.000000000000000000, 0.003571428571428571317, 0.007142857142857142634, 0.01071428571428571438, 0.01428571428571428527, 0.01785714285714285615, 0.02142857142857142877, 0.02500000000000000139, 0.02857142857142857054, 0.03214285714285713969, 0.03571428571428571230, 0.03928571428571428492, 0.04285714285714285754, 0.04642857142857143016, 0.05000000000000000278, 0.05357142857142856845, 0.05714285714285714107, 0.06071428571428571369, 0.06428571428571427937, 0.06785714285714285199, 0.07142857142857142461, 0.07499999999999999722, 0.07857142857142856984, 0.08214285714285714246, 0.08571428571428571508, 0.08928571428571428770, 0.09285714285714286031, 0.09642857142857143293, 0.1000000000000000056, 0.1035714285714285782, 0.1071428571428571369, 0.1107142857142857095, 0.1142857142857142821, 0.1178571428571428548, 0.1214285714285714274, 0.1250000000000000000, 0.1285714285714285587, 0.1321428571428571452, 0.1357142857142857040, 0.1392857142857142905, 0.1428571428571428492, 0.1464285714285714357, 0.1499999999999999944, 0.1535714285714285809, 0.1571428571428571397, 0.1607142857142857262, 0.1642857142857142849, 0.1678571428571428437, 0.1714285714285714302, 0.1749999999999999889, 0.1785714285714285754, 0.1821428571428571341, 0.1857142857142857206, 0.1892857142857142794, 0.1928571428571428659, 0.1964285714285714246, 0.2000000000000000111, 0.2035714285714285698, 0.2071428571428571563, 0.2107142857142857151, 0.2142857142857142738, 0.2178571428571428603, 0.2214285714285714191, 0.2250000000000000056, 0.2285714285714285643, 0.2321428571428571508, 0.2357142857142857095, 0.2392857142857142960, 0.2428571428571428548, 0.2464285714285714413, 0.2500000000000000000, 0.2535714285714285587, 0.2571428571428571175, 0.2607142857142857317, 0.2642857142857142905, 0.2678571428571428492, 0.2714285714285714080, 0.2750000000000000222, 0.2785714285714285809, 0.2821428571428571397, 0.2857142857142856984, 0.2892857142857143127, 0.2928571428571428714, 0.2964285714285714302, 0.2999999999999999889, 0.3035714285714285476, 0.3071428571428571619, 0.3107142857142857206, 0.3142857142857142794, 0.3178571428571428381, 0.3214285714285714524, 0.3250000000000000111, 0.3285714285714285698, 0.3321428571428571286, 0.3357142857142856873, 0.3392857142857143016, 0.3428571428571428603, 0.3464285714285714191, 0.3499999999999999778, 0.3535714285714285920, 0.3571428571428571508, 0.3607142857142857095, 0.3642857142857142683, 0.3678571428571428825, 0.3714285714285714413, 0.3750000000000000000, 0.3785714285714285587, 0.3821428571428571175, 0.3857142857142857317, 0.3892857142857142905, 0.3928571428571428492, 0.3964285714285714080, 0.4000000000000000222, 0.4035714285714285809, 0.4071428571428571397, 0.4107142857142856984, 0.4142857142857143127, 0.4178571428571428714, 0.4214285714285714302, 0.4249999999999999889, 0.4285714285714285476, 0.4321428571428571619, 0.4357142857142857206, 0.4392857142857142794, 0.4428571428571428381, 0.4464285714285714524, 0.4500000000000000111, 0.4535714285714285698, 0.4571428571428571286, 0.4607142857142856873, 0.4642857142857143016, 0.4678571428571428603, 0.4714285714285714191, 0.4749999999999999778, 0.4785714285714285920, 0.4821428571428571508, 0.4857142857142857095, 0.4892857142857142683, 0.4928571428571428825, 0.4964285714285714413, 0.5000000000000000000, 0.5035714285714285587, 0.5071428571428571175, 0.5107142857142856762, 0.5142857142857142350, 0.5178571428571429047, 0.5214285714285714635, 0.5250000000000000222, 0.5285714285714285809, 0.5321428571428571397, 0.5357142857142856984, 0.5392857142857142572, 0.5428571428571428159, 0.5464285714285713746, 0.5500000000000000444, 0.5535714285714286031, 0.5571428571428571619, 0.5607142857142857206, 0.5642857142857142794, 0.5678571428571428381, 0.5714285714285713969, 0.5749999999999999556, 0.5785714285714286254, 0.5821428571428571841, 0.5857142857142857428, 0.5892857142857143016, 0.5928571428571428603, 0.5964285714285714191, 0.5999999999999999778, 0.6035714285714285365, 0.6071428571428570953, 0.6107142857142857650, 0.6142857142857143238, 0.6178571428571428825, 0.6214285714285714413, 0.6250000000000000000, 0.6285714285714285587, 0.6321428571428571175, 0.6357142857142856762, 0.6392857142857142350, 0.6428571428571429047, 0.6464285714285714635, 0.6500000000000000222, 0.6535714285714285809, 0.6571428571428571397, 0.6607142857142856984, 0.6642857142857142572, 0.6678571428571428159, 0.6714285714285713746, 0.6750000000000000444, 0.6785714285714286031, 0.6821428571428571619, 0.6857142857142857206, 0.6892857142857142794, 0.6928571428571428381, 0.6964285714285713969, 0.6999999999999999556, 0.7035714285714286254, 0.7071428571428571841, 0.7107142857142857428, 0.7142857142857143016, 0.7178571428571428603, 0.7214285714285714191, 0.7249999999999999778, 0.7285714285714285365, 0.7321428571428570953, 0.7357142857142857650, 0.7392857142857143238, 0.7428571428571428825, 0.7464285714285714413, 0.7500000000000000000, 0.7535714285714285587, 0.7571428571428571175, 0.7607142857142856762, 0.7642857142857142350, 0.7678571428571429047, 0.7714285714285714635, 0.7750000000000000222, 0.7785714285714285809, 0.7821428571428571397, 0.7857142857142856984, 0.7892857142857142572, 0.7928571428571428159, 0.7964285714285713746, 0.8000000000000000444, 0.8035714285714286031, 0.8071428571428571619, 0.8107142857142857206, 0.8142857142857142794, 0.8178571428571428381, 0.8214285714285713969, 0.8249999999999999556, 0.8285714285714286254, 0.8321428571428571841, 0.8357142857142857428, 0.8392857142857143016, 0.8428571428571428603, 0.8464285714285714191, 0.8499999999999999778, 0.8535714285714285365, 0.8571428571428570953, 0.8607142857142857650, 0.8642857142857143238, 0.8678571428571428825, 0.8714285714285714413, 0.8750000000000000000, 0.8785714285714285587, 0.8821428571428571175, 0.8857142857142856762, 0.8892857142857142350, 0.8928571428571429047, 0.8964285714285714635, 0.9000000000000000222, 0.9035714285714285809, 0.9071428571428571397, 0.9107142857142856984, 0.9142857142857142572, 0.9178571428571428159, 0.9214285714285713746, 0.9250000000000000444, 0.9285714285714286031, 0.9321428571428571619, 0.9357142857142857206, 0.9392857142857142794, 0.9428571428571428381, 0.9464285714285713969, 0.9499999999999999556, 0.9535714285714286254, 0.9571428571428571841, 0.9607142857142857428, 0.9642857142857143016, 0.9678571428571428603, 0.9714285714285714191, 0.9749999999999999778, 0.9785714285714285365, 0.9821428571428570953 ),
 .UNSPECIFIED. ) 
 GEOMETRIC_REPRESENTATION_ITEM ( )  RATIONAL_B_SPLINE_SURFACE ( (
 ( 1.000000000000000000, 0.9510565162951535312, 1.000000000000000000, 0.9510565162951535312, 1.000000000000000000, 0.9510565162951535312, 1.000000000000000000, 0.9510565162951535312, 1.000000000000000000, 0.9510565162951535312, 1.000000000000000000, 0.9510565162951535312, 1.000000000000000000, 0.9510565162951535312, 1.000000000000000000, 0.9510565162951535312, 1.000000000000000000, 0.9510565162951535312, 1.000000000000000000, 0.9510565162951535312, 1.000000000000000000, 0.9510565162951535312, 1.000000000000000000, 0.9510565162951535312, 1.000000000000000000, 0.9510565162951535312, 1.000000000000000000, 0.9510565162951535312, 1.000000000000000000, 0.9510565162951535312, 1.000000000000000000, 0.9510565162951535312, 1.000000000000000000, 0.9510565162951535312, 1.000000000000000000, 0.9510565162951535312, 1.000000000000000000, 0.9510565162951535312, 1.000000000000000000, 0.9510565162951535312, 1.000000000000000000, 0.9510565162951535312, 1.000000000000000000, 0.9510565162951535312, 1.000000000000000000, 0.9510565162951535312, 1.000000000000000000, 0.9510565162951535312, 1.000000000000000000, 0.9510565162951535312, 1.000000000000000000, 0.9510565162951535312, 1.000000000000000000, 0.9510565162951535312, 1.000000000000000000, 0.9510565162951535312, 1.000000000000000000, 0.9510565162951535312, 1.000000000000000000, 0.9510565162951535312, 1.000000000000000000, 0.9510565162951535312, 1.000000000000000000, 0.9510565162951535312, 1.000000000000000000, 0.9510565162951535312, 1.000000000000000000, 0.9510565162951535312, 1.000000000000000000, 0.9510565162951535312, 1.000000000000000000, 0.9510565162951535312, 1.000000000000000000, 0.9510565162951535312, 1.000000000000000000, 0.9510565162951535312, 1.000000000000000000, 0.9510565162951535312, 1.000000000000000000, 0.9510565162951535312, 1.000000000000000000, 0.9510565162951535312, 1.000000000000000000, 0.9510565162951535312, 1.000000000000000000, 0.9510565162951535312, 1.000000000000000000, 0.9510565162951535312, 1.000000000000000000, 0.9510565162951535312, 1.000000000000000000, 0.9510565162951535312, 1.000000000000000000, 0.9510565162951535312, 1.000000000000000000, 0.9510565162951535312, 1.000000000000000000, 0.9510565162951535312, 1.000000000000000000, 0.9510565162951535312, 1.000000000000000000, 0.9510565162951535312, 1.000000000000000000, 0.9510565162951535312, 1.000000000000000000, 0.9510565162951535312, 1.000000000000000000, 0.9510565162951535312, 1.000000000000000000, 0.9510565162951535312, 1.000000000000000000, 0.9510565162951535312, 1.000000000000000000, 0.9510565162951535312, 1.000000000000000000, 0.9510565162951535312, 1.000000000000000000, 0.9510565162951535312, 1.000000000000000000, 0.9510565162951535312, 1.000000000000000000, 0.9510565162951535312, 1.000000000000000000, 0.9510565162951535312, 1.000000000000000000, 0.9510565162951535312, 1.000000000000000000, 0.9510565162951535312, 1.000000000000000000, 0.9510565162951535312, 1.000000000000000000, 0.9510565162951535312, 1.000000000000000000, 0.9510565162951535312, 1.000000000000000000, 0.9510565162951535312, 1.000000000000000000, 0.9510565162951535312, 1.000000000000000000, 0.9510565162951535312, 1.000000000000000000, 0.9510565162951535312, 1.000000000000000000, 0.9510565162951535312, 1.000000000000000000, 0.9510565162951535312, 1.000000000000000000, 0.9510565162951535312, 1.000000000000000000, 0.9510565162951535312, 1.000000000000000000, 0.9510565162951535312, 1.000000000000000000, 0.9510565162951535312, 1.000000000000000000, 0.9510565162951535312, 1.000000000000000000, 0.9510565162951535312, 1.000000000000000000, 0.9510565162951535312, 1.000000000000000000, 0.9510565162951535312, 1.000000000000000000, 0.9510565162951535312, 1.000000000000000000, 0.9510565162951535312, 1.000000000000000000, 0.9510565162951535312, 1.000000000000000000, 0.9510565162951535312, 1.000000000000000000, 0.9510565162951535312, 1.000000000000000000, 0.9510565162951535312, 1.000000000000000000, 0.9510565162951535312, 1.000000000000000000, 0.9510565162951535312, 1.000000000000000000, 0.9510565162951535312, 1.000000000000000000, 0.9510565162951535312, 1.000000000000000000, 0.9510565162951535312, 1.000000000000000000, 0.9510565162951535312, 1.000000000000000000, 0.9510565162951535312, 1.000000000000000000, 0.9510565162951535312, 1.000000000000000000, 0.9510565162951535312, 1.000000000000000000, 0.9510565162951535312, 1.000000000000000000, 0.9510565162951535312, 1.000000000000000000, 0.9510565162951535312, 1.000000000000000000, 0.9510565162951535312, 1.000000000000000000, 0.9510565162951535312, 1.000000000000000000, 0.9510565162951535312, 1.000000000000000000, 0.9510565162951535312, 1.000000000000000000, 0.9510565162951535312, 1.000000000000000000, 0.9510565162951535312, 1.000000000000000000, 0.9510565162951535312, 1.000000000000000000, 0.9510565162951535312, 1.000000000000000000, 0.9510565162951535312, 1.000000000000000000, 0.9510565162951535312, 1.000000000000000000, 0.9510565162951535312, 1.000000000000000000, 0.9510565162951535312, 1.000000000000000000, 0.9510565162951535312, 1.000000000000000000, 0.9510565162951535312, 1.000000000000000000, 0.9510565162951535312, 1.000000000000000000, 0.9510565162951535312, 1.000000000000000000, 0.9510565162951535312, 1.000000000000000000, 0.9510565162951535312, 1.000000000000000000, 0.9510565162951535312, 1.000000000000000000, 0.9510565162951535312, 1.000000000000000000, 0.9510565162951535312, 1.000000000000000000, 0.9510565162951535312, 1.000000000000000000, 0.9510565162951535312, 1.000000000000000000, 0.9510565162951535312, 1.000000000000000000, 0.9510565162951535312, 1.000000000000000000, 0.9510565162951535312, 1.000000000000000000, 0.9510565162951535312, 1.000000000000000000, 0.9510565162951535312, 1.000000000000000000, 0.9510565162951535312, 1.000000000000000000, 0.9510565162951535312, 1.000000000000000000, 0.9510565162951535312, 1.000000000000000000, 0.9510565162951535312, 1.000000000000000000, 0.9510565162951535312, 1.000000000000000000, 0.9510565162951535312, 1.000000000000000000, 0.9510565162951535312, 1.000000000000000000, 0.9510565162951535312, 1.000000000000000000, 0.9510565162951535312, 1.000000000000000000, 0.9510565162951535312, 1.000000000000000000, 0.9510565162951535312, 1.000000000000000000, 0.9510565162951535312, 1.000000000000000000, 0.9510565162951535312, 1.000000000000000000, 0.9510565162951535312, 1.000000000000000000, 0.9510565162951535312, 1.000000000000000000, 0.9510565162951535312, 1.000000000000000000, 0.9510565162951535312, 1.000000000000000000, 0.9510565162951535312, 1.000000000000000000, 0.9510565162951535312, 1.000000000000000000, 0.9510565162951535312, 1.000000000000000000, 0.9510565162951535312, 1.000000000000000000, 0.9510565162951535312, 1.000000000000000000, 0.9510565162951535312, 1.000000000000000000, 0.9510565162951535312, 1.000000000000000000, 0.9510565162951535312, 1.000000000000000000, 0.9510565162951535312, 1.000000000000000000, 0.9510565162951535312, 1.000000000000000000, 0.9510565162951535312, 1.000000000000000000, 0.9510565162951535312, 1.000000000000000000, 0.9510565162951535312, 1.000000000000000000, 0.9510565162951535312, 1.000000000000000000, 0.9510565162951535312, 1.000000000000000000, 0.9510565162951535312, 1.000000000000000000, 0.9510565162951535312, 1.000000000000000000, 0.9510565162951535312, 1.000000000000000000, 0.9510565162951535312, 1.000000000000000000, 0.9510565162951535312, 1.000000000000000000, 0.9510565162951535312, 1.000000000000000000, 0.9510565162951535312, 1.000000000000000000, 0.9510565162951535312, 1.000000000000000000, 0.9510565162951535312, 1.000000000000000000, 0.9510565162951535312, 1.000000000000000000, 0.9510565162951535312, 1.000000000000000000, 0.9510565162951535312, 1.000000000000000000, 0.9510565162951535312, 1.000000000000000000, 0.9510565162951535312, 1.000000000000000000, 0.9510565162951535312, 1.000000000000000000, 0.9510565162951535312, 1.000000000000000000, 0.9510565162951535312, 1.000000000000000000, 0.9510565162951535312, 1.000000000000000000, 0.9510565162951535312, 1.000000000000000000, 0.9510565162951535312, 1.000000000000000000, 0.9510565162951535312, 1.000000000000000000, 0.9510565162951535312, 1.000000000000000000, 0.9510565162951535312, 1.000000000000000000, 0.9510565162951535312, 1.000000000000000000, 0.9510565162951535312, 1.000000000000000000, 0.9510565162951535312, 1.000000000000000000, 0.9510565162951535312, 1.000000000000000000, 0.9510565162951535312, 1.000000000000000000, 0.9510565162951535312, 1.000000000000000000, 0.9510565162951535312, 1.000000000000000000, 0.9510565162951535312, 1.000000000000000000, 0.9510565162951535312, 1.000000000000000000, 0.9510565162951535312, 1.000000000000000000, 0.9510565162951535312, 1.000000000000000000, 0.9510565162951535312, 1.000000000000000000, 0.9510565162951535312, 1.000000000000000000, 0.9510565162951535312, 1.000000000000000000, 0.9510565162951535312, 1.000000000000000000, 0.9510565162951535312, 1.000000000000000000, 0.9510565162951535312, 1.000000000000000000, 0.9510565162951535312, 1.000000000000000000, 0.9510565162951535312, 1.000000000000000000, 0.9510565162951535312, 1.000000000000000000, 0.9510565162951535312, 1.000000000000000000, 0.9510565162951535312, 1.000000000000000000, 0.9510565162951535312, 1.000000000000000000, 0.9510565162951535312, 1.000000000000000000, 0.9510565162951535312, 1.000000000000000000, 0.9510565162951535312, 1.000000000000000000, 0.9510565162951535312, 1.000000000000000000, 0.9510565162951535312, 1.000000000000000000, 0.9510565162951535312, 1.000000000000000000, 0.9510565162951535312, 1.000000000000000000, 0.9510565162951535312, 1.000000000000000000, 0.9510565162951535312, 1.000000000000000000, 0.9510565162951535312, 1.000000000000000000, 0.9510565162951535312, 1.000000000000000000, 0.9510565162951535312, 1.000000000000000000, 0.9510565162951535312, 1.000000000000000000, 0.9510565162951535312, 1.000000000000000000, 0.9510565162951535312, 1.000000000000000000, 0.9510565162951535312, 1.000000000000000000, 0.9510565162951535312, 1.000000000000000000, 0.9510565162951535312, 1.000000000000000000, 0.9510565162951535312, 1.000000000000000000, 0.9510565162951535312, 1.000000000000000000, 0.9510565162951535312, 1.000000000000000000, 0.9510565162951535312, 1.000000000000000000, 0.9510565162951535312, 1.000000000000000000, 0.9510565162951535312, 1.000000000000000000, 0.9510565162951535312, 1.000000000000000000, 0.9510565162951535312, 1.000000000000000000, 0.9510565162951535312, 1.000000000000000000, 0.9510565162951535312, 1.000000000000000000, 0.9510565162951535312, 1.000000000000000000, 0.9510565162951535312, 1.000000000000000000, 0.9510565162951535312, 1.000000000000000000, 0.9510565162951535312, 1.000000000000000000, 0.9510565162951535312, 1.000000000000000000, 0.9510565162951535312, 1.000000000000000000, 0.9510565162951535312, 1.000000000000000000, 0.9510565162951535312, 1.000000000000000000, 0.9510565162951535312, 1.000000000000000000, 0.9510565162951535312, 1.000000000000000000, 0.9510565162951535312, 1.000000000000000000, 0.9510565162951535312, 1.000000000000000000, 0.9510565162951535312, 1.000000000000000000, 0.9510565162951535312, 1.000000000000000000, 0.9510565162951535312, 1.000000000000000000, 0.9510565162951535312, 1.000000000000000000, 0.9510565162951535312, 1.000000000000000000, 0.9510565162951535312, 1.000000000000000000, 0.9510565162951535312, 1.000000000000000000, 0.9510565162951535312, 1.000000000000000000, 0.9510565162951535312, 1.000000000000000000, 0.9510565162951535312, 1.000000000000000000, 0.9510565162951535312, 1.000000000000000000, 0.9510565162951535312, 1.000000000000000000, 0.9510565162951535312, 1.000000000000000000, 0.9510565162951535312, 1.000000000000000000, 0.9510565162951535312, 1.000000000000000000, 0.9510565162951535312, 1.000000000000000000, 0.9510565162951535312, 1.000000000000000000, 0.9510565162951535312, 1.000000000000000000, 0.9510565162951535312, 1.000000000000000000, 0.9510565162951535312, 1.000000000000000000, 0.9510565162951535312, 1.000000000000000000, 0.9510565162951535312, 1.000000000000000000, 0.9510565162951535312, 1.000000000000000000, 0.9510565162951535312, 1.000000000000000000, 0.9510565162951535312, 1.000000000000000000, 0.9510565162951535312, 1.000000000000000000, 0.9510565162951535312, 1.000000000000000000, 0.9510565162951535312, 1.000000000000000000, 0.9510565162951535312, 1.000000000000000000, 0.9510565162951535312, 1.000000000000000000),
 ( 1.000000000000000000, 0.9510565162951535312, 1.000000000000000000, 0.9510565162951535312, 1.000000000000000000, 0.9510565162951535312, 1.000000000000000000, 0.9510565162951535312, 1.000000000000000000, 0.9510565162951535312, 1.000000000000000000, 0.9510565162951535312, 1.000000000000000000, 0.9510565162951535312, 1.000000000000000000, 0.9510565162951535312, 1.000000000000000000, 0.9510565162951535312, 1.000000000000000000, 0.9510565162951535312, 1.000000000000000000, 0.9510565162951535312, 1.000000000000000000, 0.9510565162951535312, 1.000000000000000000, 0.9510565162951535312, 1.000000000000000000, 0.9510565162951535312, 1.000000000000000000, 0.9510565162951535312, 1.000000000000000000, 0.9510565162951535312, 1.000000000000000000, 0.9510565162951535312, 1.000000000000000000, 0.9510565162951535312, 1.000000000000000000, 0.9510565162951535312, 1.000000000000000000, 0.9510565162951535312, 1.000000000000000000, 0.9510565162951535312, 1.000000000000000000, 0.9510565162951535312, 1.000000000000000000, 0.9510565162951535312, 1.000000000000000000, 0.9510565162951535312, 1.000000000000000000, 0.9510565162951535312, 1.000000000000000000, 0.9510565162951535312, 1.000000000000000000, 0.9510565162951535312, 1.000000000000000000, 0.9510565162951535312, 1.000000000000000000, 0.9510565162951535312, 1.000000000000000000, 0.9510565162951535312, 1.000000000000000000, 0.9510565162951535312, 1.000000000000000000, 0.9510565162951535312, 1.000000000000000000, 0.9510565162951535312, 1.000000000000000000, 0.9510565162951535312, 1.000000000000000000, 0.9510565162951535312, 1.000000000000000000, 0.9510565162951535312, 1.000000000000000000, 0.9510565162951535312, 1.000000000000000000, 0.9510565162951535312, 1.000000000000000000, 0.9510565162951535312, 1.000000000000000000, 0.9510565162951535312, 1.000000000000000000, 0.9510565162951535312, 1.000000000000000000, 0.9510565162951535312, 1.000000000000000000, 0.9510565162951535312, 1.000000000000000000, 0.9510565162951535312, 1.000000000000000000, 0.9510565162951535312, 1.000000000000000000, 0.9510565162951535312, 1.000000000000000000, 0.9510565162951535312, 1.000000000000000000, 0.9510565162951535312, 1.000000000000000000, 0.9510565162951535312, 1.000000000000000000, 0.9510565162951535312, 1.000000000000000000, 0.9510565162951535312, 1.000000000000000000, 0.9510565162951535312, 1.000000000000000000, 0.9510565162951535312, 1.000000000000000000, 0.9510565162951535312, 1.000000000000000000, 0.9510565162951535312, 1.000000000000000000, 0.9510565162951535312, 1.000000000000000000, 0.9510565162951535312, 1.000000000000000000, 0.9510565162951535312, 1.000000000000000000, 0.9510565162951535312, 1.000000000000000000, 0.9510565162951535312, 1.000000000000000000, 0.9510565162951535312, 1.000000000000000000, 0.9510565162951535312, 1.000000000000000000, 0.9510565162951535312, 1.000000000000000000, 0.9510565162951535312, 1.000000000000000000, 0.9510565162951535312, 1.000000000000000000, 0.9510565162951535312, 1.000000000000000000, 0.9510565162951535312, 1.000000000000000000, 0.9510565162951535312, 1.000000000000000000, 0.9510565162951535312, 1.000000000000000000, 0.9510565162951535312, 1.000000000000000000, 0.9510565162951535312, 1.000000000000000000, 0.9510565162951535312, 1.000000000000000000, 0.9510565162951535312, 1.000000000000000000, 0.9510565162951535312, 1.000000000000000000, 0.9510565162951535312, 1.000000000000000000, 0.9510565162951535312, 1.000000000000000000, 0.9510565162951535312, 1.000000000000000000, 0.9510565162951535312, 1.000000000000000000, 0.9510565162951535312, 1.000000000000000000, 0.9510565162951535312, 1.000000000000000000, 0.9510565162951535312, 1.000000000000000000, 0.9510565162951535312, 1.000000000000000000, 0.9510565162951535312, 1.000000000000000000, 0.9510565162951535312, 1.000000000000000000, 0.9510565162951535312, 1.000000000000000000, 0.9510565162951535312, 1.000000000000000000, 0.9510565162951535312, 1.000000000000000000, 0.9510565162951535312, 1.000000000000000000, 0.9510565162951535312, 1.000000000000000000, 0.9510565162951535312, 1.000000000000000000, 0.9510565162951535312, 1.000000000000000000, 0.9510565162951535312, 1.000000000000000000, 0.9510565162951535312, 1.000000000000000000, 0.9510565162951535312, 1.000000000000000000, 0.9510565162951535312, 1.000000000000000000, 0.9510565162951535312, 1.000000000000000000, 0.9510565162951535312, 1.000000000000000000, 0.9510565162951535312, 1.000000000000000000, 0.9510565162951535312, 1.000000000000000000, 0.9510565162951535312, 1.000000000000000000, 0.9510565162951535312, 1.000000000000000000, 0.9510565162951535312, 1.000000000000000000, 0.9510565162951535312, 1.000000000000000000, 0.9510565162951535312, 1.000000000000000000, 0.9510565162951535312, 1.000000000000000000, 0.9510565162951535312, 1.000000000000000000, 0.9510565162951535312, 1.000000000000000000, 0.9510565162951535312, 1.000000000000000000, 0.9510565162951535312, 1.000000000000000000, 0.9510565162951535312, 1.000000000000000000, 0.9510565162951535312, 1.000000000000000000, 0.9510565162951535312, 1.000000000000000000, 0.9510565162951535312, 1.000000000000000000, 0.9510565162951535312, 1.000000000000000000, 0.9510565162951535312, 1.000000000000000000, 0.9510565162951535312, 1.000000000000000000, 0.9510565162951535312, 1.000000000000000000, 0.9510565162951535312, 1.000000000000000000, 0.9510565162951535312, 1.000000000000000000, 0.9510565162951535312, 1.000000000000000000, 0.9510565162951535312, 1.000000000000000000, 0.9510565162951535312, 1.000000000000000000, 0.9510565162951535312, 1.000000000000000000, 0.9510565162951535312, 1.000000000000000000, 0.9510565162951535312, 1.000000000000000000, 0.9510565162951535312, 1.000000000000000000, 0.9510565162951535312, 1.000000000000000000, 0.9510565162951535312, 1.000000000000000000, 0.9510565162951535312, 1.000000000000000000, 0.9510565162951535312, 1.000000000000000000, 0.9510565162951535312, 1.000000000000000000, 0.9510565162951535312, 1.000000000000000000, 0.9510565162951535312, 1.000000000000000000, 0.9510565162951535312, 1.000000000000000000, 0.9510565162951535312, 1.000000000000000000, 0.9510565162951535312, 1.000000000000000000, 0.9510565162951535312, 1.000000000000000000, 0.9510565162951535312, 1.000000000000000000, 0.9510565162951535312, 1.000000000000000000, 0.9510565162951535312, 1.000000000000000000, 0.9510565162951535312, 1.000000000000000000, 0.9510565162951535312, 1.000000000000000000, 0.9510565162951535312, 1.000000000000000000, 0.9510565162951535312, 1.000000000000000000, 0.9510565162951535312, 1.000000000000000000, 0.9510565162951535312, 1.000000000000000000, 0.9510565162951535312, 1.000000000000000000, 0.9510565162951535312, 1.000000000000000000, 0.9510565162951535312, 1.000000000000000000, 0.9510565162951535312, 1.000000000000000000, 0.9510565162951535312, 1.000000000000000000, 0.9510565162951535312, 1.000000000000000000, 0.9510565162951535312, 1.000000000000000000, 0.9510565162951535312, 1.000000000000000000, 0.9510565162951535312, 1.000000000000000000, 0.9510565162951535312, 1.000000000000000000, 0.9510565162951535312, 1.000000000000000000, 0.9510565162951535312, 1.000000000000000000, 0.9510565162951535312, 1.000000000000000000, 0.9510565162951535312, 1.000000000000000000, 0.9510565162951535312, 1.000000000000000000, 0.9510565162951535312, 1.000000000000000000, 0.9510565162951535312, 1.000000000000000000, 0.9510565162951535312, 1.000000000000000000, 0.9510565162951535312, 1.000000000000000000, 0.9510565162951535312, 1.000000000000000000, 0.9510565162951535312, 1.000000000000000000, 0.9510565162951535312, 1.000000000000000000, 0.9510565162951535312, 1.000000000000000000, 0.9510565162951535312, 1.000000000000000000, 0.9510565162951535312, 1.000000000000000000, 0.9510565162951535312, 1.000000000000000000, 0.9510565162951535312, 1.000000000000000000, 0.9510565162951535312, 1.000000000000000000, 0.9510565162951535312, 1.000000000000000000, 0.9510565162951535312, 1.000000000000000000, 0.9510565162951535312, 1.000000000000000000, 0.9510565162951535312, 1.000000000000000000, 0.9510565162951535312, 1.000000000000000000, 0.9510565162951535312, 1.000000000000000000, 0.9510565162951535312, 1.000000000000000000, 0.9510565162951535312, 1.000000000000000000, 0.9510565162951535312, 1.000000000000000000, 0.9510565162951535312, 1.000000000000000000, 0.9510565162951535312, 1.000000000000000000, 0.9510565162951535312, 1.000000000000000000, 0.9510565162951535312, 1.000000000000000000, 0.9510565162951535312, 1.000000000000000000, 0.9510565162951535312, 1.000000000000000000, 0.9510565162951535312, 1.000000000000000000, 0.9510565162951535312, 1.000000000000000000, 0.9510565162951535312, 1.000000000000000000, 0.9510565162951535312, 1.000000000000000000, 0.9510565162951535312, 1.000000000000000000, 0.9510565162951535312, 1.000000000000000000, 0.9510565162951535312, 1.000000000000000000, 0.9510565162951535312, 1.000000000000000000, 0.9510565162951535312, 1.000000000000000000, 0.9510565162951535312, 1.000000000000000000, 0.9510565162951535312, 1.000000000000000000, 0.9510565162951535312, 1.000000000000000000, 0.9510565162951535312, 1.000000000000000000, 0.9510565162951535312, 1.000000000000000000, 0.9510565162951535312, 1.000000000000000000, 0.9510565162951535312, 1.000000000000000000, 0.9510565162951535312, 1.000000000000000000, 0.9510565162951535312, 1.000000000000000000, 0.9510565162951535312, 1.000000000000000000, 0.9510565162951535312, 1.000000000000000000, 0.9510565162951535312, 1.000000000000000000, 0.9510565162951535312, 1.000000000000000000, 0.9510565162951535312, 1.000000000000000000, 0.9510565162951535312, 1.000000000000000000, 0.9510565162951535312, 1.000000000000000000, 0.9510565162951535312, 1.000000000000000000, 0.9510565162951535312, 1.000000000000000000, 0.9510565162951535312, 1.000000000000000000, 0.9510565162951535312, 1.000000000000000000, 0.9510565162951535312, 1.000000000000000000, 0.9510565162951535312, 1.000000000000000000, 0.9510565162951535312, 1.000000000000000000, 0.9510565162951535312, 1.000000000000000000, 0.9510565162951535312, 1.000000000000000000, 0.9510565162951535312, 1.000000000000000000, 0.9510565162951535312, 1.000000000000000000, 0.9510565162951535312, 1.000000000000000000, 0.9510565162951535312, 1.000000000000000000, 0.9510565162951535312, 1.000000000000000000, 0.9510565162951535312, 1.000000000000000000, 0.9510565162951535312, 1.000000000000000000, 0.9510565162951535312, 1.000000000000000000, 0.9510565162951535312, 1.000000000000000000, 0.9510565162951535312, 1.000000000000000000, 0.9510565162951535312, 1.000000000000000000, 0.9510565162951535312, 1.000000000000000000, 0.9510565162951535312, 1.000000000000000000, 0.9510565162951535312, 1.000000000000000000, 0.9510565162951535312, 1.000000000000000000, 0.9510565162951535312, 1.000000000000000000, 0.9510565162951535312, 1.000000000000000000, 0.9510565162951535312, 1.000000000000000000, 0.9510565162951535312, 1.000000000000000000, 0.9510565162951535312, 1.000000000000000000, 0.9510565162951535312, 1.000000000000000000, 0.9510565162951535312, 1.000000000000000000, 0.9510565162951535312, 1.000000000000000000, 0.9510565162951535312, 1.000000000000000000, 0.9510565162951535312, 1.000000000000000000, 0.9510565162951535312, 1.000000000000000000, 0.9510565162951535312, 1.000000000000000000, 0.9510565162951535312, 1.000000000000000000, 0.9510565162951535312, 1.000000000000000000, 0.9510565162951535312, 1.000000000000000000, 0.9510565162951535312, 1.000000000000000000, 0.9510565162951535312, 1.000000000000000000, 0.9510565162951535312, 1.000000000000000000, 0.9510565162951535312, 1.000000000000000000, 0.9510565162951535312, 1.000000000000000000, 0.9510565162951535312, 1.000000000000000000, 0.9510565162951535312, 1.000000000000000000, 0.9510565162951535312, 1.000000000000000000, 0.9510565162951535312, 1.000000000000000000, 0.9510565162951535312, 1.000000000000000000, 0.9510565162951535312, 1.000000000000000000, 0.9510565162951535312, 1.000000000000000000, 0.9510565162951535312, 1.000000000000000000, 0.9510565162951535312, 1.000000000000000000, 0.9510565162951535312, 1.000000000000000000, 0.9510565162951535312, 1.000000000000000000, 0.9510565162951535312, 1.000000000000000000, 0.9510565162951535312, 1.000000000000000000, 0.9510565162951535312, 1.000000000000000000, 0.9510565162951535312, 1.000000000000000000, 0.9510565162951535312, 1.000000000000000000, 0.9510565162951535312, 1.000000000000000000) ) ) 
 REPRESENTATION_ITEM ( '' )  SURFACE ( )  );
#23280 = CARTESIAN_POINT ( 'NONE',  ( -67.50001199999999812, 171.1317437780265607, 5.477666192157153446 ) ) ;
#23281 = VECTOR ( 'NONE', #29786, 1000.000000000000000 ) ;
#23282 = CARTESIAN_POINT ( 'NONE',  ( -10.01549611932653860, 203.7984951890123284, 9.351137918078569200 ) ) ;
#23283 = CARTESIAN_POINT ( 'NONE',  ( -10.00000000000000711, 206.9523078486584495, 65.49886208192143044 ) ) ;
#23284 = AXIS2_PLACEMENT_3D ( 'NONE', #9207, #19597, #7155 ) ;
#23285 = ORIENTED_EDGE ( 'NONE', *, *, #32696, .T. ) ;
#23286 = CARTESIAN_POINT ( 'NONE',  ( -12.00000000000000711, 206.9523078486584780, 77.49886208192144466 ) ) ;
#23287 = CARTESIAN_POINT ( 'NONE',  ( 8.118202686958039038, 212.8392687619912635, 91.70113791807857240 ) ) ;
#23288 = VERTEX_POINT ( 'NONE', #30663 ) ;
#23289 = CARTESIAN_POINT ( 'NONE',  ( 78.57499999726881867, 145.8408176439707802, 12.60653300113718345 ) ) ;
#23290 = CARTESIAN_POINT ( 'NONE',  ( -7.984503880673422316, 204.3529502787951628, 47.34886208192143897 ) ) ;
#23291 = EDGE_LOOP ( 'NONE', ( #18632, #5191, #24761, #15667 ) ) ;
#23292 = EDGE_CURVE ( 'NONE', #23387, #22231, #16700, .T. ) ;
#23293 = CARTESIAN_POINT ( 'NONE',  ( 73.22499999726881015, 160.0630714827496206, -15.58253175000000823 ) ) ;
#23294 = CARTESIAN_POINT ( 'NONE',  ( 6.500000000000000888, 2.723353699433710862, -5.896365680526115760 ) ) ;
#23295 = CARTESIAN_POINT ( 'NONE',  ( 60.00000000000000000, 7.347880794884118356E-15, 20.00000000000000000 ) ) ;
#23296 = ADVANCED_FACE ( 'NONE', ( #33032 ), #18868, .F. ) ;
#23297 = CARTESIAN_POINT ( 'NONE',  ( 62.02499999726880020, 160.0630714827496206, 15.58253174999999402 ) ) ;
#23298 = CARTESIAN_POINT ( 'NONE',  ( 0.000000000000000000, 0.000000000000000000, 0.000000000000000000 ) ) ;
#23299 = CARTESIAN_POINT ( 'NONE',  ( 6.220909254589681581, 198.5229672870052582, 52.44886208192143329 ) ) ;
#23300 = EDGE_LOOP ( 'NONE', ( #5804, #23156 ) ) ;
#23301 = CARTESIAN_POINT ( 'NONE',  ( 19.55945325266599966, 20.46160920480081202, -17.55088044235633760 ) ) ;
#23302 = LINE ( 'NONE', #27148, #16456 ) ;
#23303 = CARTESIAN_POINT ( 'NONE',  ( -8.015496119326597224, 209.5516654185217362, 32.64886208192144323 ) ) ;
#23304 = AXIS2_PLACEMENT_3D ( 'NONE', #23915, #3135, #579 ) ;
#23305 = CARTESIAN_POINT ( 'NONE',  ( -3.135527875058821579, 197.5041725223112223, 68.90113791807857524 ) ) ;
#23306 = CARTESIAN_POINT ( 'NONE',  ( 127.5000000000000000, 155.0000000000000000, -6.938893903907228378E-15 ) ) ;
#23307 = CARTESIAN_POINT ( 'NONE',  ( 6.220909254589536808, 215.4770327129947702, 55.55113791807855961 ) ) ;
#23308 = AXIS2_PLACEMENT_3D ( 'NONE', #2214, #7837, #15156 ) ;
#23309 = ITEM_DEFINED_TRANSFORMATION ( 'NONE', 'NONE', #15384,  #2404 ) ;
#23310 = CARTESIAN_POINT ( 'NONE',  ( -0.05014649552810635652, 196.4853777576173002, 29.75113791807856956 ) ) ;
#23311 = CARTESIAN_POINT ( 'NONE',  ( 8.015496119326531499, 209.5516654185219636, 16.85113791807856742 ) ) ;
#23312 = CARTESIAN_POINT ( 'NONE',  ( 125.5000000000000000, 229.9533188057749555, 74.95331880577313655 ) ) ;
#23313 = CARTESIAN_POINT ( 'NONE',  ( -31.74999999999995737, 0.000000000000000000, 5.000000000000001776 ) ) ;
#23314 = CARTESIAN_POINT ( 'NONE',  ( 39.72499999726881015, 169.8198683612136222, 4.815267126137181997 ) ) ;
#23315 = CARTESIAN_POINT ( 'NONE',  ( 11.98450388067348271, 203.0532714938637753, 41.15113791807857524 ) ) ;
#23316 = CARTESIAN_POINT ( 'NONE',  ( -5.913191805370921372, 206.1729016772225123, -5.405163435505806468 ) ) ;
#23317 = CARTESIAN_POINT ( 'NONE',  ( 10.00000000000000711, 206.9523078486586201, 89.00113791807858377 ) ) ;
#23318 = CARTESIAN_POINT ( 'NONE',  ( -6.220909254589537696, 198.5229672870051445, 60.05113791807856671 ) ) ;
#23319 = AXIS2_PLACEMENT_3D ( 'NONE', #23440, #25997, #9997 ) ;
#23320 = CARTESIAN_POINT ( 'NONE',  ( 75.78867513459483973, 155.0000000000000000, 15.00000000000001243 ) ) ;
#23321 = CARTESIAN_POINT ( 'NONE',  ( 3.753561863808876797, 195.6020594897209719, 22.59886208192143542 ) ) ;
#23322 = CARTESIAN_POINT ( 'NONE',  ( -8.118202686958138514, 212.8392687619910930, 32.79886208192143471 ) ) ;
#23323 = CARTESIAN_POINT ( 'NONE',  ( 70.69999999453764872, 167.3344367211045096, 8.961492836873468093 ) ) ;
#23324 = CARTESIAN_POINT ( 'NONE',  ( -3.753561863808691168, 195.6020594897209435, 71.90113791807856103 ) ) ;
#23325 = CARTESIAN_POINT ( 'NONE',  ( 2.426778023690261410, 199.3768101843759837, 86.60113791807857808 ) ) ;
#23326 = ADVANCED_FACE ( 'NONE', ( #28276 ), #31411, .T. ) ;
#23327 = CARTESIAN_POINT ( 'NONE',  ( 10.00000000000000711, 207.0476921513415220, 42.99886208192143044 ) ) ;
#23328 = EDGE_CURVE ( 'NONE', #320, #13463, #28608, .T. ) ;
#23329 = CARTESIAN_POINT ( 'NONE',  ( -9.826550578524280155, 207.8102407865004011, 102.5369383530249223 ) ) ;
#23330 = ORIENTED_EDGE ( 'NONE', *, *, #28229, .T. ) ;
#23331 = CARTESIAN_POINT ( 'NONE',  ( 7.456977232089471386, 196.8216656703012006, 52.44886208192144039 ) ) ;
#23332 = EDGE_LOOP ( 'NONE', ( #23496, #10310, #30320, #786 ) ) ;
#23333 = PRODUCT_RELATED_PRODUCT_CATEGORY ( 'part', '', ( #33103 ) ) ;
#23334 = VERTEX_POINT ( 'NONE', #20765 ) ;
#23335 = EDGE_CURVE ( 'NONE', #28735, #9574, #9803, .T. ) ;
#23336 = TOROIDAL_SURFACE ( 'NONE', #17340, 9.624472924841564136, 1.000000000000000444 ) ;
#23337 = CARTESIAN_POINT ( 'NONE',  ( 6.818272094961329799, 1.321852500971154365, -6.208027553811807486 ) ) ;
#23338 = AXIS2_PLACEMENT_3D ( 'NONE', #9041, #16539, #32378 ) ;
#23339 = FACE_OUTER_BOUND ( 'NONE', #6120, .T. ) ;
#23340 = VERTEX_POINT ( 'NONE', #33384 ) ;
#23341 = CARTESIAN_POINT ( 'NONE',  ( -4.984841277089726574, 200.2242689037092305, 45.05113791807857382 ) ) ;
#23342 = ADVANCED_FACE ( 'NONE', ( #12256 ), #12769, .F. ) ;
#23343 = CARTESIAN_POINT ( 'NONE',  ( 2.000000000000000000, 2.449293598294706414E-16, -2.874600000000001376 ) ) ;
#23344 = CARTESIAN_POINT ( 'NONE',  ( -3.044812012439970683, 197.4746971517856196, 25.89886208192143613 ) ) ;
#23345 = CARTESIAN_POINT ( 'NONE',  ( 61.17499999726882010, 145.8408176439707802, -12.60653300113719588 ) ) ;
#23347 = ORIENTED_EDGE ( 'NONE', *, *, #16605, .T. ) ;
#23346 = AXIS2_PLACEMENT_3D ( 'NONE', #33571, #7685, #26228 ) ;
#23348 = CARTESIAN_POINT ( 'NONE',  ( 7.499999999999999112, -4.330127018922205195, -1.000000000000000888 ) ) ;
#23349 =( LENGTH_UNIT ( ) NAMED_UNIT ( * ) SI_UNIT ( .MILLI., .METRE. ) );
#23350 = DIRECTION ( 'NONE',  ( 1.000000000000000000, 0.000000000000000000, 0.000000000000000000 ) ) ;
#23351 = CARTESIAN_POINT ( 'NONE',  ( -4.984841277089891776, 213.7757310962905990, 5.948862081921435063 ) ) ;
#23352 = CARTESIAN_POINT ( 'NONE',  ( 6.139770520408368348, 198.4640165459539674, 38.45113791807855819 ) ) ;
#23353 = CARTESIAN_POINT ( 'NONE',  ( 79.71132485994280614, 155.0000000000000000, -15.00000000000002487 ) ) ;
#23354 = CARTESIAN_POINT ( 'NONE',  ( -8.062137200540920645, 212.9164362838581894, 27.80113791807856671 ) ) ;
#23355 = CARTESIAN_POINT ( 'NONE',  ( 117.5000000000000000, 102.0000000000001990, 93.94869280115064214 ) ) ;
#23356 = CARTESIAN_POINT ( 'NONE',  ( 60.00000000000001421, 6.938893903907228378E-15, -45.00000000000000711 ) ) ;
#23357 = CARTESIAN_POINT ( 'NONE',  ( -4.984841277089891776, 213.7757310962905990, 92.94886208192144750 ) ) ;
#23358 = CARTESIAN_POINT ( 'NONE',  ( 84.10000000000000853, 141.2096805137202580, -4.480746418436742040 ) ) ;
#23359 = CARTESIAN_POINT ( 'NONE',  ( -6.293430271071534854, 5.026740376715094882, -0.4524126574264483169 ) ) ;
#23360 = CARTESIAN_POINT ( 'NONE',  ( -63.49999999999884892, 215.0000000000003979, 0.000000000000000000 ) ) ;
#23361 = CARTESIAN_POINT ( 'NONE',  ( -0.05014649552807705357, 194.3824533091408000, 11.75113791807856600 ) ) ;
#23362 = FACE_OUTER_BOUND ( 'NONE', #24078, .T. ) ;
#23363 = CARTESIAN_POINT ( 'NONE',  ( 57.27499999726882152, 149.9369285172503510, -15.58253175000000823 ) ) ;
#23364 = CARTESIAN_POINT ( 'NONE',  ( -3.044812012440131443, 216.5253028482142952, 61.10113791807857098 ) ) ;
#23365 = EDGE_CURVE ( 'NONE', #29025, #1664, #7830, .T. ) ;
#23366 = CARTESIAN_POINT ( 'NONE',  ( -63.50000000000004263, 215.0000000000000000, -2.500000000000000000 ) ) ;
#23367 = LINE ( 'NONE', #17920, #17387 ) ;
#23368 = EDGE_CURVE ( 'NONE', #14989, #18434, #6334, .T. ) ;
#23369 = CARTESIAN_POINT ( 'NONE',  ( -7.500000000000000000, 4.330127018922191873, -10.00000000000000000 ) ) ;
#23370 = CARTESIAN_POINT ( 'NONE',  ( 56.79999999453762882, 163.5228861582408797, 11.73074641843673049 ) ) ;
#23371 = ORIENTED_EDGE ( 'NONE', *, *, #20818, .F. ) ;
#23372 = CARTESIAN_POINT ( 'NONE',  ( 0.05014649552807549926, 219.6175466908591716, 40.25113791807856245 ) ) ;
#23373 = CARTESIAN_POINT ( 'NONE',  ( 34.50000000000000000, -103.0000000000000142, 30.00000000000000000 ) ) ;
#23374 = CARTESIAN_POINT ( 'NONE',  ( 0.05014649552828275708, 196.4853777576173002, 10.74886208192143755 ) ) ;
#23375 = FACE_OUTER_BOUND ( 'NONE', #7624, .T. ) ;
#23376 = EDGE_LOOP ( 'NONE', ( #1542, #18719, #25332, #5353 ) ) ;
#23377 = CARTESIAN_POINT ( 'NONE',  ( -6.139770520408369237, 215.5359834540460042, 9.951137918078567068 ) ) ;
#23378 = CARTESIAN_POINT ( 'NONE',  ( -9.984503880673473830, 210.2968891136704315, 66.65113791807857524 ) ) ;
#23379 = VERTEX_POINT ( 'NONE', #23160 ) ;
#23380 = CARTESIAN_POINT ( 'NONE',  ( -0.05014649552828365914, 215.4116977939061144, 30.24886208192143755 ) ) ;
#23381 = FACE_OUTER_BOUND ( 'NONE', #28859, .T. ) ;
#23382 = VERTEX_POINT ( 'NONE', #20094 ) ;
#23383 = CARTESIAN_POINT ( 'NONE',  ( 4.984841277089725686, 213.7757310962907411, 10.55113791807856671 ) ) ;
#23384 = CIRCLE ( 'NONE', #11943, 27.50000000000000355 ) ;
#23385 = CARTESIAN_POINT ( 'NONE',  ( -9.680171189290716072, 199.9079932115567146, 95.19886208192144750 ) ) ;
#23386 = CARTESIAN_POINT ( 'NONE',  ( 42.07499999726881157, 168.2552932293087906, 9.630534252274372875 ) ) ;
#23387 = VERTEX_POINT ( 'NONE', #25543 ) ;
#23388 = CARTESIAN_POINT ( 'NONE',  ( 51.92499999726880588, 164.1591823560292198, 12.60653300113718167 ) ) ;
#23389 = CARTESIAN_POINT ( 'NONE',  ( -64.96121601855533356, 1.809269760319432319, 19.53878398144468775 ) ) ;
#23390 = CARTESIAN_POINT ( 'NONE',  ( -3.044812012440131443, 216.5253028482142952, 4.101137918078565647 ) ) ;
#23391 = CARTESIAN_POINT ( 'NONE',  ( -10.00000000000000711, 206.9523078486584495, 77.49886208192144466 ) ) ;
#23392 = CARTESIAN_POINT ( 'NONE',  ( 56.47499999726881015, 149.9369285172503510, 15.58253174999999580 ) ) ;
#23393 = CARTESIAN_POINT ( 'NONE',  ( -68.50000000000000000, 215.0000000000000000, -2.500000000000000000 ) ) ;
#23394 = CARTESIAN_POINT ( 'NONE',  ( 0.05014649552810505201, 217.5146222423826714, 10.25113791807856778 ) ) ;
#23395 = CARTESIAN_POINT ( 'NONE',  ( 15.61000000000001364, 0.000000000000000000, 0.000000000000000000 ) ) ;
#23396 = CARTESIAN_POINT ( 'NONE',  ( 65.90000000000000568, 141.2096805137202580, 4.480746418436733158 ) ) ;
#23397 =( BOUNDED_CURVE ( )  B_SPLINE_CURVE ( 2, ( #28190, #15238, #30749, #24958, #6730, #2133, #12516, #25289, #19841, #22905, #12004 ),
 .UNSPECIFIED., .F., .T. ) 
 B_SPLINE_CURVE_WITH_KNOTS ( ( 3, 2, 2, 2, 2, 3 ),
 ( 0.3749999999999997780, 0.3785714285714283367, 0.3821428571428569509, 0.3857142857142855097, 0.3892857142857141239, 0.3928571428571426827 ),
 .UNSPECIFIED. ) 
 CURVE ( )  GEOMETRIC_REPRESENTATION_ITEM ( )  RATIONAL_B_SPLINE_CURVE ( ( 1.000000000000003109, 0.9510565162951504226, 1.000000000000000000, 0.9510565162951534202, 1.000000000000000000, 0.9510565162951534202, 1.000000000000000000, 0.9510565162951534202, 1.000000000000000000, 0.9510565162951549745, 0.9999999999999984457 ) ) 
 REPRESENTATION_ITEM ( '' )  );
#23398 = CARTESIAN_POINT ( 'NONE',  ( -9.949154985843399857, 217.7087784572769067, 102.9933096652613074 ) ) ;
#23399 = CARTESIAN_POINT ( 'NONE',  ( 18.40782811468575275, 21.12650028821923343, -0.2827231011780743652 ) ) ;
#23400 = CARTESIAN_POINT ( 'NONE',  ( -9.984503880673473830, 210.2968891136704315, 87.65113791807854682 ) ) ;
#23401 = CARTESIAN_POINT ( 'NONE',  ( 3.500000000000004885, 2.020725942163702715, -0.3126073911696551910 ) ) ;
#23402 = FACE_OUTER_BOUND ( 'NONE', #8494, .T. ) ;
#23403 = CARTESIAN_POINT ( 'NONE',  ( 3.753561863808876797, 195.6020594897209719, 97.59886208192145318 ) ) ;
#23404 = CARTESIAN_POINT ( 'NONE',  ( 71.32499999726881867, 164.1591823560292198, -12.60653300113719766 ) ) ;
#23405 = VERTEX_POINT ( 'NONE', #18217 ) ;
#23406 = CARTESIAN_POINT ( 'NONE',  ( -60.48814638060569848, 194.9711715815534205, -1.524404325634890700 ) ) ;
#23407 = CARTESIAN_POINT ( 'NONE',  ( 87.07499999726880446, 141.7447067706911810, -9.630534252274385310 ) ) ;
#23408 = CARTESIAN_POINT ( 'NONE',  ( 3.662846001190051659, 195.5725841191953691, 95.60113791807857808 ) ) ;
#23409 = CARTESIAN_POINT ( 'NONE',  ( -31.74999999999995737, 0.000000000000000000, 3.500000000000000000 ) ) ;
#23410 = ORIENTED_EDGE ( 'NONE', *, *, #32504, .T. ) ;
#23411 = CARTESIAN_POINT ( 'NONE',  ( -6.220909254589682469, 215.4770327129947134, 86.94886208192141908 ) ) ;
#23412 = CARTESIAN_POINT ( 'NONE',  ( -7.375838497908014268, 196.7627149292498530, 23.04886208192143826 ) ) ;
#23413 = CARTESIAN_POINT ( 'NONE',  ( 77.50000000000000000, 155.0000000000000000, -6.938893903907228378E-15 ) ) ;
#23414 = CARTESIAN_POINT ( 'NONE',  ( -8.062137200540920645, 212.9164362838581894, 39.80113791807857382 ) ) ;
#23415 = ORIENTED_EDGE ( 'NONE', *, *, #6166, .T. ) ;
#23416 = CARTESIAN_POINT ( 'NONE',  ( 2.517493886309087436, 199.4062855549015865, 7.598862081921434530 ) ) ;
#23417 = DIRECTION ( 'NONE',  ( 0.000000000000000000, -1.000000000000000000, 1.222984857324291014E-15 ) ) ;
#23418 = ORIENTED_EDGE ( 'NONE', *, *, #5625, .T. ) ;
#23419 = CARTESIAN_POINT ( 'NONE',  ( 4.984841277089891776, 200.2242689037093726, 91.44886208192143329 ) ) ;
#23420 = VERTEX_POINT ( 'NONE', #7151 ) ;
#23421 = ADVANCED_FACE ( 'NONE', ( #33548 ), #29766, .T. ) ;
#23422 = CARTESIAN_POINT ( 'NONE',  ( 6.444103211791042618, 202.2591342207267644, 35.30113791807856671 ) ) ;
#23423 = CARTESIAN_POINT ( 'NONE',  ( -65.20000000000000284, -7.347880794884118356E-15, 270.4495957273638282 ) ) ;
#23424 = ORIENTED_EDGE ( 'NONE', *, *, #16665, .T. ) ;
#23425 = CARTESIAN_POINT ( 'NONE',  ( 3.093533885183100018, 6.874201416487501604, -7.446478553995813598 ) ) ;
#23426 = AXIS2_PLACEMENT_3D ( 'NONE', #11078, #16169, #13786 ) ;
#23427 = CARTESIAN_POINT ( 'NONE',  ( 84.22499999726879594, 149.9369285172503510, 15.58253174999999580 ) ) ;
#23428 = CARTESIAN_POINT ( 'NONE',  ( 62.70000000000001705, -88.00000000000000000, 30.00000000000000000 ) ) ;
#23429 = CARTESIAN_POINT ( 'NONE',  ( -6.444103211791042618, 211.7408657792732356, 84.80113791807858092 ) ) ;
#23430 = FACE_BOUND ( 'NONE', #14145, .T. ) ;
#23431 = CARTESIAN_POINT ( 'NONE',  ( 50.10000000000000853, 141.2096805137202580, -4.480746418436742040 ) ) ;
#23432 = CARTESIAN_POINT ( 'NONE',  ( -4.984841277089891776, 213.7757310962905990, 65.94886208192144750 ) ) ;
#23433 = DIRECTION ( 'NONE',  ( -0.000000000000000000, -0.000000000000000000, 1.000000000000000000 ) ) ;
#23434 = CARTESIAN_POINT ( 'NONE',  ( 50.92499999726880588, 145.8408176439707802, -12.60653300113719588 ) ) ;
#23435 = CARTESIAN_POINT ( 'NONE',  ( 3.135527875058820690, 216.4958274776887492, 4.401137918078565470 ) ) ;
#23436 = CARTESIAN_POINT ( 'NONE',  ( 87.50000000000001421, 155.0000000000000000, -70.00000000000002842 ) ) ;
#23437 = CARTESIAN_POINT ( 'NONE',  ( 58.32499999726881157, 145.8408176439707802, 12.60653300113718345 ) ) ;
#23438 = CARTESIAN_POINT ( 'NONE',  ( 73.17499999726881299, 145.8408176439707802, -12.60653300113719588 ) ) ;
#23439 = CARTESIAN_POINT ( 'NONE',  ( -9.736236675707914401, 199.9851607334237542, 63.20113791807857240 ) ) ;
#23440 = CARTESIAN_POINT ( 'NONE',  ( -60.00000000000000000, -7.347880794884118356E-15, 20.00000000000001776 ) ) ;
#23441 = CARTESIAN_POINT ( 'NONE',  ( -3.753561863808691168, 195.6020594897209435, 14.90113791807856636 ) ) ;
#23442 = CARTESIAN_POINT ( 'NONE',  ( 8.062137200540920645, 201.0835637161417822, 83.30113791807858092 ) ) ;
#23443 = CARTESIAN_POINT ( 'NONE',  ( 35.68867513459483121, 159.8737954434934920, 15.00000000000010836 ) ) ;
#23444 = CARTESIAN_POINT ( 'NONE',  ( -12.01549611932659722, 210.8513442034533227, 56.64886208192142902 ) ) ;
#23445 = CARTESIAN_POINT ( 'NONE',  ( 10.01549611932659367, 203.7984951890124421, 61.14886208192144323 ) ) ;
#23446 = CARTESIAN_POINT ( 'NONE',  ( 12.00000000000000711, 206.9523078486586485, 101.0011379180785696 ) ) ;
#23447 = CARTESIAN_POINT ( 'NONE',  ( -67.50001199999999812, 167.8075758004702038, 11.23405475987244273 ) ) ;
#23448 = CARTESIAN_POINT ( 'NONE',  ( 10.01549611932653860, 210.2015048109876716, 10.85113791807856387 ) ) ;
#23449 = CARTESIAN_POINT ( 'NONE',  ( -10.01549611932659722, 210.2015048109875011, 77.64886208192143613 ) ) ;
#23450 = ORIENTED_EDGE ( 'NONE', *, *, #19298, .F. ) ;
#23451 = CARTESIAN_POINT ( 'NONE',  ( -12.00000000000000711, 206.9523078486584780, 80.49886208192144466 ) ) ;
#23452 = CARTESIAN_POINT ( 'NONE',  ( 3.135527875058820690, 216.4958274776887492, 100.4011379180785752 ) ) ;
#23453 = EDGE_LOOP ( 'NONE', ( #25278, #8663, #2837, #26292 ) ) ;
#23454 = FACE_OUTER_BOUND ( 'NONE', #24546, .T. ) ;
#23455 = CARTESIAN_POINT ( 'NONE',  ( -4.903702542908436435, 200.1653181626580249, 65.04886208192144181 ) ) ;
#23456 = ORIENTED_EDGE ( 'NONE', *, *, #11389, .F. ) ;
#23457 = EDGE_CURVE ( 'NONE', #25621, #27498, #26318, .T. ) ;
#23458 = CARTESIAN_POINT ( 'NONE',  ( 72.62499999726880162, 138.6155565068815747, -3.929120461958505118E-15 ) ) ;
#23459 = CARTESIAN_POINT ( 'NONE',  ( 58.50000000000001421, -88.00000000000000000, 30.00000000000000000 ) ) ;
#23460 = CARTESIAN_POINT ( 'NONE',  ( -57.24471460971760450, 194.9412964752286825, 2.168227419017068502 ) ) ;
#23461 = EDGE_CURVE ( 'NONE', #32913, #16785, #18046, .T. ) ;
#23462 = CARTESIAN_POINT ( 'NONE',  ( 63.62499999726879452, 171.3844434931184253, -7.942151717890132712E-15 ) ) ;
#23463 = CARTESIAN_POINT ( 'NONE',  ( 0.000000000000000000, 0.000000000000000000, 0.000000000000000000 ) ) ;
#23464 = CARTESIAN_POINT ( 'NONE',  ( -10.01549611932659722, 210.2015048109875011, 50.64886208192143613 ) ) ;
#23465 = ORIENTED_EDGE ( 'NONE', *, *, #299, .T. ) ;
#23466 = CARTESIAN_POINT ( 'NONE',  ( 14.91983402814537740, 23.14029461301515056, -17.98559444045776701 ) ) ;
#23467 = ADVANCED_FACE ( 'NONE', ( #28096, #20435 ), #30831, .T. ) ;
#23468 = DIRECTION ( 'NONE',  ( 1.000000000000000000, 0.000000000000000000, 0.000000000000000000 ) ) ;
#23469 = CARTESIAN_POINT ( 'NONE',  ( 7.984503880673422316, 209.6470497212048372, 33.84886208192144608 ) ) ;
#23470 = CARTESIAN_POINT ( 'NONE',  ( 0.05014649552810505201, 217.5146222423826714, 70.25113791807858377 ) ) ;
#23471 = DIRECTION ( 'NONE',  ( 1.000000000000000000, -0.000000000000000000, -0.000000000000000000 ) ) ;
#23472 = CARTESIAN_POINT ( 'NONE',  ( -0.05014649552810635652, 196.4853777576173002, 56.75113791807855534 ) ) ;
#23473 = CARTESIAN_POINT ( 'NONE',  ( 8.062137200540920645, 201.0835637161417822, 23.30113791807856671 ) ) ;
#23474 = CARTESIAN_POINT ( 'NONE',  ( -6.500168698208129925, 202.3363017425936050, 18.20113791807856529 ) ) ;
#23475 = CARTESIAN_POINT ( 'NONE',  ( 119.7500000000000000, -0.6872233929727361579, 35.00001200000000523 ) ) ;
#23476 = CARTESIAN_POINT ( 'NONE',  ( -65.20000000000000284, -7.347880794884118356E-15, 19.29999999999998295 ) ) ;
#23477 = CARTESIAN_POINT ( 'NONE',  ( 39.82499999726881157, 168.2552932293087906, 9.630534252274372875 ) ) ;
#23478 = CARTESIAN_POINT ( 'NONE',  ( 11.98450388067348271, 203.0532714938637753, 38.15113791807856813 ) ) ;
#23479 = FACE_OUTER_BOUND ( 'NONE', #8518, .T. ) ;
#23480 = EDGE_CURVE ( 'NONE', #16947, #4416, #7997, .T. ) ;
#23481 = CARTESIAN_POINT ( 'NONE',  ( -10.01549611932653860, 203.7984951890123284, 81.35113791807857808 ) ) ;
#23482 = CARTESIAN_POINT ( 'NONE',  ( 10.01549611932653860, 210.2015048109876716, 55.85113791807857098 ) ) ;
#23483 = CARTESIAN_POINT ( 'NONE',  ( 0.05014649552828288198, 194.3824533091408000, 19.74886208192143400 ) ) ;
#23484 = CARTESIAN_POINT ( 'NONE',  ( 10.00000000000000711, 207.0476921513415220, 27.99886208192143755 ) ) ;
#23485 = CONICAL_SURFACE ( 'NONE', #20759, 8.542937654374687995, 1.221730476396047926 ) ;
#23486 = CARTESIAN_POINT ( 'NONE',  ( 78.89999999453762314, 159.7113355953771077, 14.49999999999999289 ) ) ;
#23487 = CARTESIAN_POINT ( 'NONE',  ( 9.736236675707914401, 214.0148392665762458, 64.70113791807857240 ) ) ;
#23488 = CARTESIAN_POINT ( 'NONE',  ( 8.000000000000008882, 206.9523078486586485, 89.00113791807858377 ) ) ;
#23489 = ADVANCED_FACE ( 'NONE', ( #18869, #31981 ), #15816, .T. ) ;
#23490 = CARTESIAN_POINT ( 'NONE',  ( -9.984503880673420539, 203.7031108863293980, 50.34886208192141765 ) ) ;
#23491 = CARTESIAN_POINT ( 'NONE',  ( 49.58867513459482268, 163.8167787843871110, 12.13525491562421621 ) ) ;
#23492 = ORIENTED_EDGE ( 'NONE', *, *, #26864, .F. ) ;
#23493 = CARTESIAN_POINT ( 'NONE',  ( 12.01549611932659367, 203.1486557965466773, 49.14886208192143613 ) ) ;
#23494 = AXIS2_PLACEMENT_3D ( 'NONE', #32306, #1802, #32467 ) ;
#23495 = ORIENTED_EDGE ( 'NONE', *, *, #1139, .T. ) ;
#23496 = ORIENTED_EDGE ( 'NONE', *, *, #28982, .F. ) ;
#23497 = EDGE_CURVE ( 'NONE', #18054, #31501, #21586, .T. ) ;
#23498 = CARTESIAN_POINT ( 'NONE',  ( -63.50000000000001421, 210.0000000000000000, 0.000000000000000000 ) ) ;
#23499 = FACE_OUTER_BOUND ( 'NONE', #9802, .T. ) ;
#23500 = CARTESIAN_POINT ( 'NONE',  ( 4.984841277089725686, 213.7757310962907411, 46.55113791807856671 ) ) ;
#23501 = PRESENTATION_STYLE_ASSIGNMENT (( #2736 ) ) ;
#23502 = CARTESIAN_POINT ( 'NONE',  ( 6.139770520408223575, 215.5359834540460611, 24.54886208192143471 ) ) ;
#23503 = CARTESIAN_POINT ( 'NONE',  ( 63.87499999726880873, 171.3844434931184253, -7.942151717890134290E-15 ) ) ;
#23504 = ORIENTED_EDGE ( 'NONE', *, *, #13698, .T. ) ;
#23505 = DIRECTION ( 'NONE',  ( -1.000000000000000000, 0.000000000000000000, 0.000000000000000000 ) ) ;
#23506 = CIRCLE ( 'NONE', #27314, 4.000000000000000000 ) ;
#23507 = CARTESIAN_POINT ( 'NONE',  ( 78.00000000000001421, 4.475777889183788807E-16, -3.309499999999999886 ) ) ;
#23508 = CARTESIAN_POINT ( 'NONE',  ( -4.984841277089891776, 213.7757310962905990, 8.948862081921433287 ) ) ;
#23509 = CARTESIAN_POINT ( 'NONE',  ( 8.118202686958039038, 212.8392687619912635, 43.70113791807857240 ) ) ;
#23510 = CARTESIAN_POINT ( 'NONE',  ( 79.91132485994282320, 163.8167787843871110, -12.13525491562423397 ) ) ;
#23511 = EDGE_CURVE ( 'NONE', #3624, #30882, #18347, .T. ) ;
#23512 = CARTESIAN_POINT ( 'NONE',  ( 9.984503880673470277, 203.7031108863295401, 29.15113791807856103 ) ) ;
#23513 = CARTESIAN_POINT ( 'NONE',  ( -10.01549611932659545, 210.2015048109875011, 101.6488620819214361 ) ) ;
#23514 = APPLICATION_PROTOCOL_DEFINITION ( 'draft international standard', 'automotive_design', 1998, #23568 ) ;
#23515 = CARTESIAN_POINT ( 'NONE',  ( 8.000000000000008882, 207.0476921513415220, 87.99886208192144466 ) ) ;
#23516 = CONICAL_SURFACE ( 'NONE', #27853, 32.00000000000002842, 1.466076571675243523 ) ;
#23517 = CARTESIAN_POINT ( 'NONE',  ( 85.90000000000000568, 141.2096805137202580, 4.480746418436733158 ) ) ;
#23518 = CARTESIAN_POINT ( 'NONE',  ( -64.50000000000000000, 120.3589838486224579, -20.00000000000000000 ) ) ;
#23519 = FACE_OUTER_BOUND ( 'NONE', #30917, .T. ) ;
#23520 = CARTESIAN_POINT ( 'NONE',  ( -12.01549611932652972, 203.1486557965464499, 6.351137918078565647 ) ) ;
#23521 = FACE_OUTER_BOUND ( 'NONE', #6610, .T. ) ;
#23522 = CARTESIAN_POINT ( 'NONE',  ( 56.97499999726881015, 140.1801316387863778, -4.815267126137194431 ) ) ;
#23523 = ADVANCED_FACE ( 'NONE', ( #10715 ), #5592, .T. ) ;
#23524 = CARTESIAN_POINT ( 'NONE',  ( 8.118202686958039038, 212.8392687619912635, 55.70113791807857950 ) ) ;
#23525 = CARTESIAN_POINT ( 'NONE',  ( -8.118202686958039038, 201.1607312380087080, 30.20113791807856884 ) ) ;
#23526 = DIRECTION ( 'NONE',  ( 1.000000000000000000, 0.000000000000000000, 0.000000000000000000 ) ) ;
#23527 = CARTESIAN_POINT ( 'NONE',  ( -10.00000000000000178, 206.9999999999998863, 103.5000000000000426 ) ) ;
#23528 = CARTESIAN_POINT ( 'NONE',  ( 6.220909254589680693, 198.5229672870052582, 1.448862081921434397 ) ) ;
#23529 = CARTESIAN_POINT ( 'NONE',  ( 63.09999999453763309, 150.2886644046228639, 14.49999999999999645 ) ) ;
#23530 = EDGE_LOOP ( 'NONE', ( #11052, #14802, #12474, #31670 ) ) ;
#23531 = CARTESIAN_POINT ( 'NONE',  ( -9.680171189290831535, 214.0920067884431148, 36.80113791807856671 ) ) ;
#23532 = EDGE_CURVE ( 'NONE', #7491, #15536, #397, .T. ) ;
#23533 = DIRECTION ( 'NONE',  ( 1.000000000000000000, 0.000000000000000000, 0.000000000000000000 ) ) ;
#23534 = CARTESIAN_POINT ( 'NONE',  ( 6.220909254589681581, 198.5229672870052582, 10.44886208192143506 ) ) ;
#23535 = DIRECTION ( 'NONE',  ( -1.000000000000000000, -0.000000000000000000, -0.000000000000000000 ) ) ;
#23536 = ORIENTED_EDGE ( 'NONE', *, *, #8975, .T. ) ;
#23537 = AXIS2_PLACEMENT_3D ( 'NONE', #17219, #20284, #12615 ) ;
#23538 = CARTESIAN_POINT ( 'NONE',  ( -8.118202686958039038, 201.1607312380087080, 75.20113791807857240 ) ) ;
#23539 = VERTEX_POINT ( 'NONE', #18547 ) ;
#23540 = CARTESIAN_POINT ( 'NONE',  ( 8.015496119326595448, 204.4483345814782638, 28.14886208192143968 ) ) ;
#23541 = FACE_OUTER_BOUND ( 'NONE', #30824, .T. ) ;
#23542 = ORIENTED_EDGE ( 'NONE', *, *, #18364, .T. ) ;
#23543 = CARTESIAN_POINT ( 'NONE',  ( -2.517493886308901807, 199.4062855549015012, 8.901137918078566358 ) ) ;
#23544 = VECTOR ( 'NONE', #30783, 1000.000000000000000 ) ;
#23545 = CARTESIAN_POINT ( 'NONE',  ( 12.01549611932659367, 203.1486557965466773, 103.1488620819214361 ) ) ;
#23546 = CARTESIAN_POINT ( 'NONE',  ( 43.17499999726881299, 145.8408176439707802, -12.60653300113719588 ) ) ;
#23547 = ORIENTED_EDGE ( 'NONE', *, *, #7865, .F. ) ;
#23548 = CARTESIAN_POINT ( 'NONE',  ( 52.72499999726881015, 140.1801316387863778, -4.815267126137194431 ) ) ;
#23549 = DIRECTION ( 'NONE',  ( 0.000000000000000000, -1.000000000000000000, 9.682177540335733218E-15 ) ) ;
#23550 = CARTESIAN_POINT ( 'NONE',  ( -10.00000000000000711, 207.0476921513413515, 12.50113791807856778 ) ) ;
#23551 = CARTESIAN_POINT ( 'NONE',  ( -8.062137200540822946, 201.0835637161416400, 80.19886208192143329 ) ) ;
#23552 = CARTESIAN_POINT ( 'NONE',  ( 55.97499999726881015, 169.8198683612136222, 4.815267126137181997 ) ) ;
#23553 = CARTESIAN_POINT ( 'NONE',  ( -67.50001199999996970, 141.4831703651135228, 10.36982646209945003 ) ) ;
#23554 = CARTESIAN_POINT ( 'NONE',  ( 10.00000000000000711, 206.9523078486586201, 17.00113791807856600 ) ) ;
#23555 = CARTESIAN_POINT ( 'NONE',  ( 44.28867513459481842, 139.2280666364260071, -4.041636747397287284E-15 ) ) ;
#23556 = EDGE_CURVE ( 'NONE', #5223, #31333, #25226, .T. ) ;
#23557 = EDGE_CURVE ( 'NONE', #17200, #8086, #1460, .T. ) ;
#23558 = VECTOR ( 'NONE', #24352, 999.9999999999998863 ) ;
#23559 = CARTESIAN_POINT ( 'NONE',  ( 67.19999999999998863, 167.3344367211045096, 8.961492836873468093 ) ) ;
#23560 = CARTESIAN_POINT ( 'NONE',  ( 77.50000000000000000, 155.0000000000000000, -6.938893903907228378E-15 ) ) ;
#23561 = CARTESIAN_POINT ( 'NONE',  ( 37.88867513459482694, 150.1262045565064227, 15.00000000000001599 ) ) ;
#23562 = CARTESIAN_POINT ( 'NONE',  ( 8.118202686958039038, 212.8392687619912635, 88.70113791807857240 ) ) ;
#23563 = DIRECTION ( 'NONE',  ( 1.000000000000000000, 0.000000000000000000, 0.000000000000000000 ) ) ;
#23564 = ADVANCED_FACE ( 'NONE', ( #31814 ), #10559, .T. ) ;
#23565 = CARTESIAN_POINT ( 'NONE',  ( 35.37499999726881583, 155.0000000000000000, -15.58253175000000823 ) ) ;
#23566 = ADVANCED_FACE ( 'NONE', ( #29101 ), #28683, .T. ) ;
#23567 = CARTESIAN_POINT ( 'NONE',  ( -12.00000000000000711, 206.9523078486584780, 101.4988620819214304 ) ) ;
#23568 = APPLICATION_CONTEXT ( 'automotive_design' ) ;
#23569 = CARTESIAN_POINT ( 'NONE',  ( 70.52499999726880731, 140.1801316387863778, 4.815267126137185549 ) ) ;
#23570 = ORIENTED_EDGE ( 'NONE', *, *, #14716, .T. ) ;
#23571 = CARTESIAN_POINT ( 'NONE',  ( -60.98407617557292326, 194.9989950908677088, 0.3262505061364526227 ) ) ;
#23572 = CARTESIAN_POINT ( 'NONE',  ( 38.39999999453763024, 168.7903194862797420, -4.480746418436745593 ) ) ;
#23573 = CARTESIAN_POINT ( 'NONE',  ( 11.98450388067348271, 203.0532714938637753, 92.15113791807856103 ) ) ;
#23574 = AXIS2_PLACEMENT_3D ( 'NONE', #3122, #27133, #26958 ) ;
#23575 = DIRECTION ( 'NONE',  ( -0.000000000000000000, 1.000000000000000000, 1.224646799147353207E-16 ) ) ;
#23576 = AXIS2_PLACEMENT_3D ( 'NONE', #17086, #9248, #24758 ) ;
#23577 = ORIENTED_EDGE ( 'NONE', *, *, #26207, .T. ) ;
#23578 = CARTESIAN_POINT ( 'NONE',  ( 8.118202686958138514, 201.1607312380088501, 91.29886208192144181 ) ) ;
#23579 = CARTESIAN_POINT ( 'NONE',  ( 0.05014649552828288198, 194.3824533091408000, 25.74886208192143755 ) ) ;
#23580 = CARTESIAN_POINT ( 'NONE',  ( 92.59660660068168170, 155.0000000000000000, 0.000000000000000000 ) ) ;
#23581 = CARTESIAN_POINT ( 'NONE',  ( 10.01549611932653860, 210.2015048109876716, 46.85113791807856387 ) ) ;
#23582 = EDGE_LOOP ( 'NONE', ( #14142, #18636, #2682, #17492, #30500, #6940 ) ) ;
#23583 = CARTESIAN_POINT ( 'NONE',  ( -8.000000000000008882, 206.9523078486584780, 8.498862081921435774 ) ) ;
#23584 = AXIS2_PLACEMENT_3D ( 'NONE', #15076, #11854, #20024 ) ;
#23585 = CARTESIAN_POINT ( 'NONE',  ( 74.71132485994280614, 155.0000000000000000, 15.00000000000001243 ) ) ;
#23586 = VERTEX_POINT ( 'NONE', #21587 ) ;
#23588 = CARTESIAN_POINT ( 'NONE',  ( -0.05014649552828365914, 215.4116977939061144, 93.24886208192143044 ) ) ;
#23587 =( GEOMETRIC_REPRESENTATION_CONTEXT ( 3 ) GLOBAL_UNCERTAINTY_ASSIGNED_CONTEXT ( ( #6346 ) ) GLOBAL_UNIT_ASSIGNED_CONTEXT ( ( #32798, #13902, #11353 ) ) REPRESENTATION_CONTEXT ( 'NONE', 'WORKASPACE' ) );
#23589 = CARTESIAN_POINT ( 'NONE',  ( -2.426778023690262742, 214.6231898156240163, 31.10113791807856742 ) ) ;
#23590 = DIRECTION ( 'NONE',  ( 1.000000000000000000, 0.000000000000000000, 0.000000000000000000 ) ) ;
#23591 = ORIENTED_EDGE ( 'NONE', *, *, #16401, .T. ) ;
#23592 = CARTESIAN_POINT ( 'NONE',  ( 10.40000000000000036, 6.123233995736768255E-16, -5.000000000000001776 ) ) ;
#23593 = AXIS2_PLACEMENT_3D ( 'NONE', #14159, #6149, #26599 ) ;
#23594 =( BOUNDED_CURVE ( )  B_SPLINE_CURVE ( 2, ( #19118, #24057, #29508, #8075, #21504, #6161, #10956, #29009, #16223, #13503, #5502 ),
 .UNSPECIFIED., .F., .T. ) 
 B_SPLINE_CURVE_WITH_KNOTS ( ( 3, 2, 2, 2, 2, 3 ),
 ( 0.2499999999999999445, 0.2535714285714285032, 0.2571428571428570620, 0.2607142857142857317, 0.2642857142857142905, 0.2678571428571428492 ),
 .UNSPECIFIED. ) 
 CURVE ( )  GEOMETRIC_REPRESENTATION_ITEM ( )  RATIONAL_B_SPLINE_CURVE ( ( 1.000000000000000666, 0.9510565162951526430, 1.000000000000000000, 0.9510565162951534202, 1.000000000000000000, 0.9510565162951534202, 1.000000000000000000, 0.9510565162951534202, 1.000000000000000000, 0.9510565162951534202, 1.000000000000000000 ) ) 
 REPRESENTATION_ITEM ( '' )  );
#23595 = CARTESIAN_POINT ( 'NONE',  ( 36.27499999726880731, 160.0630714827496206, 15.58253174999999402 ) ) ;
#23596 = DIRECTION ( 'NONE',  ( -0.9945218953682717355, 0.000000000000000000, 0.1045284632676676817 ) ) ;
#23597 = CARTESIAN_POINT ( 'NONE',  ( 7.984503880673485376, 204.3529502787953902, 92.15113791807856103 ) ) ;
#23598 = AXIS2_PLACEMENT_3D ( 'NONE', #6168, #10799, #24230 ) ;
#23599 = CARTESIAN_POINT ( 'NONE',  ( 67.49999999999998579, 155.0000000000000000, 0.000000000000000000 ) ) ;
#23600 = CARTESIAN_POINT ( 'NONE',  ( 49.39999999999999147, 159.7113355953771077, 14.49999999999999289 ) ) ;
#23601 = CARTESIAN_POINT ( 'NONE',  ( -6.500168698208244500, 211.6636982574061676, 59.79886208192143471 ) ) ;
#23602 = DIRECTION ( 'NONE',  ( -0.000000000000000000, -0.000000000000000000, 1.000000000000000000 ) ) ;
#23603 = CARTESIAN_POINT ( 'NONE',  ( 49.22499999726881725, 160.0630714827496206, -15.58253175000000823 ) ) ;
#23604 = CARTESIAN_POINT ( 'NONE',  ( -6.220909254589537696, 198.5229672870051445, 6.051137918078565825 ) ) ;
#23605 = DIRECTION ( 'NONE',  ( 1.000000000000000000, -0.000000000000000000, -0.000000000000000000 ) ) ;
#23606 = CARTESIAN_POINT ( 'NONE',  ( 66.52499999726880731, 140.1801316387863778, 4.815267126137185549 ) ) ;
#23607 = CARTESIAN_POINT ( 'NONE',  ( 67.07499999726880446, 141.7447067706911810, -9.630534252274385310 ) ) ;
#23608 = CARTESIAN_POINT ( 'NONE',  ( 7.456977232089302632, 217.1783343296989131, 70.55113791807856671 ) ) ;
#23609 = DIRECTION ( 'NONE',  ( 0.000000000000000000, 0.000000000000000000, -1.000000000000000000 ) ) ;
#23610 = CARTESIAN_POINT ( 'NONE',  ( -10.00000000000000711, 207.0476921513413515, 87.50113791807858377 ) ) ;
#23611 = CARTESIAN_POINT ( 'NONE',  ( -12.01549611932659722, 210.8513442034533227, 53.64886208192142902 ) ) ;
#23612 = CARTESIAN_POINT ( 'NONE',  ( -6.139770520408224463, 198.4640165459539105, 59.04886208192143471 ) ) ;
#23613 = AXIS2_PLACEMENT_3D ( 'NONE', #5279, #23675, #10411 ) ;
#23614 = CARTESIAN_POINT ( 'NONE',  ( -7.456977232089304408, 196.8216656703010301, 96.05113791807858092 ) ) ;
#23615 = CARTESIAN_POINT ( 'NONE',  ( 4.000000000000000000, 3.518949890710768802, -4.770489558936219510E-15 ) ) ;
#23616 = CARTESIAN_POINT ( 'NONE',  ( -8.118202686958039038, 201.1607312380087080, 12.20113791807856707 ) ) ;
#23617 = CIRCLE ( 'NONE', #11650, 2.149999999999974598 ) ;
#23618 = CARTESIAN_POINT ( 'NONE',  ( -8.062137200540822946, 201.0835637161416400, 80.19886208192143329 ) ) ;
#23619 = EDGE_LOOP ( 'NONE', ( #30244, #26889 ) ) ;
#23620 = CARTESIAN_POINT ( 'NONE',  ( -10.01549611932653860, 203.7984951890123284, 96.35113791807853545 ) ) ;
#23621 = ORIENTED_EDGE ( 'NONE', *, *, #2242, .T. ) ;
#23622 = DIRECTION ( 'NONE',  ( 1.000000000000000000, 0.000000000000000000, 0.000000000000000000 ) ) ;
#23623 = CARTESIAN_POINT ( 'NONE',  ( 4.903702542908435547, 213.8346818373419751, 63.54886208192144181 ) ) ;
#23624 = ORIENTED_EDGE ( 'NONE', *, *, #29387, .T. ) ;
#23625 = CARTESIAN_POINT ( 'NONE',  ( 78.92499999726881299, 145.8408176439707802, -12.60653300113719588 ) ) ;
#23626 = DIRECTION ( 'NONE',  ( 1.000000000000000000, 0.000000000000000000, 0.000000000000000000 ) ) ;
#23627 = COLOUR_RGB ( '', 0.31764706, 0.68627451, 0.89019608) ;
#23628 = DIRECTION ( 'NONE',  ( 0.000000000000000000, 0.000000000000000000, 1.000000000000000000 ) ) ;
#23629 = CARTESIAN_POINT ( 'NONE',  ( 67.12499999726881583, 155.0000000000000000, -15.58253175000000823 ) ) ;
#23630 = CARTESIAN_POINT ( 'NONE',  ( 7.984503880673485376, 204.3529502787953902, 62.15113791807858945 ) ) ;
#23631 = CARTESIAN_POINT ( 'NONE',  ( -7.500000000000667910, 3.157052757790226316, -7.642767288269818771 ) ) ;
#23632 = CARTESIAN_POINT ( 'NONE',  ( 3.135527875058981895, 197.5041725223112792, 49.59886208192143897 ) ) ;
#23633 = LINE ( 'NONE', #26353, #22720 ) ;
#23634 = PRESENTATION_LAYER_ASSIGNMENT (  '', '', ( #27423 ) ) ;
#23635 = SURFACE_STYLE_USAGE ( .BOTH. , #7974 ) ;
#23636 = CARTESIAN_POINT ( 'NONE',  ( 117.5000000000000000, 255.8678580070898363, -25.91453920131760924 ) ) ;
#23637 = CARTESIAN_POINT ( 'NONE',  ( -2.517493886309087880, 214.5937144450984135, 33.09886208192143897 ) ) ;
#23638 = CARTESIAN_POINT ( 'NONE',  ( -8.062137200540920645, 212.9164362838581894, 78.80113791807858092 ) ) ;
#23639 = FACE_OUTER_BOUND ( 'NONE', #30371, .T. ) ;
#23640 = CARTESIAN_POINT ( 'NONE',  ( -10.01549611932653860, 203.7984951890123284, 54.35113791807856387 ) ) ;
#23641 = CARTESIAN_POINT ( 'NONE',  ( 0.05014649552810505201, 217.5146222423826714, 28.25113791807855890 ) ) ;
#23642 = CARTESIAN_POINT ( 'NONE',  ( 2.517493886308900919, 214.5937144450984420, 13.40113791807856636 ) ) ;
#23643 = CARTESIAN_POINT ( 'NONE',  ( 119.8866434474913518, -1.374176392886190756, 35.00001199999999102 ) ) ;
#23644 = CARTESIAN_POINT ( 'NONE',  ( -2.055025722542106692, 6.319083845363845597, -5.720331885005371930 ) ) ;
#23645 = CARTESIAN_POINT ( 'NONE',  ( 43.12499999726881583, 155.0000000000000000, -15.58253175000000823 ) ) ;
#23646 = CARTESIAN_POINT ( 'NONE',  ( -12.00000000000000711, 207.0476921513413515, 42.50113791807856245 ) ) ;
#23647 = DIRECTION ( 'NONE',  ( 1.000000000000000000, 0.000000000000000000, 0.000000000000000000 ) ) ;
#23648 = CARTESIAN_POINT ( 'NONE',  ( 9.984503880673470277, 203.7031108863295401, 89.15113791807857524 ) ) ;
#23649 = EDGE_CURVE ( 'NONE', #31501, #22995, #16141, .T. ) ;
#23650 = CARTESIAN_POINT ( 'NONE',  ( -0.05014649552810635652, 196.4853777576173002, 59.75113791807857666 ) ) ;
#23651 = CARTESIAN_POINT ( 'NONE',  ( 12.00000000000000711, 207.0476921513415220, 18.99886208192143400 ) ) ;
#23652 = CARTESIAN_POINT ( 'NONE',  ( 3.135527875058981895, 197.5041725223112792, 25.59886208192143897 ) ) ;
#23653 = CARTESIAN_POINT ( 'NONE',  ( 82.39999999453763735, 168.7903194862797420, -4.480746418436745593 ) ) ;
#23654 = CARTESIAN_POINT ( 'NONE',  ( 12.01549611932652972, 210.8513442034534933, 70.85113791807857808 ) ) ;
#23655 = CARTESIAN_POINT ( 'NONE',  ( -6.500168698208129925, 202.3363017425936050, 84.20113791807858661 ) ) ;
#23656 = CARTESIAN_POINT ( 'NONE',  ( -10.01549611932659722, 210.2015048109875011, 53.64886208192141481 ) ) ;
#23657 = DIRECTION ( 'NONE',  ( -0.000000000000000000, 0.000000000000000000, -1.000000000000000000 ) ) ;
#23658 = VERTEX_POINT ( 'NONE', #26533 ) ;
#23659 = CARTESIAN_POINT ( 'NONE',  ( -12.01549611932659722, 210.8513442034533227, 50.64886208192143613 ) ) ;
#23660 = ORIENTED_EDGE ( 'NONE', *, *, #33526, .T. ) ;
#23661 = ORIENTED_EDGE ( 'NONE', *, *, #1569, .F. ) ;
#23662 = DIRECTION ( 'NONE',  ( 1.000000000000000000, -0.000000000000000000, -0.000000000000000000 ) ) ;
#23663 = CARTESIAN_POINT ( 'NONE',  ( -66.50402289005056389, 121.5305141831588003, 17.99597710994943967 ) ) ;
#23664 = CARTESIAN_POINT ( 'NONE',  ( 7.984503880673485376, 204.3529502787953902, 41.15113791807857524 ) ) ;
#23665 = LINE ( 'NONE', #23343, #21590 ) ;
#23666 = CARTESIAN_POINT ( 'NONE',  ( -9.984503880673420539, 203.7031108863293980, 26.34886208192142831 ) ) ;
#23667 = CARTESIAN_POINT ( 'NONE',  ( 63.17499999726880588, 145.8408176439707802, -12.60653300113719588 ) ) ;
#23668 = ORIENTED_EDGE ( 'NONE', *, *, #26407, .F. ) ;
#23669 = CARTESIAN_POINT ( 'NONE',  ( 115.4999999999999858, 155.0000000000000000, -50.00000000000000711 ) ) ;
#23670 = B_SPLINE_CURVE_WITH_KNOTS ( 'NONE', 3,
 ( #29481, #27262, #9034, #24543, #29656, #11104, #19094, #3416, #3586, #16699, #26587, #23870, #24034, #16869, #18927, #24205, #6305, #11263, #26753, #1041, #702, #26928, #32370, #868, #21483, #6490, #8704, #21983, #5971, #13978, #13812, #16531, #5800, #6137 ),
 .UNSPECIFIED., .F., .F.,
 ( 4, 2, 2, 2, 2, 2, 2, 2, 2, 2, 2, 2, 2, 2, 2, 2, 4 ),
 ( 0.000000000000000000, 0.0004886277888461246482, 0.0009772555776922492964, 0.001465883366538373945, 0.001954511155384498593, 0.002443138944230623458, 0.002931766733076747889, 0.003420394521922872320, 0.003909022310768997185, 0.004397650099615122050, 0.004886277888461246915, 0.005374905677307370913, 0.005863533466153495778, 0.006352161254999620643, 0.006840789043845744641, 0.007329416832691869506, 0.007818044621537994371 ),
 .UNSPECIFIED. ) ;
#23671 = CARTESIAN_POINT ( 'NONE',  ( -7.263825692932299738, -4.945657111639584436, -7.907570769506049757 ) ) ;
#23672 = CARTESIAN_POINT ( 'NONE',  ( -7.984503880673422316, 204.3529502787951628, 5.348862081921435419 ) ) ;
#23673 = EDGE_CURVE ( 'NONE', #24872, #19887, #23986, .T. ) ;
#23674 = CARTESIAN_POINT ( 'NONE',  ( -10.01549611932653860, 203.7984951890123284, 54.35113791807856387 ) ) ;
#23675 = DIRECTION ( 'NONE',  ( -1.000000000000000000, 0.000000000000000000, 0.000000000000000000 ) ) ;
#23676 = PRODUCT_DEFINITION_SHAPE ( 'NONE', 'NONE',  #33716 ) ;
#23677 = CARTESIAN_POINT ( 'NONE',  ( 3.135527875058820690, 216.4958274776887492, 28.40113791807856813 ) ) ;
#23678 = CARTESIAN_POINT ( 'NONE',  ( 82.47499999726881015, 149.9369285172503510, 15.58253174999999580 ) ) ;
#23679 = CARTESIAN_POINT ( 'NONE',  ( 4.984841277089891776, 200.2242689037093726, 91.44886208192143329 ) ) ;
#23680 = CARTESIAN_POINT ( 'NONE',  ( 41.62499999726880162, 171.3844434931184253, -7.942151717890132712E-15 ) ) ;
#23681 = CARTESIAN_POINT ( 'NONE',  ( -56.61573505521625549, 194.9660755786677555, 1.651105572388385401 ) ) ;
#23682 = DIRECTION ( 'NONE',  ( 0.000000000000000000, 0.000000000000000000, -1.000000000000000000 ) ) ;
#23683 = CARTESIAN_POINT ( 'NONE',  ( -12.00000000000000711, 207.0476921513413515, 9.501137918078566003 ) ) ;
#23684 = DIRECTION ( 'NONE',  ( 1.000000000000000000, -0.000000000000000000, -0.000000000000000000 ) ) ;
#23685 = CARTESIAN_POINT ( 'NONE',  ( 56.77499999726881441, 140.1801316387863778, 4.815267126137185549 ) ) ;
#23686 = CARTESIAN_POINT ( 'NONE',  ( 9.984503880673470277, 203.7031108863295401, 59.15113791807858235 ) ) ;
#23687 = EDGE_CURVE ( 'NONE', #10532, #33564, #19405, .T. ) ;
#23688 = CARTESIAN_POINT ( 'NONE',  ( 6.139770520408367460, 198.4640165459539389, 32.45113791807857240 ) ) ;
#23689 = CARTESIAN_POINT ( 'NONE',  ( 102.4138169258850581, 155.0000000000000000, -32.10452846326769816 ) ) ;
#23690 = CARTESIAN_POINT ( 'NONE',  ( -7.500000000000000000, -3.469446951953614189E-15, -6.991905250253751980 ) ) ;
#23691 = CARTESIAN_POINT ( 'NONE',  ( 8.062137200540822946, 212.9164362838583315, 3.698862081921434619 ) ) ;
#23692 = CARTESIAN_POINT ( 'NONE',  ( 61.29999999453762882, 142.6655632788954620, 8.961492836873471646 ) ) ;
#23693 = VERTEX_POINT ( 'NONE', #11046 ) ;
#23694 = CARTESIAN_POINT ( 'NONE',  ( 12.01549611932652972, 210.8513442034534933, 40.85113791807856387 ) ) ;
#23695 = DIRECTION ( 'NONE',  ( -0.8289387912553660698, 0.000000000000000000, 0.5593393248754217062 ) ) ;
#23696 = CARTESIAN_POINT ( 'NONE',  ( -3.135527875058982783, 216.4958274776886924, 24.09886208192143542 ) ) ;
#23697 = CARTESIAN_POINT ( 'NONE',  ( 44.91132485994280898, 146.1832212156128890, 12.13525491562421976 ) ) ;
#23698 = EDGE_LOOP ( 'NONE', ( #9564, #6823, #29022, #29468 ) ) ;
#23699 = EDGE_CURVE ( 'NONE', #21974, #32863, #17784, .T. ) ;
#23700 = CARTESIAN_POINT ( 'NONE',  ( 10.01549611932653860, 210.2015048109876716, 67.85113791807857808 ) ) ;
#23701 = ORIENTED_EDGE ( 'NONE', *, *, #3635, .T. ) ;
#23702 = CARTESIAN_POINT ( 'NONE',  ( -6.830473686658677934E-14, -4.041451884327390331, -0.3126073911696551910 ) ) ;
#23703 = CARTESIAN_POINT ( 'NONE',  ( 4.506125120515186211, -29.15265225409787675, -16.90910675883081637 ) ) ;
#23704 = MANIFOLD_SOLID_BREP ( 'Hex', #13397 ) ;
#23705 = ORIENTED_EDGE ( 'NONE', *, *, #17471, .F. ) ;
#23706 = CARTESIAN_POINT ( 'NONE',  ( -7.984503880673488041, 209.6470497212046098, 15.65113791807856636 ) ) ;
#23707 = EDGE_CURVE ( 'NONE', #171, #14561, #9069, .T. ) ;
#23708 = CARTESIAN_POINT ( 'NONE',  ( 3.753561863808876797, 195.6020594897209719, 97.59886208192145318 ) ) ;
#23709 = CARTESIAN_POINT ( 'NONE',  ( 45.77499999726881441, 169.8198683612136222, -4.815267126137197984 ) ) ;
#23710 = EDGE_LOOP ( 'NONE', ( #15706, #13771, #23661 ) ) ;
#23711 = CARTESIAN_POINT ( 'NONE',  ( 48.92499999726881299, 145.8408176439707802, -12.60653300113719588 ) ) ;
#23712 = FACE_OUTER_BOUND ( 'NONE', #22430, .T. ) ;
#23713 = CARTESIAN_POINT ( 'NONE',  ( 6.139770520408368348, 198.4640165459539674, 8.451137918078565292 ) ) ;
#23714 = CARTESIAN_POINT ( 'NONE',  ( 0.05014649552828275708, 196.4853777576173002, 79.74886208192143044 ) ) ;
#23715 = ADVANCED_FACE ( 'NONE', ( #980 ), #7456, .F. ) ;
#23716 = CARTESIAN_POINT ( 'NONE',  ( 50.97499999726881725, 140.1801316387863778, -4.815267126137194431 ) ) ;
#23717 = DIRECTION ( 'NONE',  ( 0.000000000000000000, -0.7071067811865506814, -0.7071067811865442421 ) ) ;
#23718 = CARTESIAN_POINT ( 'NONE',  ( -3.044812012440131443, 216.5253028482142952, 10.10113791807856565 ) ) ;
#23719 = CARTESIAN_POINT ( 'NONE',  ( 43.98867513459482836, 146.1832212156128890, 12.13525491562421976 ) ) ;
#23720 = CARTESIAN_POINT ( 'NONE',  ( 71.60000000000000853, 150.2886644046228639, 14.49999999999999645 ) ) ;
#23721 = CARTESIAN_POINT ( 'NONE',  ( 3.135527875058820690, 216.4958274776887492, 97.40113791807858945 ) ) ;
#23722 = CARTESIAN_POINT ( 'NONE',  ( 16.08713178458080861, 22.46635493911270132, -0.07154745401828326024 ) ) ;
#23723 = CARTESIAN_POINT ( 'NONE',  ( -9.984503880673473830, 210.2968891136704315, 84.65113791807857524 ) ) ;
#23724 = CARTESIAN_POINT ( 'NONE',  ( 56.98867513459482126, 163.8167787843871110, -12.13525491562423397 ) ) ;
#23725 = CARTESIAN_POINT ( 'NONE',  ( 40.37499999726880873, 155.0000000000000000, 15.58253174999999402 ) ) ;
#23726 = CARTESIAN_POINT ( 'NONE',  ( -9.680171189290716072, 199.9079932115567146, 92.19886208192143329 ) ) ;
#23727 = CARTESIAN_POINT ( 'NONE',  ( 71.62499999726881583, 171.3844434931184253, -7.942151717890132712E-15 ) ) ;
#23728 = ORIENTED_EDGE ( 'NONE', *, *, #31819, .F. ) ;
#23729 = LINE ( 'NONE', #24227, #33153 ) ;
#23730 = CARTESIAN_POINT ( 'NONE',  ( 39.49999999453761745, 139.7537977485451393, -4.138211985947621020E-15 ) ) ;
#23731 =( BOUNDED_CURVE ( )  B_SPLINE_CURVE ( 2, ( #46, #23867, #3086, #31542, #364, #10768, #7711, #15701, #20813, #10607, #28323 ),
 .UNSPECIFIED., .F., .T. ) 
 B_SPLINE_CURVE_WITH_KNOTS ( ( 3, 2, 2, 2, 2, 3 ),
 ( 0.1785714285714286031, 0.1821428571428571619, 0.1857142857142857484, 0.1892857142857143071, 0.1928571428571428936, 0.1964285714285714524 ),
 .UNSPECIFIED. ) 
 CURVE ( )  GEOMETRIC_REPRESENTATION_ITEM ( )  RATIONAL_B_SPLINE_CURVE ( ( 0.9999999999999996669, 0.9510565162951537532, 1.000000000000000000, 0.9510565162951534202, 1.000000000000000000, 0.9510565162951534202, 1.000000000000000000, 0.9510565162951534202, 1.000000000000000000, 0.9510565162951530871, 1.000000000000000444 ) ) 
 REPRESENTATION_ITEM ( '' )  );
#23732 = DIRECTION ( 'NONE',  ( 1.000000000000000000, 0.000000000000000000, 0.000000000000000000 ) ) ;
#23733 = EDGE_LOOP ( 'NONE', ( #13508, #580 ) ) ;
#23734 = CARTESIAN_POINT ( 'NONE',  ( -0.05014649552828402690, 217.5146222423826714, 96.24886208192144466 ) ) ;
#23735 = CARTESIAN_POINT ( 'NONE',  ( -9.680171189290716072, 199.9079932115567146, 32.19886208192144039 ) ) ;
#23736 = CARTESIAN_POINT ( 'NONE',  ( -65.20000000000000284, -7.347880794884118356E-15, 19.29999999999998295 ) ) ;
#23737 = CARTESIAN_POINT ( 'NONE',  ( -3.135527875058821579, 197.5041725223112223, 41.90113791807856813 ) ) ;
#23738 = ORIENTED_EDGE ( 'NONE', *, *, #1282, .T. ) ;
#23739 = CARTESIAN_POINT ( 'NONE',  ( -8.000000000000008882, 206.9523078486584780, 5.498862081921434886 ) ) ;
#23740 = ADVANCED_FACE ( 'NONE', ( #32482 ), #14429, .T. ) ;
#23741 = EDGE_CURVE ( 'NONE', #11308, #8952, #22429, .T. ) ;
#23742 = CIRCLE ( 'NONE', #349, 13.50000000000001066 ) ;
#23743 = CARTESIAN_POINT ( 'NONE',  ( 74.01132485994280330, 167.7597621252805880, -9.270509831248443078 ) ) ;
#23744 = ORIENTED_EDGE ( 'NONE', *, *, #14300, .F. ) ;
#23745 = CARTESIAN_POINT ( 'NONE',  ( 2.517493886309087436, 199.4062855549015865, 94.59886208192145318 ) ) ;
#23746 = EDGE_CURVE ( 'NONE', #8952, #739, #29767, .T. ) ;
#23747 = CARTESIAN_POINT ( 'NONE',  ( -0.05014649552807731031, 198.5883022060938572, 26.75113791807856956 ) ) ;
#23748 = CARTESIAN_POINT ( 'NONE',  ( 7.500000000000000000, -3.988190556646209028, -0.8526458641284331286 ) ) ;
#23750 = ORIENTED_EDGE ( 'NONE', *, *, #13855, .F. ) ;
#23749 = AXIS2_PLACEMENT_3D ( 'NONE', #5238, #25859, #13399 ) ;
#23751 = CARTESIAN_POINT ( 'NONE',  ( 34.12499999726881583, 155.0000000000000000, 15.58253174999999402 ) ) ;
#23752 = EDGE_CURVE ( 'NONE', #25811, #613, #1221, .T. ) ;
#23753 = CARTESIAN_POINT ( 'NONE',  ( 87.02499999726879309, 149.9369285172503510, -15.58253175000000823 ) ) ;
#23754 = CARTESIAN_POINT ( 'NONE',  ( -4.336808689942017736E-14, -31.75426480542944319, -2.456200930618646971 ) ) ;
#23755 = CARTESIAN_POINT ( 'NONE',  ( -7.984503880673488041, 209.6470497212046098, 87.65113791807857524 ) ) ;
#23756 = DIRECTION ( 'NONE',  ( 1.000000000000000000, 0.000000000000000000, 0.000000000000000000 ) ) ;
#23757 = CARTESIAN_POINT ( 'NONE',  ( 50.89999999999999858, 168.7903194862797420, -4.480746418436745593 ) ) ;
#23758 = CARTESIAN_POINT ( 'NONE',  ( -4.903702542908436435, 200.1653181626580249, 77.04886208192142760 ) ) ;
#23759 = CARTESIAN_POINT ( 'NONE',  ( 115.4999999999999858, 65.35130719884915607, -52.99999999999947420 ) ) ;
#23760 = CARTESIAN_POINT ( 'NONE',  ( 50.22499999726880304, 149.9369285172503510, 15.58253174999999580 ) ) ;
#23761 = PRESENTATION_LAYER_ASSIGNMENT (  '', '', ( #3643 ) ) ;
#23763 = VERTEX_POINT ( 'NONE', #27210 ) ;
#23762 = CARTESIAN_POINT ( 'NONE',  ( -10.00000000000000711, 207.0476921513413515, 15.50113791807856600 ) ) ;
#23764 = DIRECTION ( 'NONE',  ( 0.000000000000000000, 0.000000000000000000, -1.000000000000000000 ) ) ;
#23765 = CARTESIAN_POINT ( 'NONE',  ( 64.02499999726880731, 160.0630714827496206, 15.58253174999999224 ) ) ;
#23766 = CARTESIAN_POINT ( 'NONE',  ( 75.37499999726881583, 155.0000000000000000, -15.58253175000000823 ) ) ;
#23767 = CARTESIAN_POINT ( 'NONE',  ( 11.98450388067348271, 203.0532714938637753, 77.15113791807857524 ) ) ;
#23768 = CARTESIAN_POINT ( 'NONE',  ( -6.746558653882965828, -3.895127454921782029, -6.526045885145518533 ) ) ;
#23769 = CARTESIAN_POINT ( 'NONE',  ( 8.118202686958039038, 212.8392687619912635, 91.70113791807857240 ) ) ;
#23770 = CARTESIAN_POINT ( 'NONE',  ( 53.78867513459483263, 155.0000000000000000, 15.00000000000001243 ) ) ;
#23771 = AXIS2_PLACEMENT_3D ( 'NONE', #9288, #30247, #27185 ) ;
#23772 = VERTEX_POINT ( 'NONE', #3865 ) ;
#23773 = CARTESIAN_POINT ( 'NONE',  ( -0.05014649552828442242, 219.6175466908591716, 54.24886208192143755 ) ) ;
#23774 = CARTESIAN_POINT ( 'NONE',  ( -8.062137200540822946, 201.0835637161416400, 71.19886208192144750 ) ) ;
#23775 = CARTESIAN_POINT ( 'NONE',  ( -12.00000000000000711, 206.9523078486584780, 5.498862081921433997 ) ) ;
#23776 = CARTESIAN_POINT ( 'NONE',  ( 34.18867513459482410, 140.7341522555726669, 4.635254915624211769 ) ) ;
#23777 = CARTESIAN_POINT ( 'NONE',  ( -3.044812012440131443, 216.5253028482142952, 13.10113791807856742 ) ) ;
#23778 = CARTESIAN_POINT ( 'NONE',  ( 6.139770520408223575, 215.5359834540460611, 81.54886208192144181 ) ) ;
#23779 = VERTEX_POINT ( 'NONE', #14258 ) ;
#23780 = CARTESIAN_POINT ( 'NONE',  ( 10.01549611932653860, 210.2015048109876716, 97.85113791807857808 ) ) ;
#23781 = ORIENTED_EDGE ( 'NONE', *, *, #21478, .F. ) ;
#23782 = DIRECTION ( 'NONE',  ( -0.000000000000000000, -0.000000000000000000, 1.000000000000000000 ) ) ;
#23783 = CARTESIAN_POINT ( 'NONE',  ( -8.015496119326597224, 209.5516654185217362, 65.64886208192142192 ) ) ;
#23784 = VECTOR ( 'NONE', #26759, 1000.000000000000000 ) ;
#23785 = ORIENTED_EDGE ( 'NONE', *, *, #14125, .F. ) ;
#23786 = CONICAL_SURFACE ( 'NONE', #29232, 18.00000000000000711, 0.9599310885968802554 ) ;
#23787 = CARTESIAN_POINT ( 'NONE',  ( 75.32499999726881867, 164.1591823560292198, -12.60653300113719766 ) ) ;
#23788 = CARTESIAN_POINT ( 'NONE',  ( 125.5000000000000000, 80.04668119422552763, -74.95331880577366235 ) ) ;
#23789 = VECTOR ( 'NONE', #25008, 1000.000000000000000 ) ;
#23790 = FACE_OUTER_BOUND ( 'NONE', #31853, .T. ) ;
#23791 = CARTESIAN_POINT ( 'NONE',  ( 68.12499999726881583, 155.0000000000000000, 15.58253174999999402 ) ) ;
#23792 = CARTESIAN_POINT ( 'NONE',  ( 4.984841277089725686, 213.7757310962907411, 58.55113791807858092 ) ) ;
#23793 = CIRCLE ( 'NONE', #2042, 2.149999999999985256 ) ;
#23794 = CARTESIAN_POINT ( 'NONE',  ( -9.000000000000005329, 206.8877928634024101, 103.6076739047741029 ) ) ;
#23795 = CARTESIAN_POINT ( 'NONE',  ( 125.5000000000000000, 152.8500000000011028, 106.0000000000000426 ) ) ;
#23796 = CARTESIAN_POINT ( 'NONE',  ( -2.426778023690076225, 199.3768101843759553, 34.89886208192144323 ) ) ;
#23797 = CARTESIAN_POINT ( 'NONE',  ( 8.062137200540920645, 201.0835637161417822, 83.30113791807858092 ) ) ;
#23798 = CARTESIAN_POINT ( 'NONE',  ( 48.71132485994280614, 155.0000000000000000, 15.00000000000001243 ) ) ;
#23799 = CARTESIAN_POINT ( 'NONE',  ( -0.05014649552810635652, 196.4853777576173002, 68.75113791807855534 ) ) ;
#23800 = DIRECTION ( 'NONE',  ( 0.000000000000000000, 0.000000000000000000, -1.000000000000000000 ) ) ;
#23801 = CARTESIAN_POINT ( 'NONE',  ( -6.444103211791042618, 211.7408657792732356, 18.80113791807856671 ) ) ;
#23802 = DIRECTION ( 'NONE',  ( 0.000000000000000000, -1.000000000000000000, 0.000000000000000000 ) ) ;
#23803 = FACE_OUTER_BOUND ( 'NONE', #7232, .T. ) ;
#23804 = CARTESIAN_POINT ( 'NONE',  ( 41.82499999726881157, 168.2552932293087906, 9.630534252274372875 ) ) ;
#23805 = CARTESIAN_POINT ( 'NONE',  ( 7.456977232089302632, 217.1783343296989131, 37.55113791807855961 ) ) ;
#23806 = DIRECTION ( 'NONE',  ( -0.000000000000000000, -0.000000000000000000, 1.000000000000000000 ) ) ;
#23807 = CARTESIAN_POINT ( 'NONE',  ( -8.062137200540920645, 212.9164362838581894, 96.80113791807858092 ) ) ;
#23808 = CARTESIAN_POINT ( 'NONE',  ( 6.139770520408367460, 198.4640165459539389, 59.45113791807856529 ) ) ;
#23809 = AXIS2_PLACEMENT_3D ( 'NONE', #9836, #14759, #15104 ) ;
#23810 = CARTESIAN_POINT ( 'NONE',  ( -11.98450388067341876, 203.0532714938636047, 26.34886208192143897 ) ) ;
#23811 = CARTESIAN_POINT ( 'NONE',  ( -6.220909254589682469, 215.4770327129947134, 41.94886208192144039 ) ) ;
#23812 = CARTESIAN_POINT ( 'NONE',  ( 82.79999999453762882, 163.5228861582408797, 11.73074641843673049 ) ) ;
#23813 = MANIFOLD_SOLID_BREP ( 'EndChamfer', #30281 ) ;
#23814 = CARTESIAN_POINT ( 'NONE',  ( -7.375838497908182134, 217.2372850707499765, 63.95113791807857240 ) ) ;
#23815 = CARTESIAN_POINT ( 'NONE',  ( 2.426778023690261410, 199.3768101843759837, 89.60113791807857808 ) ) ;
#23816 = CARTESIAN_POINT ( 'NONE',  ( -6.139770520408224463, 198.4640165459539389, 47.04886208192142050 ) ) ;
#23817 = CARTESIAN_POINT ( 'NONE',  ( 49.08867513459482979, 167.7597621252805880, -9.270509831248443078 ) ) ;
#23818 = VECTOR ( 'NONE', #1515, 1000.000000000000000 ) ;
#23819 = ORIENTED_EDGE ( 'NONE', *, *, #30981, .F. ) ;
#23820 = CARTESIAN_POINT ( 'NONE',  ( -11.98450388067341876, 203.0532714938636047, 50.34886208192144608 ) ) ;
#23821 = ORIENTED_EDGE ( 'NONE', *, *, #18949, .F. ) ;
#23822 = EDGE_LOOP ( 'NONE', ( #2995, #26284 ) ) ;
#23823 = CARTESIAN_POINT ( 'NONE',  ( 75.77499999726880731, 169.8198683612136222, -4.815267126137197984 ) ) ;
#23824 = CARTESIAN_POINT ( 'NONE',  ( 52.71132485994279904, 155.0000000000000000, 15.00000000000001243 ) ) ;
#23825 = DIRECTION ( 'NONE',  ( 1.000000000000000000, 0.000000000000000000, 0.000000000000000000 ) ) ;
#23826 = CARTESIAN_POINT ( 'NONE',  ( 2.517493886308900919, 214.5937144450984420, 43.40113791807856813 ) ) ;
#23827 = AXIS2_PLACEMENT_3D ( 'NONE', #25298, #25973, #14906 ) ;
#23828 = EDGE_CURVE ( 'NONE', #11491, #14565, #31432, .T. ) ;
#23829 = VECTOR ( 'NONE', #1451, 1000.000000000000114 ) ;
#23830 = CARTESIAN_POINT ( 'NONE',  ( 6.139770520408223575, 215.5359834540460611, 27.54886208192142760 ) ) ;
#23831 = CARTESIAN_POINT ( 'NONE',  ( 60.57499999726881157, 145.8408176439707802, 12.60653300113718345 ) ) ;
#23832 = VERTEX_POINT ( 'NONE', #23116 ) ;
#23833 = CARTESIAN_POINT ( 'NONE',  ( 62.58867513459481557, 146.1832212156128890, -12.13525491562423042 ) ) ;
#23834 = CARTESIAN_POINT ( 'NONE',  ( -7.500000000000000000, -4.330127018922198090, -10.00000000000000000 ) ) ;
#23835 = CARTESIAN_POINT ( 'NONE',  ( 6.444103211790928043, 211.7408657792734061, 3.698862081921435063 ) ) ;
#23836 = CARTESIAN_POINT ( 'NONE',  ( 8.062137200540920645, 201.0835637161417822, 53.30113791807857382 ) ) ;
#23837 = CARTESIAN_POINT ( 'NONE',  ( 83.48867513459482836, 167.7597621252805880, 9.270509831248428867 ) ) ;
#23838 = CARTESIAN_POINT ( 'NONE',  ( 10.01549611932653860, 210.2015048109876716, 25.85113791807856742 ) ) ;
#23839 = CARTESIAN_POINT ( 'NONE',  ( 82.37499999726881583, 155.0000000000000000, 15.58253174999999402 ) ) ;
#23840 = AXIS2_PLACEMENT_3D ( 'NONE', #2866, #2713, #20594 ) ;
#23841 = APPLICATION_PROTOCOL_DEFINITION ( 'draft international standard', 'automotive_design', 1998, #3757 ) ;
#23842 = CARTESIAN_POINT ( 'NONE',  ( -4.903702542908436435, 200.1653181626580249, 95.04886208192144181 ) ) ;
#23843 = CARTESIAN_POINT ( 'NONE',  ( 39.02499999726880731, 149.9369285172503510, -15.58253175000000823 ) ) ;
#23844 = CARTESIAN_POINT ( 'NONE',  ( 8.000000000000000000, 0.000000000000000000, -4.400000000000001243 ) ) ;
#23845 = CARTESIAN_POINT ( 'NONE',  ( 7.375838497908181246, 196.7627149292499666, 8.451137918078563516 ) ) ;
#23846 = CARTESIAN_POINT ( 'NONE',  ( -125.0000000000000000, 25.00000000000000000, -35.00000000000000000 ) ) ;
#23847 = CARTESIAN_POINT ( 'NONE',  ( 55.47499999726881015, 160.0630714827496206, -15.58253175000000823 ) ) ;
#23848 = CARTESIAN_POINT ( 'NONE',  ( -10.01549611932653860, 203.7984951890123284, 60.35113791807857808 ) ) ;
#23849 = CARTESIAN_POINT ( 'NONE',  ( -6.220909254589537696, 198.5229672870051445, 27.05113791807856671 ) ) ;
#23850 = DIRECTION ( 'NONE',  ( 1.000000000000000000, 0.000000000000000000, 0.000000000000000000 ) ) ;
#23851 = CARTESIAN_POINT ( 'NONE',  ( 5.000000000000000000, -5.258101095580058680E-15, -4.057500000000000107 ) ) ;
#23852 = CARTESIAN_POINT ( 'NONE',  ( -125.0000000000000000, 25.00000000000000000, 35.00000000000000000 ) ) ;
#23853 = CARTESIAN_POINT ( 'NONE',  ( 59.99999999453763166, 155.0000000000000000, -14.50000000000000711 ) ) ;
#23854 = EDGE_LOOP ( 'NONE', ( #8780, #26672 ) ) ;
#23855 = CARTESIAN_POINT ( 'NONE',  ( 7.375838497908181246, 196.7627149292499666, 35.45113791807855819 ) ) ;
#23856 = AXIS2_PLACEMENT_3D ( 'NONE', #9818, #4023, #4696 ) ;
#23857 = CARTESIAN_POINT ( 'NONE',  ( 115.4999999999999858, 246.7986928011511907, 52.99999999999882760 ) ) ;
#23858 = CARTESIAN_POINT ( 'NONE',  ( 3.135527875058981895, 197.5041725223112792, 25.59886208192143897 ) ) ;
#23859 = CIRCLE ( 'NONE', #21671, 4.199999999999988631 ) ;
#23860 = CARTESIAN_POINT ( 'NONE',  ( 72.51132485994280330, 163.8167787843871110, 12.13525491562421621 ) ) ;
#23861 = ORIENTED_EDGE ( 'NONE', *, *, #15348, .T. ) ;
#23862 = AXIS2_PLACEMENT_3D ( 'NONE', #28112, #33051, #15168 ) ;
#23863 = CARTESIAN_POINT ( 'NONE',  ( -3.135527875058821579, 197.5041725223112223, 80.90113791807858945 ) ) ;
#23864 = VERTEX_POINT ( 'NONE', #10176 ) ;
#23865 = AXIS2_PLACEMENT_3D ( 'NONE', #12626, #7363, #22516 ) ;
#23866 = CARTESIAN_POINT ( 'NONE',  ( 0.000000000000000000, 0.000000000000000000, 0.000000000000000000 ) ) ;
#23867 = CARTESIAN_POINT ( 'NONE',  ( 43.81132485994280046, 159.8737954434936341, -15.00000000000000355 ) ) ;
#23868 = VERTEX_POINT ( 'NONE', #12383 ) ;
#23869 = CARTESIAN_POINT ( 'NONE',  ( 7.984503880673485376, 204.3529502787953902, 14.15113791807856991 ) ) ;
#23870 = CARTESIAN_POINT ( 'NONE',  ( -60.66959905230670103, 194.9806057094332346, 1.252942659870247555 ) ) ;
#23871 = ADVANCED_FACE ( 'NONE', ( #17326 ), #1485, .T. ) ;
#23872 = CARTESIAN_POINT ( 'NONE',  ( 0.05014649552828288198, 194.3824533091408000, 97.74886208192141623 ) ) ;
#23873 = CARTESIAN_POINT ( 'NONE',  ( 44.47499999726880304, 149.9369285172503510, 15.58253174999999580 ) ) ;
#23874 = ORIENTED_EDGE ( 'NONE', *, *, #335, .F. ) ;
#23875 = CARTESIAN_POINT ( 'NONE',  ( 48.52499999726880731, 140.1801316387863778, 4.815267126137185549 ) ) ;
#23876 = CARTESIAN_POINT ( 'NONE',  ( 64.50000000000000000, 0.000000000000000000, 20.00000000000000000 ) ) ;
#23877 = FACE_OUTER_BOUND ( 'NONE', #13179, .T. ) ;
#23878 = ADVANCED_FACE ( 'NONE', ( #10012, #9656 ), #25326, .T. ) ;
#23879 = CARTESIAN_POINT ( 'NONE',  ( -9.984503880673420539, 203.7031108863293980, 83.34886208192139634 ) ) ;
#23880 = CARTESIAN_POINT ( 'NONE',  ( 56.07499999726881157, 168.2552932293087906, 9.630534252274372875 ) ) ;
#23881 = CARTESIAN_POINT ( 'NONE',  ( 8.118202686958039038, 212.8392687619912635, 22.70113791807856884 ) ) ;
#23882 = DIRECTION ( 'NONE',  ( 0.000000000000000000, 0.000000000000000000, -1.000000000000000000 ) ) ;
#23883 = EDGE_CURVE ( 'NONE', #12782, #25798, #27592, .T. ) ;
#23884 = VECTOR ( 'NONE', #3051, 1000.000000000000000 ) ;
#23885 = CONTEXT_DEPENDENT_SHAPE_REPRESENTATION ( #18144, #8185 ) ;
#23886 = CARTESIAN_POINT ( 'NONE',  ( 76.89999999999999147, 168.7903194862797420, -4.480746418436745593 ) ) ;
#23887 = CARTESIAN_POINT ( 'NONE',  ( -125.0000000000000000, 25.00000000000000000, -35.00000000000000000 ) ) ;
#23888 = CARTESIAN_POINT ( 'NONE',  ( 115.4999999999999858, 102.0000000000001990, 91.79869280115065067 ) ) ;
#23889 = CARTESIAN_POINT ( 'NONE',  ( 6.139770520408368348, 198.4640165459539674, 80.45113791807857240 ) ) ;
#23890 = CARTESIAN_POINT ( 'NONE',  ( 57.68867513459482410, 159.8737954434937478, 14.99999999999991651 ) ) ;
#23891 = CARTESIAN_POINT ( 'NONE',  ( 41.17499999726881299, 145.8408176439707802, -12.60653300113719588 ) ) ;
#23892 = CARTESIAN_POINT ( 'NONE',  ( -12.01549611932659722, 210.8513442034533227, 98.64886208192146455 ) ) ;
#23893 = CIRCLE ( 'NONE', #21095, 5.000000000000000888 ) ;
#23894 = CARTESIAN_POINT ( 'NONE',  ( 77.02499999726880731, 149.9369285172503510, -15.58253175000000823 ) ) ;
#23895 = ORIENTED_EDGE ( 'NONE', *, *, #33053, .T. ) ;
#23896 = DIRECTION ( 'NONE',  ( -1.000000000000000000, 0.000000000000000000, 0.000000000000000000 ) ) ;
#23897 = CARTESIAN_POINT ( 'NONE',  ( 40.79999999453762882, 163.5228861582408797, 11.73074641843673049 ) ) ;
#23898 = ADVANCED_FACE ( 'NONE', ( #33339 ), #23786, .F. ) ;
#23899 = DIRECTION ( 'NONE',  ( -1.000000000000000000, 0.000000000000000000, 0.000000000000000000 ) ) ;
#23900 = B_SPLINE_CURVE_WITH_KNOTS ( 'NONE', 3,
 ( #27910, #9516, #32853, #19903, #33016, #1680 ),
 .UNSPECIFIED., .F., .F.,
 ( 4, 2, 4 ),
 ( 8.673617379884035472E-19, 0.0003352299596252132619, 0.0006704599192504256564 ),
 .UNSPECIFIED. ) ;
#23901 = CARTESIAN_POINT ( 'NONE',  ( -0.3306966981848578069, -8.469326210127253063, -7.349897473154448413 ) ) ;
#23902 = ORIENTED_EDGE ( 'NONE', *, *, #12635, .F. ) ;
#23903 = CARTESIAN_POINT ( 'NONE',  ( 0.05014649552828275014, 196.4853777576173002, 91.74886208192144466 ) ) ;
#23904 = CARTESIAN_POINT ( 'NONE',  ( -7.456977232089471386, 217.1783343296987709, 32.94886208192144039 ) ) ;
#23905 = CARTESIAN_POINT ( 'NONE',  ( 117.5000000000000000, 155.0000000000000000, -6.938893903907228378E-15 ) ) ;
#23906 = CONICAL_SURFACE ( 'NONE', #32075, 1.535500000000000087, 1.047197551196590748 ) ;
#23907 = CARTESIAN_POINT ( 'NONE',  ( 6.139770520408368348, 198.4640165459539674, 56.45113791807857950 ) ) ;
#23908 = EDGE_CURVE ( 'NONE', #6774, #15657, #8046, .T. ) ;
#23909 = ORIENTED_EDGE ( 'NONE', *, *, #32599, .T. ) ;
#23910 = CARTESIAN_POINT ( 'NONE',  ( -8.015496119326597224, 209.5516654185217362, 2.648862081921435241 ) ) ;
#23911 = CARTESIAN_POINT ( 'NONE',  ( 7.331804101520335523E-16, -31.75426480542945740, -18.00000000000000000 ) ) ;
#23912 = ORIENTED_EDGE ( 'NONE', *, *, #30631, .T. ) ;
#23913 = CARTESIAN_POINT ( 'NONE',  ( -6.444103211790928043, 202.2591342207265939, 95.19886208192144750 ) ) ;
#23914 = CARTESIAN_POINT ( 'NONE',  ( 6.444103211791042618, 202.2591342207267644, 32.30113791807856671 ) ) ;
#23915 = CARTESIAN_POINT ( 'NONE',  ( 0.000000000000000000, 0.000000000000000000, -2.899999999999999911 ) ) ;
#23916 = EDGE_LOOP ( 'NONE', ( #21221, #24408, #26618, #24605 ) ) ;
#23917 = CARTESIAN_POINT ( 'NONE',  ( 34.62499999726880873, 138.6155565068815463, -3.929120461958505118E-15 ) ) ;
#23918 = CARTESIAN_POINT ( 'NONE',  ( 86.62499999726883004, 138.6155565068815463, -3.929120461958505118E-15 ) ) ;
#23919 = DIRECTION ( 'NONE',  ( -0.000000000000000000, -0.000000000000000000, 1.000000000000000000 ) ) ;
#23920 = CARTESIAN_POINT ( 'NONE',  ( 2.426778023690261410, 199.3768101843759837, 101.6011379180785781 ) ) ;
#23921 = DIRECTION ( 'NONE',  ( 0.000000000000000000, -0.8660254037844401509, -0.4999999999999977796 ) ) ;
#23922 = CARTESIAN_POINT ( 'NONE',  ( 54.00000000000000000, 139.7537977485451393, -4.138211985947621020E-15 ) ) ;
#23923 = CARTESIAN_POINT ( 'NONE',  ( 6.500168698208244500, 202.3363017425938324, 70.29886208192142760 ) ) ;
#23924 = TOROIDAL_SURFACE ( 'NONE', #19576, 4.999999999999993783, 1.000000000000000222 ) ;
#23925 = CARTESIAN_POINT ( 'NONE',  ( 27.50000000000000000, -14.58598892539967906, -2.083479913523504923 ) ) ;
#23926 =( BOUNDED_CURVE ( )  B_SPLINE_CURVE ( 2, ( #21174, #565, #21678, #8730, #19121, #16559, #5672, #5999, #8565, #8894, #893 ),
 .UNSPECIFIED., .F., .T. ) 
 B_SPLINE_CURVE_WITH_KNOTS ( ( 3, 2, 2, 2, 2, 3 ),
 ( 0.1071428571428571092, 0.1107142857142856818, 0.1142857142857142544, 0.1178571428571428270, 0.1214285714285713996, 0.1249999999999999722 ),
 .UNSPECIFIED. ) 
 CURVE ( )  GEOMETRIC_REPRESENTATION_ITEM ( )  RATIONAL_B_SPLINE_CURVE ( ( 1.000000000000000444, 0.9510565162951530871, 1.000000000000000000, 0.9510565162951534202, 1.000000000000000000, 0.9510565162951534202, 1.000000000000000000, 0.9510565162951534202, 1.000000000000000000, 0.9510565162951537532, 0.9999999999999996669 ) ) 
 REPRESENTATION_ITEM ( '' )  );
#23927 = EDGE_CURVE ( 'NONE', #2969, #10366, #12213, .T. ) ;
#23928 = CARTESIAN_POINT ( 'NONE',  ( 60.12499999726880873, 155.0000000000000000, 15.58253174999999402 ) ) ;
#23930 = ORIENTED_EDGE ( 'NONE', *, *, #28938, .F. ) ;
#23929 = CARTESIAN_POINT ( 'NONE',  ( 0.05014649552810506589, 217.5146222423826714, 10.25113791807856600 ) ) ;
#23931 = DIRECTION ( 'NONE',  ( 0.000000000000000000, 1.000000000000000000, -1.224646799147353207E-16 ) ) ;
#23932 = CARTESIAN_POINT ( 'NONE',  ( 62.32499999726881867, 145.8408176439707802, 12.60653300113718345 ) ) ;
#23933 = CARTESIAN_POINT ( 'NONE',  ( 78.97499999726881015, 140.1801316387863778, -4.815267126137194431 ) ) ;
#23934 = CARTESIAN_POINT ( 'NONE',  ( -12.01549611932652972, 203.1486557965464499, 75.35113791807856387 ) ) ;
#23935 = CYLINDRICAL_SURFACE ( 'NONE', #27684, 15.00000000000001776 ) ;
#23936 = ADVANCED_FACE ( 'NONE', ( #22600 ), #22779, .T. ) ;
#23937 = CARTESIAN_POINT ( 'NONE',  ( -3.044812012440131443, 216.5253028482142952, 97.10113791807857808 ) ) ;
#23938 = CARTESIAN_POINT ( 'NONE',  ( 53.68867513459483121, 159.8737954434933499, 15.00000000000019895 ) ) ;
#23939 = ORIENTED_EDGE ( 'NONE', *, *, #6818, .F. ) ;
#23940 = CARTESIAN_POINT ( 'NONE',  ( -3.753561863808878130, 218.3979405102790281, 63.09886208192143187 ) ) ;
#23941 = CARTESIAN_POINT ( 'NONE',  ( -9.984503880673420539, 203.7031108863293980, 65.34886208192143897 ) ) ;
#23942 = CARTESIAN_POINT ( 'NONE',  ( -11.98450388067341876, 203.0532714938636047, 8.348862081921435419 ) ) ;
#23943 = DIRECTION ( 'NONE',  ( 0.000000000000000000, -1.000000000000000000, 0.000000000000000000 ) ) ;
#23944 = CARTESIAN_POINT ( 'NONE',  ( -6.220909254589537696, 198.5229672870051161, 9.051137918078561384 ) ) ;
#23945 = EDGE_CURVE ( 'NONE', #780, #27878, #33044, .T. ) ;
#23946 = CARTESIAN_POINT ( 'NONE',  ( -10.00000000000000711, 206.9523078486584495, 80.49886208192143044 ) ) ;
#23947 = ORIENTED_EDGE ( 'NONE', *, *, #3537, .T. ) ;
#23948 = CARTESIAN_POINT ( 'NONE',  ( -3.135527875058821579, 197.5041725223112223, 95.90113791807858945 ) ) ;
#23949 = ORIENTED_EDGE ( 'NONE', *, *, #15294, .T. ) ;
#23950 = CARTESIAN_POINT ( 'NONE',  ( 2.000000000000000000, -1.773042676681340524, 1.734723475976807094E-15 ) ) ;
#23951 = CARTESIAN_POINT ( 'NONE',  ( -4.903702542908436435, 200.1653181626580249, 59.04886208192144181 ) ) ;
#23952 = ORIENTED_EDGE ( 'NONE', *, *, #624, .F. ) ;
#23953 = CARTESIAN_POINT ( 'NONE',  ( 77.42499999726881299, 168.2552932293087906, -9.630534252274387086 ) ) ;
#23954 = ORIENTED_EDGE ( 'NONE', *, *, #16795, .T. ) ;
#23955 = CARTESIAN_POINT ( 'NONE',  ( -0.3755270751584372513, 206.7692714347155629, 108.3323677711371573 ) ) ;
#23956 = DIRECTION ( 'NONE',  ( -1.000000000000000000, -0.000000000000000000, -0.000000000000000000 ) ) ;
#23957 = UNCERTAINTY_MEASURE_WITH_UNIT (LENGTH_MEASURE( 1.000000000000000082E-05 ), #24849, 'distance_accuracy_value', 'NONE');
#23958 = CARTESIAN_POINT ( 'NONE',  ( 70.62499999726881583, 138.6155565068815463, -3.929120461958505118E-15 ) ) ;
#23959 = CARTESIAN_POINT ( 'NONE',  ( -7.984503880673488041, 209.6470497212046098, 60.65113791807856813 ) ) ;
#23960 =( LENGTH_UNIT ( ) NAMED_UNIT ( * ) SI_UNIT ( .MILLI., .METRE. ) );
#23961 = DIRECTION ( 'NONE',  ( 0.000000000000000000, 0.000000000000000000, 1.000000000000000000 ) ) ;
#23962 = CONICAL_SURFACE ( 'NONE', #14720, 4.174999999999999822, 0.9599310885968795892 ) ;
#23963 = CARTESIAN_POINT ( 'NONE',  ( 33.20000000000000284, 167.3344367211045096, 8.961492836873468093 ) ) ;
#23964 = CARTESIAN_POINT ( 'NONE',  ( 6.444103211790928043, 211.7408657792734061, 45.69886208192144750 ) ) ;
#23965 = CARTESIAN_POINT ( 'NONE',  ( 8.118202686958039038, 212.8392687619912635, 76.70113791807857240 ) ) ;
#23966 = CARTESIAN_POINT ( 'NONE',  ( 10.00000000000000711, 206.9523078486586201, 62.00113791807856956 ) ) ;
#23967 = ADVANCED_FACE ( 'NONE', ( #30616 ), #30448, .T. ) ;
#23968 = FACE_BOUND ( 'NONE', #7959, .T. ) ;
#23969 = CARTESIAN_POINT ( 'NONE',  ( -7.984503880673488041, 209.6470497212046098, 15.65113791807856636 ) ) ;
#23970 = CARTESIAN_POINT ( 'NONE',  ( 10.00000000000000178, 0.000000000000000000, 8.000000000000000000 ) ) ;
#23971 = CARTESIAN_POINT ( 'NONE',  ( 0.2259792476677715822, 7.636022678937395725, -6.470294263593361350 ) ) ;
#23972 = CARTESIAN_POINT ( 'NONE',  ( 44.92499999726880588, 145.8408176439707802, -12.60653300113719588 ) ) ;
#23973 = CARTESIAN_POINT ( 'NONE',  ( -12.01549611932652972, 203.1486557965464499, 45.35113791807857098 ) ) ;
#23974 = CARTESIAN_POINT ( 'NONE',  ( 115.4999999999999858, 207.9999999999998010, -91.79869280115066488 ) ) ;
#23975 = EDGE_CURVE ( 'NONE', #22995, #27125, #4712, .T. ) ;
#23976 = CARTESIAN_POINT ( 'NONE',  ( -3.044812012440131443, 216.5253028482142952, 91.10113791807857808 ) ) ;
#23977 = EDGE_CURVE ( 'NONE', #4327, #15528, #3667, .T. ) ;
#23978 = CARTESIAN_POINT ( 'NONE',  ( -8.062137200540920645, 212.9164362838581894, 66.80113791807858092 ) ) ;
#23979 = CARTESIAN_POINT ( 'NONE',  ( 3.662846001189864698, 218.4274158808046593, 33.39886208192143613 ) ) ;
#23980 = CARTESIAN_POINT ( 'NONE',  ( 3.044812012439969795, 216.5253028482143520, 36.39886208192142902 ) ) ;
#23981 = CARTESIAN_POINT ( 'NONE',  ( 78.59999999453762598, 168.7903194862797420, 4.480746418436729606 ) ) ;
#23982 = MANIFOLD_SOLID_BREP ( '\X2\00d8\X0\8.4 (8.4) Diameter Hole1', #17763 ) ;
#23983 = CARTESIAN_POINT ( 'NONE',  ( -7.375838497908182134, 217.2372850707499765, 78.95113791807858661 ) ) ;
#23984 = CARTESIAN_POINT ( 'NONE',  ( 6.444103211791042618, 202.2591342207267644, 86.30113791807858092 ) ) ;
#23985 = CARTESIAN_POINT ( 'NONE',  ( 3.044812012439969795, 216.5253028482143520, 51.39886208192143613 ) ) ;
#23986 = LINE ( 'NONE', #13100, #19426 ) ;
#23987 = ORIENTED_EDGE ( 'NONE', *, *, #4342, .T. ) ;
#23988 = CARTESIAN_POINT ( 'NONE',  ( 9.736236675708031640, 199.9851607334238963, 52.29886208192143471 ) ) ;
#23989 = ORIENTED_EDGE ( 'NONE', *, *, #13443, .F. ) ;
#23990 = VERTEX_POINT ( 'NONE', #8447 ) ;
#23991 = CARTESIAN_POINT ( 'NONE',  ( 75.57499999726881867, 164.1591823560292198, -12.60653300113719766 ) ) ;
#23992 = CARTESIAN_POINT ( 'NONE',  ( 53.01132485994281751, 142.2402378747194405, 9.270509831248432420 ) ) ;
#23993 = CARTESIAN_POINT ( 'NONE',  ( 117.5000000000000000, 207.9999999999998010, -91.79869280115066488 ) ) ;
#23994 = CARTESIAN_POINT ( 'NONE',  ( 4.903702542908601636, 200.1653181626581102, 53.45113791807857950 ) ) ;
#23995 = CARTESIAN_POINT ( 'NONE',  ( 2.346298152288388117, -2.686816014504594730, -2.899999999999981704 ) ) ;
#23996 =( REPRESENTATION_RELATIONSHIP ('NONE','NONE', #25663, #22175 ) REPRESENTATION_RELATIONSHIP_WITH_TRANSFORMATION ( #19396 )SHAPE_REPRESENTATION_RELATIONSHIP( ) );
#23997 = CARTESIAN_POINT ( 'NONE',  ( 8.118202686958138514, 201.1607312380088501, 34.29886208192143471 ) ) ;
#23998 = CARTESIAN_POINT ( 'NONE',  ( 67.87499999726881583, 171.3844434931184253, -7.942151717890134290E-15 ) ) ;
#23999 = EDGE_LOOP ( 'NONE', ( #8616, #22990 ) ) ;
#24000 = CARTESIAN_POINT ( 'NONE',  ( 67.98867513459482836, 146.1832212156128890, 12.13525491562421976 ) ) ;
#24001 = DIRECTION ( 'NONE',  ( -0.000000000000000000, -0.000000000000000000, -1.000000000000000000 ) ) ;
#24002 = CARTESIAN_POINT ( 'NONE',  ( 8.000000000000008882, 207.0476921513415220, 12.99886208192143400 ) ) ;
#24003 = CARTESIAN_POINT ( 'NONE',  ( -8.118202686958039038, 201.1607312380087080, 48.20113791807857950 ) ) ;
#24004 = CARTESIAN_POINT ( 'NONE',  ( 80.21132485994280614, 170.7719333635740497, -7.904646289410545231E-15 ) ) ;
#24005 = CARTESIAN_POINT ( 'NONE',  ( 3.135527875058820690, 216.4958274776887492, 40.40113791807857524 ) ) ;
#24006 = CARTESIAN_POINT ( 'NONE',  ( 85.77499999726880731, 169.8198683612136222, -4.815267126137197984 ) ) ;
#24007 = ITEM_DEFINED_TRANSFORMATION ( 'NONE', 'NONE', #15911,  #2404 ) ;
#24008 = AXIS2_PLACEMENT_3D ( 'NONE', #4624, #25063, #4276 ) ;
#24009 = CARTESIAN_POINT ( 'NONE',  ( -4.984841277089891776, 213.7757310962905990, 95.94886208192144750 ) ) ;
#24010 = CARTESIAN_POINT ( 'NONE',  ( 40.72499999726881725, 140.1801316387863778, -4.815267126137194431 ) ) ;
#24011 = CARTESIAN_POINT ( 'NONE',  ( -7.922281120364393914, -4.573931137438277617, -8.047472243342932430 ) ) ;
#24012 = LINE ( 'NONE', #13952, #20719 ) ;
#24013 = CARTESIAN_POINT ( 'NONE',  ( -0.05014649552807705357, 194.3824533091408000, 17.75113791807856956 ) ) ;
#24014 = CARTESIAN_POINT ( 'NONE',  ( 60.63708498984762940, 155.0000000000000000, -40.00000000000000000 ) ) ;
#24015 = CARTESIAN_POINT ( 'NONE',  ( 56.17499999726881299, 164.1591823560292198, 12.60653300113718167 ) ) ;
#24016 = CARTESIAN_POINT ( 'NONE',  ( -0.05014649552810635652, 196.4853777576173002, 62.75113791807856956 ) ) ;
#24017 = CARTESIAN_POINT ( 'NONE',  ( 10.01549611932653860, 210.2015048109876716, 40.85113791807857098 ) ) ;
#24018 = EDGE_CURVE ( 'NONE', #20656, #24119, #19922, .T. ) ;
#24019 = CARTESIAN_POINT ( 'NONE',  ( -67.50000000000000000, 155.0000000000000000, -37.00000000000000000 ) ) ;
#24020 = DIRECTION ( 'NONE',  ( 0.000000000000000000, 0.000000000000000000, -1.000000000000000000 ) ) ;
#24021 = CARTESIAN_POINT ( 'NONE',  ( -9.984503880673420539, 203.7031108863293980, 5.348862081921434530 ) ) ;
#24022 = CARTESIAN_POINT ( 'NONE',  ( 61.59999999453763309, 141.2096805137202580, -4.480746418436742040 ) ) ;
#24023 = EDGE_LOOP ( 'NONE', ( #18968, #6092, #30910, #11064 ) ) ;
#24024 = CARTESIAN_POINT ( 'NONE',  ( 11.98450388067348271, 203.0532714938637753, 53.15113791807857524 ) ) ;
#24025 = CARTESIAN_POINT ( 'NONE',  ( -58.50000000000001421, -88.00000000000000000, -20.00000000000000000 ) ) ;
#24026 = CARTESIAN_POINT ( 'NONE',  ( 10.01549611932659545, 203.7984951890123853, 22.14886208192143613 ) ) ;
#24027 = ORIENTED_EDGE ( 'NONE', *, *, #1411, .F. ) ;
#24028 = CARTESIAN_POINT ( 'NONE',  ( 6.139770520408368348, 198.4640165459539674, 83.45113791807858661 ) ) ;
#24029 = EDGE_LOOP ( 'NONE', ( #18181, #18346, #22869, #2171 ) ) ;
#24030 = CARTESIAN_POINT ( 'NONE',  ( 50.61132485994281893, 159.8737954434936057, 15.00000000000001421 ) ) ;
#24031 = CARTESIAN_POINT ( 'NONE',  ( 64.50000000000000000, 0.000000000000000000, -20.00000000000000000 ) ) ;
#24032 = ORIENTED_EDGE ( 'NONE', *, *, #18744, .T. ) ;
#24033 = CARTESIAN_POINT ( 'NONE',  ( -4.903702542908602524, 213.8346818373418898, 21.95113791807856884 ) ) ;
#24034 = CARTESIAN_POINT ( 'NONE',  ( -60.74722861894645831, 194.9849492171461804, 1.107464383744043657 ) ) ;
#24035 = CARTESIAN_POINT ( 'NONE',  ( -3.044812012439970683, 197.4746971517856196, 7.898862081921434353 ) ) ;
#24036 = CARTESIAN_POINT ( 'NONE',  ( 41.57499999726881157, 164.1591823560292198, -12.60653300113719766 ) ) ;
#24037 = ORIENTED_EDGE ( 'NONE', *, *, #7473, .T. ) ;
#24038 = CARTESIAN_POINT ( 'NONE',  ( 50.52499999726880731, 140.1801316387863778, 4.815267126137185549 ) ) ;
#24039 = LINE ( 'NONE', #707, #33315 ) ;
#24040 = AXIS2_PLACEMENT_3D ( 'NONE', #32585, #22540, #7041 ) ;
#24041 = DIRECTION ( 'NONE',  ( 0.000000000000000000, 0.000000000000000000, -1.000000000000000000 ) ) ;
#24042 = CARTESIAN_POINT ( 'NONE',  ( 9.984503880673420539, 210.2968891136705167, 84.84886208192143897 ) ) ;
#24043 = CARTESIAN_POINT ( 'NONE',  ( 51.87499999726880162, 171.3844434931184253, -7.942151717890132712E-15 ) ) ;
#24044 = CARTESIAN_POINT ( 'NONE',  ( -6.139770520408369237, 215.5359834540460042, 24.95113791807855819 ) ) ;
#24045 = CARTESIAN_POINT ( 'NONE',  ( -52.50000000000002132, 155.0000000000000000, 17.00000000000001066 ) ) ;
#24046 = CARTESIAN_POINT ( 'NONE',  ( -7.456977232089471386, 217.1783343296987709, 83.94886208192144750 ) ) ;
#24047 = CARTESIAN_POINT ( 'NONE',  ( 76.00000000000002842, 139.7537977485451393, -4.138211985947621020E-15 ) ) ;
#24048 = CARTESIAN_POINT ( 'NONE',  ( 107.9108275708642850, 155.0000000000000000, 0.000000000000000000 ) ) ;
#24049 = DIRECTION ( 'NONE',  ( -1.000000000000000000, 0.000000000000000000, 0.000000000000000000 ) ) ;
#24050 = CARTESIAN_POINT ( 'NONE',  ( 6.220909254589536808, 215.4770327129947702, 82.55113791807858092 ) ) ;
#24051 = CARTESIAN_POINT ( 'NONE',  ( 33.78867513459482552, 155.0000000000000000, 15.00000000000001243 ) ) ;
#24052 = CARTESIAN_POINT ( 'NONE',  ( 35.57499999726881157, 164.1591823560292198, -12.60653300113719766 ) ) ;
#24053 = CARTESIAN_POINT ( 'NONE',  ( 6.220909254589536808, 215.4770327129947702, 37.55113791807856671 ) ) ;
#24054 = CARTESIAN_POINT ( 'NONE',  ( 78.42499999726882720, 141.7447067706911810, 9.630534252274376428 ) ) ;
#24055 = VERTEX_POINT ( 'NONE', #18512 ) ;
#24056 = PRODUCT_DEFINITION_FORMATION_WITH_SPECIFIED_SOURCE ( 'ANY', '', #16751, .NOT_KNOWN. ) ;
#24057 = CARTESIAN_POINT ( 'NONE',  ( 47.81132485994282177, 159.8737954434935489, -15.00000000000007638 ) ) ;
#24058 = CARTESIAN_POINT ( 'NONE',  ( 41.19999999453762740, 146.4771138417591203, 11.73074641843673227 ) ) ;
#24059 = CARTESIAN_POINT ( 'NONE',  ( 12.00000000000000711, 206.9523078486586485, 8.001137918078566003 ) ) ;
#24060 = DIRECTION ( 'NONE',  ( -1.000000000000000000, 0.000000000000000000, 0.000000000000000000 ) ) ;
#24061 = EDGE_CURVE ( 'NONE', #25811, #12674, #25245, .T. ) ;
#24062 = CARTESIAN_POINT ( 'NONE',  ( -6.484173630544109557, -4.916614646775610886, -7.642786413610934915 ) ) ;
#24063 = VERTEX_POINT ( 'NONE', #5224 ) ;
#24064 = CARTESIAN_POINT ( 'NONE',  ( 8.062137200540822946, 212.9164362838583315, 96.69886208192143329 ) ) ;
#24065 = CIRCLE ( 'NONE', #9377, 70.00000000000000000 ) ;
#24066 = CARTESIAN_POINT ( 'NONE',  ( 12.00000000000000711, 207.0476921513415220, 36.99886208192143044 ) ) ;
#24067 = PLANE ( 'NONE',  #12693 ) ;
#24068 = CARTESIAN_POINT ( 'NONE',  ( 3.044812012440130555, 197.4746971517856764, 50.60113791807857808 ) ) ;
#24069 = ORIENTED_EDGE ( 'NONE', *, *, #22273, .F. ) ;
#24070 = AXIS2_PLACEMENT_3D ( 'NONE', #8691, #19083, #29472 ) ;
#24071 = CARTESIAN_POINT ( 'NONE',  ( 2.426778023690075337, 214.6231898156240447, 12.39886208192143613 ) ) ;
#24072 = ADVANCED_FACE ( 'NONE', ( #13385 ), #14540, .T. ) ;
#24073 = CARTESIAN_POINT ( 'NONE',  ( 79.18867513459481700, 169.2658477444273331, -4.635254915624224203 ) ) ;
#24074 = ORIENTED_EDGE ( 'NONE', *, *, #16386, .F. ) ;
#24075 = CARTESIAN_POINT ( 'NONE',  ( -0.05014649552828365914, 215.4116977939061144, 90.24886208192144466 ) ) ;
#24076 = CARTESIAN_POINT ( 'NONE',  ( 6.500168698208129925, 211.6636982574063381, 31.70113791807857240 ) ) ;
#24077 = CARTESIAN_POINT ( 'NONE',  ( 56.51132485994280330, 163.8167787843871110, 12.13525491562421621 ) ) ;
#24078 = EDGE_LOOP ( 'NONE', ( #15320, #28152, #32923, #28104 ) ) ;
#24079 = LINE ( 'NONE', #6015, #23245 ) ;
#24080 = AXIS2_PLACEMENT_3D ( 'NONE', #10981, #26149, #2816 ) ;
#24081 = CARTESIAN_POINT ( 'NONE',  ( 36.77499999726881441, 140.1801316387863778, 4.815267126137185549 ) ) ;
#24082 = CARTESIAN_POINT ( 'NONE',  ( -3.499999999999997780, -2.020725942163714262, -0.3126073911696551910 ) ) ;
#24083 = CARTESIAN_POINT ( 'NONE',  ( -4.903702542908602524, 213.8346818373418898, 96.95113791807857240 ) ) ;
#24085 = AXIS2_PLACEMENT_3D ( 'NONE', #13017, #17783, #28527 ) ;
#24084 = DIRECTION ( 'NONE',  ( 1.000000000000000000, 0.000000000000000000, 0.000000000000000000 ) ) ;
#24086 = CARTESIAN_POINT ( 'NONE',  ( 52.29999999999999716, 146.4771138417591203, -11.73074641843674470 ) ) ;
#24087 = CARTESIAN_POINT ( 'NONE',  ( 8.015496119326595448, 204.4483345814782638, 70.14886208192142192 ) ) ;
#24088 = CARTESIAN_POINT ( 'NONE',  ( -3.983107665916332252, 5.570601890521282407, -6.171481112545251335 ) ) ;
#24089 = ADVANCED_FACE ( 'NONE', ( #15609 ), #13561, .T. ) ;
#24090 = VECTOR ( 'NONE', #9281, 999.9999999999998863 ) ;
#24091 = CARTESIAN_POINT ( 'NONE',  ( 59.02499999726880731, 149.9369285172503510, -15.58253175000000823 ) ) ;
#24092 = CARTESIAN_POINT ( 'NONE',  ( 6.139770520408367460, 198.4640165459539389, 14.45113791807856529 ) ) ;
#24093 = CARTESIAN_POINT ( 'NONE',  ( 37.11132485994280472, 140.7341522555726669, 4.635254915624211769 ) ) ;
#24094 = CARTESIAN_POINT ( 'NONE',  ( 65.62499999726880162, 171.3844434931184253, -7.942151717890134290E-15 ) ) ;
#24095 = CARTESIAN_POINT ( 'NONE',  ( 77.57499999726881867, 164.1591823560292198, -12.60653300113719766 ) ) ;
#24096 = CARTESIAN_POINT ( 'NONE',  ( -7.456977232089304408, 196.8216656703010301, 75.05113791807858092 ) ) ;
#24097 = CARTESIAN_POINT ( 'NONE',  ( 6.220909254589536808, 215.4770327129947987, 100.5511379180785809 ) ) ;
#24098 = ADVANCED_FACE ( 'NONE', ( #23454 ), #4767, .T. ) ;
#24099 = DIRECTION ( 'NONE',  ( 1.000000000000000000, 0.000000000000000000, 0.000000000000000000 ) ) ;
#24100 = ORIENTED_EDGE ( 'NONE', *, *, #1853, .T. ) ;
#24101 = CARTESIAN_POINT ( 'NONE',  ( 11.98450388067341876, 210.9467285061363953, 102.8488620819214390 ) ) ;
#24102 = CARTESIAN_POINT ( 'NONE',  ( 3.753561863808876797, 195.6020594897209719, 64.59886208192142476 ) ) ;
#24103 = AXIS2_PLACEMENT_3D ( 'NONE', #26410, #11240, #31849 ) ;
#24104 = CARTESIAN_POINT ( 'NONE',  ( -3.044812012439970683, 197.4746971517856196, 64.89886208192145034 ) ) ;
#24105 = CARTESIAN_POINT ( 'NONE',  ( 7.456977232089471386, 196.8216656703012006, 7.448862081921435951 ) ) ;
#24106 = CARTESIAN_POINT ( 'NONE',  ( -58.50000000000002132, 209.9999999999999716, 0.000000000000000000 ) ) ;
#24107 = CARTESIAN_POINT ( 'NONE',  ( -0.05014649552810635652, 196.4853777576173002, 20.75113791807855890 ) ) ;
#24108 = CARTESIAN_POINT ( 'NONE',  ( 3.044812012439969795, 216.5253028482143520, 81.39886208192145034 ) ) ;
#24109 = ORIENTED_EDGE ( 'NONE', *, *, #27506, .F. ) ;
#24110 = ADVANCED_FACE ( 'NONE', ( #26014 ), #121, .T. ) ;
#24111 = CARTESIAN_POINT ( 'NONE',  ( -9.949154985843399857, 217.7087784572769067, 102.9933096652613074 ) ) ;
#24112 = AXIS2_PLACEMENT_3D ( 'NONE', #13489, #7896, #10294 ) ;
#24113 = VERTEX_POINT ( 'NONE', #23950 ) ;
#24114 = CARTESIAN_POINT ( 'NONE',  ( -2.352990130084580066E-16, 8.660254037844390851, -7.564335161054497547 ) ) ;
#24115 = CARTESIAN_POINT ( 'NONE',  ( 8.000000000000008882, 207.0476921513415220, 60.99886208192144466 ) ) ;
#24116 = ORIENTED_EDGE ( 'NONE', *, *, #7623, .T. ) ;
#24117 = AXIS2_PLACEMENT_3D ( 'NONE', #32243, #459, #28902 ) ;
#24118 = CARTESIAN_POINT ( 'NONE',  ( 75.82499999726881867, 168.2552932293087906, 9.630534252274372875 ) ) ;
#24119 = VERTEX_POINT ( 'NONE', #5395 ) ;
#24120 = FACE_OUTER_BOUND ( 'NONE', #23117, .T. ) ;
#24121 = CARTESIAN_POINT ( 'NONE',  ( 70.52499999726880731, 140.1801316387863778, 4.815267126137185549 ) ) ;
#24122 = EDGE_CURVE ( 'NONE', #22913, #23167, #17809, .T. ) ;
#24123 = CARTESIAN_POINT ( 'NONE',  ( 8.015496119326531499, 209.5516654185219636, 73.85113791807857808 ) ) ;
#24124 = SURFACE_STYLE_USAGE ( .BOTH. , #18685 ) ;
#24125 = CARTESIAN_POINT ( 'NONE',  ( -9.017078565483988228, 206.7748875732014255, 103.7159841306440313 ) ) ;
#24126 = CONICAL_SURFACE ( 'NONE', #17053, 3.499999999999999556, 1.047197551196589638 ) ;
#24127 = CARTESIAN_POINT ( 'NONE',  ( 33.50000000000000000, 155.0000000000000000, 14.49999999999999467 ) ) ;
#24128 =( GEOMETRIC_REPRESENTATION_CONTEXT ( 3 ) GLOBAL_UNCERTAINTY_ASSIGNED_CONTEXT ( ( #32575 ) ) GLOBAL_UNIT_ASSIGNED_CONTEXT ( ( #1970, #25476, #33314 ) ) REPRESENTATION_CONTEXT ( 'NONE', 'WORKASPACE' ) );
#24129 = CARTESIAN_POINT ( 'NONE',  ( -8.015496119326597224, 209.5516654185217362, 44.64886208192143613 ) ) ;
#24130 = EDGE_CURVE ( 'NONE', #23693, #20612, #31620, .T. ) ;
#24131 = CARTESIAN_POINT ( 'NONE',  ( -3.044812012440131443, 216.5253028482142952, 76.10113791807856387 ) ) ;
#24132 = CARTESIAN_POINT ( 'NONE',  ( 9.984503880673470277, 203.7031108863295401, 65.15113791807856103 ) ) ;
#24133 = CARTESIAN_POINT ( 'NONE',  ( -67.50000000000000000, 122.1366465496900418, -17.00000000000001421 ) ) ;
#24134 = CARTESIAN_POINT ( 'NONE',  ( 7.984503880673485376, 204.3529502787953902, 23.15113791807856458 ) ) ;
#24135 = CARTESIAN_POINT ( 'NONE',  ( 124.3127766070272457, -5.249999999999974243, 35.00001199999999812 ) ) ;
#24136 = CARTESIAN_POINT ( 'NONE',  ( 10.00000000000000888, 207.8771832641648984, -0.04188241574673567946 ) ) ;
#24137 = CARTESIAN_POINT ( 'NONE',  ( 44.62499999726880873, 138.6155565068815747, -3.929120461958505118E-15 ) ) ;
#24138 = CARTESIAN_POINT ( 'NONE',  ( -12.00000000000000711, 207.0476921513413515, 51.50113791807856956 ) ) ;
#24139 = CARTESIAN_POINT ( 'NONE',  ( 7.894787914004607998, 1.243647571710251278E-13, -7.591390474663425536 ) ) ;
#24140 = AXIS2_PLACEMENT_3D ( 'NONE', #24539, #1193, #31864 ) ;
#24141 = CARTESIAN_POINT ( 'NONE',  ( 8.062137200540920645, 201.0835637161417822, 95.30113791807858092 ) ) ;
#24142 = CARTESIAN_POINT ( 'NONE',  ( -10.00000000000000711, 207.0476921513413515, 66.50113791807856956 ) ) ;
#24143 = CARTESIAN_POINT ( 'NONE',  ( 0.05014649552828288198, 194.3824533091408000, 28.74886208192144110 ) ) ;
#24144 = CARTESIAN_POINT ( 'NONE',  ( 8.062137200540822946, 212.9164362838583315, 33.69886208192143329 ) ) ;
#24145 = CARTESIAN_POINT ( 'NONE',  ( 86.19999999453763451, 163.5228861582408797, -11.73074641843674470 ) ) ;
#24146 = CARTESIAN_POINT ( 'NONE',  ( 12.00000000000000711, 206.9523078486586485, 80.00113791807856956 ) ) ;
#24147 = CARTESIAN_POINT ( 'NONE',  ( -6.444103211791042618, 211.7408657792732356, 96.80113791807858092 ) ) ;
#24148 = CARTESIAN_POINT ( 'NONE',  ( -3.044812012439970683, 197.4746971517856196, 52.89886208192143613 ) ) ;
#24149 = CARTESIAN_POINT ( 'NONE',  ( 48.88867513459482694, 159.8737954434937478, -14.99999999999993072 ) ) ;
#24150 = ORIENTED_EDGE ( 'NONE', *, *, #29938, .F. ) ;
#24151 = CARTESIAN_POINT ( 'NONE',  ( -0.05014649552828442242, 219.6175466908591716, 63.24886208192142334 ) ) ;
#24152 = VECTOR ( 'NONE', #31590, 1000.000000000000114 ) ;
#24153 = ORIENTED_EDGE ( 'NONE', *, *, #20574, .F. ) ;
#24154 = CARTESIAN_POINT ( 'NONE',  ( -2.517493886309087880, 214.5937144450984135, 33.09886208192143897 ) ) ;
#24155 = VERTEX_POINT ( 'NONE', #18674 ) ;
#24156 = ADVANCED_FACE ( 'NONE', ( #611 ), #6934, .F. ) ;
#24157 = EDGE_CURVE ( 'NONE', #28067, #210, #32447, .T. ) ;
#24158 = CARTESIAN_POINT ( 'NONE',  ( 77.07499999726881867, 141.7447067706911810, -9.630534252274387086 ) ) ;
#24159 = CARTESIAN_POINT ( 'NONE',  ( 72.99495483890930814, 155.0000000000000000, -15.50000000000001776 ) ) ;
#24160 = CARTESIAN_POINT ( 'NONE',  ( 98.19869130599479945, 155.0000000000000000, 32.10452846326769816 ) ) ;
#24161 = CARTESIAN_POINT ( 'NONE',  ( -6.444103211791042618, 211.7408657792732356, 54.80113791807857382 ) ) ;
#24162 = ADVANCED_FACE ( 'NONE', ( #3500 ), #9114, .F. ) ;
#24163 = CIRCLE ( 'NONE', #6757, 8.542937654374687995 ) ;
#24164 = EDGE_CURVE ( 'NONE', #8613, #20097, #7485, .T. ) ;
#24165 = CARTESIAN_POINT ( 'NONE',  ( 3.499999999999993339, -2.020725942163723143, -2.587392608830344720 ) ) ;
#24166 = CARTESIAN_POINT ( 'NONE',  ( 3.044812012439969795, 216.5253028482143520, 36.39886208192142902 ) ) ;
#24167 = CARTESIAN_POINT ( 'NONE',  ( 68.57499999726881867, 145.8408176439707802, 12.60653300113718345 ) ) ;
#24168 = ORIENTED_EDGE ( 'NONE', *, *, #1139, .F. ) ;
#24169 = CARTESIAN_POINT ( 'NONE',  ( 62.48867513459482836, 142.2402378747194405, -9.270509831248439525 ) ) ;
#24170 = CARTESIAN_POINT ( 'NONE',  ( 43.08867513459483689, 167.7597621252805880, -9.270509831248443078 ) ) ;
#24171 = CARTESIAN_POINT ( 'NONE',  ( 4.984841277089891776, 200.2242689037093726, 16.44886208192143684 ) ) ;
#24172 = EDGE_CURVE ( 'NONE', #13676, #10180, #6393, .T. ) ;
#24173 = CARTESIAN_POINT ( 'NONE',  ( -10.01549611932653860, 203.7984951890123284, 51.35113791807858519 ) ) ;
#24174 = FACE_OUTER_BOUND ( 'NONE', #15778, .T. ) ;
#24175 = CARTESIAN_POINT ( 'NONE',  ( -3.044812012440131443, 216.5253028482142952, 37.10113791807857098 ) ) ;
#24176 = CARTESIAN_POINT ( 'NONE',  ( 84.07499999726877604, 168.2552932293087906, 9.630534252274372875 ) ) ;
#24177 = APPLICATION_PROTOCOL_DEFINITION ( 'draft international standard', 'automotive_design', 1998, #13556 ) ;
#24178 = PRESENTATION_LAYER_ASSIGNMENT (  '', '', ( #15484 ) ) ;
#24179 = CARTESIAN_POINT ( 'NONE',  ( 0.05014649552828262524, 198.5883022060938572, 103.7488620819214304 ) ) ;
#24180 = CARTESIAN_POINT ( 'NONE',  ( 39.22499999726881015, 160.0630714827496206, -15.58253175000000823 ) ) ;
#24181 = CARTESIAN_POINT ( 'NONE',  ( -52.50000000000002132, 155.0000000000000000, 6.938893903907228378E-15 ) ) ;
#24182 = CARTESIAN_POINT ( 'NONE',  ( -12.01549611932652972, 203.1486557965464499, 15.35113791807856387 ) ) ;
#24183 = CARTESIAN_POINT ( 'NONE',  ( 117.5000000000000142, 155.0000000000000000, -98.00000000000002842 ) ) ;
#24184 = CARTESIAN_POINT ( 'NONE',  ( 64.47499999726881015, 149.9369285172503510, 15.58253174999999580 ) ) ;
#24185 = CARTESIAN_POINT ( 'NONE',  ( 10.01549611932653860, 210.2015048109876716, 61.85113791807857098 ) ) ;
#24186 = CARTESIAN_POINT ( 'NONE',  ( -3.135527875058821579, 197.5041725223112223, 35.90113791807856813 ) ) ;
#24187 = LINE ( 'NONE', #13958, #14839 ) ;
#24188 = CARTESIAN_POINT ( 'NONE',  ( -7.940546747334008337, 27.16978800334332078, -17.55088044235632694 ) ) ;
#24189 = CARTESIAN_POINT ( 'NONE',  ( -3.753561863808691168, 195.6020594897209435, 101.9011379180785895 ) ) ;
#24190 = CARTESIAN_POINT ( 'NONE',  ( 9.984503880673420539, 210.2968891136705736, 9.848862081921435419 ) ) ;
#24191 = CARTESIAN_POINT ( 'NONE',  ( 61.89999999453763024, 150.2886644046228639, -14.50000000000000888 ) ) ;
#24192 = ORIENTED_EDGE ( 'NONE', *, *, #21594, .T. ) ;
#24193 = CARTESIAN_POINT ( 'NONE',  ( 7.456977232089302632, 217.1783343296989131, 52.55113791807856671 ) ) ;
#24194 = LINE ( 'NONE', #31534, #20337 ) ;
#24195 = CARTESIAN_POINT ( 'NONE',  ( 8.118202686958138514, 201.1607312380088501, 19.29886208192143471 ) ) ;
#24196 = CARTESIAN_POINT ( 'NONE',  ( 58.71132485994280614, 155.0000000000000000, 15.00000000000001243 ) ) ;
#24197 = ORIENTED_EDGE ( 'NONE', *, *, #20539, .T. ) ;
#24198 = CARTESIAN_POINT ( 'NONE',  ( -10.00000000000000711, 207.0476921513413515, 84.50113791807856956 ) ) ;
#24199 = ORIENTED_EDGE ( 'NONE', *, *, #31340, .T. ) ;
#24200 = APPLICATION_CONTEXT ( 'automotive_design' ) ;
#24201 = DIRECTION ( 'NONE',  ( -0.000000000000000000, -0.000000000000000000, 1.000000000000000000 ) ) ;
#24202 = CARTESIAN_POINT ( 'NONE',  ( 57.71132485994280614, 155.0000000000000000, -15.00000000000002487 ) ) ;
#24203 = ORIENTED_EDGE ( 'NONE', *, *, #23699, .T. ) ;
#24204 = CARTESIAN_POINT ( 'NONE',  ( 4.903702542908601636, 200.1653181626581102, 26.45113791807857240 ) ) ;
#24205 = CARTESIAN_POINT ( 'NONE',  ( -60.98407617557292326, 194.9989950908677088, 0.3262505061364526227 ) ) ;
#24206 = CARTESIAN_POINT ( 'NONE',  ( -9.984503880673420539, 203.7031108863293980, 5.348862081921433642 ) ) ;
#24207 = CARTESIAN_POINT ( 'NONE',  ( 49.27499999726880020, 149.9369285172503510, -15.58253175000000823 ) ) ;
#24208 = ORIENTED_EDGE ( 'NONE', *, *, #27635, .F. ) ;
#24209 = CARTESIAN_POINT ( 'NONE',  ( 58.62499999726880162, 138.6155565068815463, -3.929120461958505118E-15 ) ) ;
#24210 = CARTESIAN_POINT ( 'NONE',  ( 92.60208470531341618, 155.0000000000000000, 0.000000000000000000 ) ) ;
#24211 = CARTESIAN_POINT ( 'NONE',  ( -1.750000000000016209, -3.031088913245524985, -2.899999999999999911 ) ) ;
#24212 = CARTESIAN_POINT ( 'NONE',  ( -52.50000000000002132, 120.3589838486224579, -20.00000000000000000 ) ) ;
#24213 = CARTESIAN_POINT ( 'NONE',  ( -3.044812012439970683, 197.4746971517856196, 85.89886208192143613 ) ) ;
#24214 = CARTESIAN_POINT ( 'NONE',  ( 58.47499999726880304, 149.9369285172503510, 15.58253174999999580 ) ) ;
#24215 = CARTESIAN_POINT ( 'NONE',  ( 9.984503880673470277, 203.7031108863295401, 26.15113791807856813 ) ) ;
#24216 = CARTESIAN_POINT ( 'NONE',  ( 7.500000000000000000, -4.330127018922199866, -7.422398894150035176 ) ) ;
#24217 = CARTESIAN_POINT ( 'NONE',  ( -3.662846001189865142, 195.5725841191952838, 76.89886208192143613 ) ) ;
#24218 = CARTESIAN_POINT ( 'NONE',  ( 74.00000000000000000, 139.7537977485451393, -4.138211985947621020E-15 ) ) ;
#24219 = CARTESIAN_POINT ( 'NONE',  ( 64.78867513459482552, 155.0000000000000000, -15.00000000000002487 ) ) ;
#24220 = DIRECTION ( 'NONE',  ( 1.000000000000000000, -0.000000000000000000, -0.000000000000000000 ) ) ;
#24221 = CARTESIAN_POINT ( 'NONE',  ( -8.118202686958039038, 201.1607312380087080, 90.20113791807857240 ) ) ;
#24222 = DIRECTION ( 'NONE',  ( -1.000000000000000000, 0.000000000000000000, -0.000000000000000000 ) ) ;
#24223 = CARTESIAN_POINT ( 'NONE',  ( 40.27499999726881441, 160.0630714827496206, 15.58253174999999402 ) ) ;
#24224 = CARTESIAN_POINT ( 'NONE',  ( -10.00000000000000711, 207.0476921513413515, 36.50113791807857666 ) ) ;
#24225 = CARTESIAN_POINT ( 'NONE',  ( 74.62499999726883004, 138.6155565068815463, -3.929120461958505118E-15 ) ) ;
#24226 = ORIENTED_EDGE ( 'NONE', *, *, #14533, .T. ) ;
#24227 = CARTESIAN_POINT ( 'NONE',  ( 32.50000000000000000, 155.0000000000000000, -15.00000000000002487 ) ) ;
#24228 = CARTESIAN_POINT ( 'NONE',  ( 39.89999999453763735, 150.2886644046228639, -14.50000000000000888 ) ) ;
#24229 = CARTESIAN_POINT ( 'NONE',  ( -9.736236675707914401, 199.9851607334237542, 24.20113791807856529 ) ) ;
#24230 = DIRECTION ( 'NONE',  ( 1.000000000000000000, 0.000000000000000000, 0.000000000000000000 ) ) ;
#24231 = FACE_OUTER_BOUND ( 'NONE', #30790, .T. ) ;
#24232 = ORIENTED_EDGE ( 'NONE', *, *, #20838, .T. ) ;
#24233 = CARTESIAN_POINT ( 'NONE',  ( 0.05014649552828288198, 194.3824533091408000, 37.74886208192143755 ) ) ;
#24234 = DIRECTION ( 'NONE',  ( 0.000000000000000000, 0.000000000000000000, 1.000000000000000000 ) ) ;
#24235 = CARTESIAN_POINT ( 'NONE',  ( 3.135527875058820690, 216.4958274776887492, 52.40113791807857524 ) ) ;
#24236 = ORIENTED_EDGE ( 'NONE', *, *, #16236, .F. ) ;
#24237 = CARTESIAN_POINT ( 'NONE',  ( -6.444103211790928043, 202.2591342207265939, 17.19886208192143684 ) ) ;
#24238 = CARTESIAN_POINT ( 'NONE',  ( 78.78867513459481131, 155.0000000000000000, -15.00000000000002487 ) ) ;
#24239 = ORIENTED_EDGE ( 'NONE', *, *, #5202, .T. ) ;
#24240 = CARTESIAN_POINT ( 'NONE',  ( -8.015496119326597224, 209.5516654185217362, 101.6488620819214361 ) ) ;
#24241 = CARTESIAN_POINT ( 'NONE',  ( -4.984841277089726574, 200.2242689037092305, 42.05113791807857382 ) ) ;
#24242 = FACE_OUTER_BOUND ( 'NONE', #1566, .T. ) ;
#24243 = ORIENTED_EDGE ( 'NONE', *, *, #7501, .T. ) ;
#24244 = CARTESIAN_POINT ( 'NONE',  ( 35.72499999726881015, 169.8198683612136222, 4.815267126137181997 ) ) ;
#24245 = CARTESIAN_POINT ( 'NONE',  ( 6.220909254589681581, 198.5229672870052582, 58.44886208192144039 ) ) ;
#24246 = CARTESIAN_POINT ( 'NONE',  ( 37.07499999726881157, 141.7447067706911810, -9.630534252274385310 ) ) ;
#24247 = DIRECTION ( 'NONE',  ( -1.000000000000000000, 0.000000000000000000, 0.000000000000000000 ) ) ;
#24248 = CARTESIAN_POINT ( 'NONE',  ( -2.517493886308901807, 199.4062855549015012, 98.90113791807858945 ) ) ;
#24249 = EDGE_CURVE ( 'NONE', #18434, #73, #2081, .T. ) ;
#24250 = CARTESIAN_POINT ( 'NONE',  ( 54.80000000000000426, 167.3344367211045096, -8.961492836873482304 ) ) ;
#24251 = CARTESIAN_POINT ( 'NONE',  ( 6.444103211790928043, 211.7408657792734061, 72.69886208192143329 ) ) ;
#24252 = CARTESIAN_POINT ( 'NONE',  ( 33.71132485994280614, 155.0000000000000000, -15.00000000000002487 ) ) ;
#24253 = CARTESIAN_POINT ( 'NONE',  ( 55.62499999726881583, 171.3844434931184253, -7.942151717890132712E-15 ) ) ;
#24254 = CARTESIAN_POINT ( 'NONE',  ( 6.220909254589536808, 215.4770327129947987, 13.55113791807856671 ) ) ;
#24255 = CARTESIAN_POINT ( 'NONE',  ( -6.500000000000000000, -4.014037567183532218, -6.470355840301004413 ) ) ;
#24256 = CARTESIAN_POINT ( 'NONE',  ( 64.72499999726881015, 140.1801316387863778, -4.815267126137194431 ) ) ;
#24257 = CARTESIAN_POINT ( 'NONE',  ( 73.37499999726881583, 155.0000000000000000, -15.58253175000000823 ) ) ;
#24258 = CARTESIAN_POINT ( 'NONE',  ( 3.753561863808689836, 218.3979405102790565, 73.40113791807856103 ) ) ;
#24259 = CARTESIAN_POINT ( 'NONE',  ( -0.05014649552810635652, 196.4853777576173002, 95.75113791807856956 ) ) ;
#24260 = DIRECTION ( 'NONE',  ( 1.000000000000000000, 0.000000000000000000, 0.000000000000000000 ) ) ;
#24261 = VERTEX_POINT ( 'NONE', #19676 ) ;
#24262 = CARTESIAN_POINT ( 'NONE',  ( -10.00000000000000711, 206.9523078486584495, 2.498862081921433997 ) ) ;
#24263 = CARTESIAN_POINT ( 'NONE',  ( 12.01549611932659367, 203.1486557965466773, 61.14886208192143613 ) ) ;
#24264 = CARTESIAN_POINT ( 'NONE',  ( -8.118202686958138514, 212.8392687619910930, 62.79886208192144181 ) ) ;
#24265 = CARTESIAN_POINT ( 'NONE',  ( -12.00000000000000711, 206.9523078486584780, 2.498862081921434442 ) ) ;
#24266 = CARTESIAN_POINT ( 'NONE',  ( -67.50001199999998391, 166.2340547598724356, -12.80757580047018251 ) ) ;
#24267 = CARTESIAN_POINT ( 'NONE',  ( -3.135527875058821579, 197.5041725223112223, 26.90113791807856813 ) ) ;
#24268 = CARTESIAN_POINT ( 'NONE',  ( -9.984503880673420539, 203.7031108863293980, 89.34886208192143897 ) ) ;
#24269 = VERTEX_POINT ( 'NONE', #24455 ) ;
#24270 = CARTESIAN_POINT ( 'NONE',  ( 5.000000000000000000, 4.969004387540385421E-16, -4.057500000000000107 ) ) ;
#24271 = VERTEX_POINT ( 'NONE', #1287 ) ;
#24272 = DIRECTION ( 'NONE',  ( 0.000000000000000000, 0.000000000000000000, 1.000000000000000000 ) ) ;
#24273 = CARTESIAN_POINT ( 'NONE',  ( 7.984503880673422316, 209.6470497212048372, 69.84886208192143897 ) ) ;
#24274 = ORIENTED_EDGE ( 'NONE', *, *, #25576, .F. ) ;
#24275 = CARTESIAN_POINT ( 'NONE',  ( 79.62499999726881583, 171.3844434931184253, -7.942151717890134290E-15 ) ) ;
#24276 = ORIENTED_EDGE ( 'NONE', *, *, #20611, .F. ) ;
#24277 = DIRECTION ( 'NONE',  ( -1.000000000000000000, 0.000000000000000000, 0.000000000000000000 ) ) ;
#24278 = B_SPLINE_CURVE_WITH_KNOTS ( 'NONE', 3,
 ( #6358, #32754, #1750, #19983 ),
 .UNSPECIFIED., .F., .F.,
 ( 4, 4 ),
 ( 2.380739282168500117E-07, 0.002044882221487550125 ),
 .UNSPECIFIED. ) ;
#24279 = CARTESIAN_POINT ( 'NONE',  ( 68.72499999726881015, 140.1801316387863778, -4.815267126137194431 ) ) ;
#24280 = CARTESIAN_POINT ( 'NONE',  ( -8.015496119326531499, 204.4483345814780364, 66.35113791807857808 ) ) ;
#24281 = CARTESIAN_POINT ( 'NONE',  ( 115.4999999999999858, 155.0000000000000000, -50.00000000000000711 ) ) ;
#24282 = ADVANCED_FACE ( 'NONE', ( #13889 ), #16945, .T. ) ;
#24283 = VECTOR ( 'NONE', #18592, 1000.000000000000000 ) ;
#24284 = CARTESIAN_POINT ( 'NONE',  ( -9.452103778985696536, 206.1202243157721057, 104.3225283253248392 ) ) ;
#24285 = B_SPLINE_CURVE_WITH_KNOTS ( 'NONE', 3,
 ( #1592, #25433, #6872, #22547, #4481, #7213, #25267, #17600, #27991, #4657 ),
 .UNSPECIFIED., .F., .F.,
 ( 4, 2, 2, 2, 4 ),
 ( 0.009353627468483380336, 0.01031000219096067476, 0.01126637691343796918, 0.01222275163591526534, 0.01317912635839255976 ),
 .UNSPECIFIED. ) ;
#24286 = SURFACE_STYLE_USAGE ( .BOTH. , #19020 ) ;
#24287 = CARTESIAN_POINT ( 'NONE',  ( 34.89999999999999858, 168.7903194862797420, -4.480746418436745593 ) ) ;
#24288 = CARTESIAN_POINT ( 'NONE',  ( -2.426778023690076225, 199.3768101843759553, 43.89886208192144323 ) ) ;
#24289 = CARTESIAN_POINT ( 'NONE',  ( -3.135527875058821579, 197.5041725223112223, 83.90113791807857524 ) ) ;
#24290 = CARTESIAN_POINT ( 'NONE',  ( 8.062137200540920645, 201.0835637161417822, 68.30113791807856671 ) ) ;
#24291 = VECTOR ( 'NONE', #8825, 1000.000000000000000 ) ;
#24292 = EDGE_CURVE ( 'NONE', #20665, #25118, #26503, .T. ) ;
#24293 = CARTESIAN_POINT ( 'NONE',  ( 92.60756280994512224, 155.0000000000000000, 0.000000000000000000 ) ) ;
#24294 = CARTESIAN_POINT ( 'NONE',  ( 6.444103211791042618, 202.2591342207267644, 23.30113791807857027 ) ) ;
#24295 = CARTESIAN_POINT ( 'NONE',  ( 0.000000000000000000, 0.000000000000000000, 0.000000000000000000 ) ) ;
#24296 = CARTESIAN_POINT ( 'NONE',  ( -3.499999999999996891, -1.692071238847157710, -0.2177329504545129080 ) ) ;
#24297 = CARTESIAN_POINT ( 'NONE',  ( 44.02499999726881441, 160.0630714827496206, 15.58253174999999224 ) ) ;
#24298 = CARTESIAN_POINT ( 'NONE',  ( -9.736236675707914401, 199.9851607334237542, 45.20113791807857240 ) ) ;
#24299 = CARTESIAN_POINT ( 'NONE',  ( 7.500000000000000000, 4.732328341851997244, -7.493855119309152713 ) ) ;
#24300 = CARTESIAN_POINT ( 'NONE',  ( -0.05014649552810635652, 196.4853777576173002, 95.75113791807856956 ) ) ;
#24301 = CARTESIAN_POINT ( 'NONE',  ( 3.044812012440130555, 197.4746971517856764, 68.60113791807857808 ) ) ;
#24302 = CARTESIAN_POINT ( 'NONE',  ( 0.05014649552828288198, 194.3824533091408000, 31.74886208192143755 ) ) ;
#24303 = CARTESIAN_POINT ( 'NONE',  ( 9.984503880673420539, 210.2968891136705736, 33.84886208192143187 ) ) ;
#24304 = CARTESIAN_POINT ( 'NONE',  ( 84.29999999453761461, 167.3344367211045096, -8.961492836873482304 ) ) ;
#24305 = CARTESIAN_POINT ( 'NONE',  ( -9.736236675707914401, 199.9851607334237542, 81.20113791807858661 ) ) ;
#24306 = CIRCLE ( 'NONE', #8563, 32.10452846326764131 ) ;
#24307 = CARTESIAN_POINT ( 'NONE',  ( -4.984841277089726574, 200.2242689037092305, 99.05113791807858092 ) ) ;
#24308 = EDGE_CURVE ( 'NONE', #27342, #9113, #22064, .T. ) ;
#24309 = CARTESIAN_POINT ( 'NONE',  ( 0.05014649552828275708, 196.4853777576173002, 58.74886208192141623 ) ) ;
#24310 =( LENGTH_UNIT ( ) NAMED_UNIT ( * ) SI_UNIT ( .MILLI., .METRE. ) );
#24311 = EDGE_LOOP ( 'NONE', ( #4601, #18047, #6472, #23230 ) ) ;
#24312 = CARTESIAN_POINT ( 'NONE',  ( 9.680171189290716072, 214.0920067884432854, 60.69886208192144039 ) ) ;
#24313 = COLOUR_RGB ( '', 0.66274510, 0.83137255, 0.94901961) ;
#24314 = ORIENTED_EDGE ( 'NONE', *, *, #30216, .F. ) ;
#24315 = CARTESIAN_POINT ( 'NONE',  ( 70.17499999726881299, 164.1591823560292198, 12.60653300113718167 ) ) ;
#24316 = CARTESIAN_POINT ( 'NONE',  ( 0.05014649552828262524, 198.5883022060938572, 31.74886208192143755 ) ) ;
#24317 = EDGE_CURVE ( 'NONE', #27639, #30739, #942, .T. ) ;
#24318 = EDGE_LOOP ( 'NONE', ( #13137, #33640, #32364, #404, #8856, #15057 ) ) ;
#24319 = VECTOR ( 'NONE', #4859, 1000.000000000000000 ) ;
#24320 = CARTESIAN_POINT ( 'NONE',  ( 79.77499999726880731, 169.8198683612136222, -4.815267126137197984 ) ) ;
#24321 = CARTESIAN_POINT ( 'NONE',  ( 76.71132485994280614, 155.0000000000000000, 15.00000000000001243 ) ) ;
#24322 = DIRECTION ( 'NONE',  ( -0.000000000000000000, -0.000000000000000000, -1.000000000000000000 ) ) ;
#24323 = CARTESIAN_POINT ( 'NONE',  ( -0.05014649552807731031, 198.5883022060938572, 50.75113791807857666 ) ) ;
#24324 = SURFACE_STYLE_FILL_AREA ( #28945 ) ;
#24325 = CARTESIAN_POINT ( 'NONE',  ( -10.00000000000000711, 206.9523078486584495, 29.49886208192143400 ) ) ;
#24326 = CARTESIAN_POINT ( 'NONE',  ( 67.37499999726881583, 155.0000000000000000, -15.58253175000000823 ) ) ;
#24327 = ORIENTED_EDGE ( 'NONE', *, *, #20169, .T. ) ;
#24328 = CYLINDRICAL_SURFACE ( 'NONE', #28171, 50.00000000000000000 ) ;
#24329 = SHAPE_REPRESENTATION_RELATIONSHIP ( 'NONE' , 'NONE' ,  #21975, #21009 ) ;
#24330 = LINE ( 'NONE', #21157, #14500 ) ;
#24331 = DIRECTION ( 'NONE',  ( -1.000000000000000000, 0.000000000000000000, 0.000000000000000000 ) ) ;
#24332 = CARTESIAN_POINT ( 'NONE',  ( -2.517493886309087880, 214.5937144450984135, 12.09886208192143364 ) ) ;
#24333 = CIRCLE ( 'NONE', #22177, 37.00000000000000711 ) ;
#24334 = CARTESIAN_POINT ( 'NONE',  ( 8.062137200540920645, 201.0835637161417822, 50.30113791807857382 ) ) ;
#24335 = CARTESIAN_POINT ( 'NONE',  ( 10.01549611932653860, 210.2015048109876716, 40.85113791807857098 ) ) ;
#24336 = CARTESIAN_POINT ( 'NONE',  ( 82.77499999726880731, 140.1801316387863778, 4.815267126137185549 ) ) ;
#24337 = AXIS2_PLACEMENT_3D ( 'NONE', #1117, #8950, #1618 ) ;
#24338 = APPLICATION_PROTOCOL_DEFINITION ( 'draft international standard', 'automotive_design', 1998, #14200 ) ;
#24339 = VECTOR ( 'NONE', #6714, 1000.000000000000000 ) ;
#24340 = CARTESIAN_POINT ( 'NONE',  ( 4.984841277089891776, 200.2242689037093726, 103.4488620819214475 ) ) ;
#24341 = CARTESIAN_POINT ( 'NONE',  ( 40.12499999726880873, 155.0000000000000000, 15.58253174999999402 ) ) ;
#24342 = CARTESIAN_POINT ( 'NONE',  ( 36.48867513459482836, 142.2402378747194405, -9.270509831248439525 ) ) ;
#24343 = DIRECTION ( 'NONE',  ( 0.000000000000000000, 0.000000000000000000, 1.000000000000000000 ) ) ;
#24344 = CARTESIAN_POINT ( 'NONE',  ( 12.01549611932652972, 210.8513442034534933, 19.85113791807856387 ) ) ;
#24345 = CARTESIAN_POINT ( 'NONE',  ( 0.000000000000000000, 0.000000000000000000, -1.400415076419418092 ) ) ;
#24346 = CARTESIAN_POINT ( 'NONE',  ( 65.07499999726881867, 141.7447067706911810, -9.630534252274385310 ) ) ;
#24347 = EDGE_CURVE ( 'NONE', #28318, #4979, #27340, .T. ) ;
#24348 = CARTESIAN_POINT ( 'NONE',  ( 10.01549611932653860, 210.2015048109876716, 64.85113791807857808 ) ) ;
#24349 = EDGE_CURVE ( 'NONE', #31055, #18759, #13472, .T. ) ;
#24350 = CARTESIAN_POINT ( 'NONE',  ( -0.05014649552810635652, 196.4853777576173002, 41.75113791807856245 ) ) ;
#24351 = CIRCLE ( 'NONE', #3128, 13.49999999999996980 ) ;
#24352 = DIRECTION ( 'NONE',  ( 0.1045284632676472814, 0.000000000000000000, -0.9945218953682740670 ) ) ;
#24353 = CARTESIAN_POINT ( 'NONE',  ( 85.78867513459481131, 155.0000000000000000, 15.00000000000001243 ) ) ;
#24354 = CARTESIAN_POINT ( 'NONE',  ( -9.736236675708031640, 214.0148392665760753, 5.798862081921434708 ) ) ;
#24355 = CARTESIAN_POINT ( 'NONE',  ( -0.05014649552828402690, 217.5146222423826714, 12.24886208192143577 ) ) ;
#24356 = CARTESIAN_POINT ( 'NONE',  ( 66.69999999453763451, 167.3344367211045096, 8.961492836873468093 ) ) ;
#24357 = ORIENTED_EDGE ( 'NONE', *, *, #11401, .T. ) ;
#24358 = CARTESIAN_POINT ( 'NONE',  ( -7.456977232089304408, 196.8216656703010301, 45.05113791807857382 ) ) ;
#24359 = CARTESIAN_POINT ( 'NONE',  ( 0.05014649552807626948, 215.4116977939061144, 67.25113791807856956 ) ) ;
#24360 = ADVANCED_FACE ( 'NONE', ( #11343 ), #11844, .F. ) ;
#24361 = FACE_BOUND ( 'NONE', #12819, .T. ) ;
#24362 = CARTESIAN_POINT ( 'NONE',  ( -3.135527875058982783, 216.4958274776886924, 21.09886208192143897 ) ) ;
#24363 = CYLINDRICAL_SURFACE ( 'NONE', #8512, 15.00000000000001776 ) ;
#24364 = VERTEX_POINT ( 'NONE', #4168 ) ;
#24365 = CARTESIAN_POINT ( 'NONE',  ( 10.01549611932653860, 210.2015048109876716, 82.85113791807854966 ) ) ;
#24366 = AXIS2_PLACEMENT_3D ( 'NONE', #28544, #7756, #10324 ) ;
#24367 = ADVANCED_FACE ( 'NONE', ( #8778 ), #12008, .F. ) ;
#24368 = ORIENTED_EDGE ( 'NONE', *, *, #179, .T. ) ;
#24369 = AXIS2_PLACEMENT_3D ( 'NONE', #26835, #29567, #6220 ) ;
#24370 = DIRECTION ( 'NONE',  ( 1.000000000000000000, 0.000000000000000000, 0.000000000000000000 ) ) ;
#24371 = AXIS2_PLACEMENT_3D ( 'NONE', #8140, #21735, #18524 ) ;
#24372 = CARTESIAN_POINT ( 'NONE',  ( -6.878751942472531411, -3.924677726130930910, -6.573129608219091757 ) ) ;
#24373 = EDGE_LOOP ( 'NONE', ( #14261, #22143, #6998, #8429, #19958 ) ) ;
#24374 = CARTESIAN_POINT ( 'NONE',  ( 0.05014649552807626948, 215.4116977939061144, 22.25113791807856956 ) ) ;
#24375 = DIRECTION ( 'NONE',  ( 0.000000000000000000, 0.000000000000000000, 1.000000000000000000 ) ) ;
#24376 = CARTESIAN_POINT ( 'NONE',  ( -8.118202686958138514, 212.8392687619910930, 5.798862081921434708 ) ) ;
#24377 = CARTESIAN_POINT ( 'NONE',  ( 50.97499999726881725, 140.1801316387863778, -4.815267126137194431 ) ) ;
#24379 = ORIENTED_EDGE ( 'NONE', *, *, #9880, .F. ) ;
#24378 = TOROIDAL_SURFACE ( 'NONE', #6407, 4.999999999999990230, 2.500000000000000000 ) ;
#24380 = CARTESIAN_POINT ( 'NONE',  ( 57.42499999726880588, 168.2552932293087906, -9.630534252274385310 ) ) ;
#24381 = DIRECTION ( 'NONE',  ( 0.1045284632676470454, 1.217938055844715641E-16, 0.9945218953682739560 ) ) ;
#24382 = CARTESIAN_POINT ( 'NONE',  ( 58.78867513459481842, 155.0000000000000000, -15.00000000000002487 ) ) ;
#24383 = DIRECTION ( 'NONE',  ( 1.000000000000000000, 0.000000000000000000, 0.000000000000000000 ) ) ;
#24384 = CARTESIAN_POINT ( 'NONE',  ( -8.118202686958138514, 212.8392687619910930, 92.79886208192144181 ) ) ;
#24385 = CARTESIAN_POINT ( 'NONE',  ( 58.97499999726881015, 140.1801316387863778, -4.815267126137194431 ) ) ;
#24386 = CARTESIAN_POINT ( 'NONE',  ( -10.00000000000000711, 207.0476921513413515, 27.50113791807856600 ) ) ;
#24387 = CARTESIAN_POINT ( 'NONE',  ( 47.08867513459482979, 167.7597621252805880, -9.270509831248443078 ) ) ;
#24388 = CARTESIAN_POINT ( 'NONE',  ( -9.736236675708031640, 214.0148392665760753, 74.79886208192142760 ) ) ;
#24389 = ADVANCED_FACE ( 'NONE', ( #9456 ), #19171, .T. ) ;
#24390 = CARTESIAN_POINT ( 'NONE',  ( 72.29999999999999716, 146.4771138417591203, -11.73074641843674470 ) ) ;
#24391 = CARTESIAN_POINT ( 'NONE',  ( -7.500000000000000888, -4.330127018922198090, -7.564335161054497547 ) ) ;
#24392 = LINE ( 'NONE', #13493, #20219 ) ;
#24393 = CARTESIAN_POINT ( 'NONE',  ( 3.135527875058820690, 216.4958274776887492, 94.40113791807857524 ) ) ;
#24394 = AXIS2_PLACEMENT_3D ( 'NONE', #25311, #1975, #22762 ) ;
#24395 = LINE ( 'NONE', #1061, #16737 ) ;
#24396 = CARTESIAN_POINT ( 'NONE',  ( 47.17499999726881299, 145.8408176439707802, -12.60653300113719588 ) ) ;
#24397 = CARTESIAN_POINT ( 'NONE',  ( 10.00000000000000711, 206.9523078486586201, 41.00113791807856956 ) ) ;
#24398 = EDGE_CURVE ( 'NONE', #11008, #24997, #2083, .T. ) ;
#24399 = AXIS2_PLACEMENT_3D ( 'NONE', #28614, #9882, #25376 ) ;
#24400 = CARTESIAN_POINT ( 'NONE',  ( 79.22499999726879594, 160.0630714827496206, -15.58253175000000823 ) ) ;
#24401 = VERTEX_POINT ( 'NONE', #16608 ) ;
#24402 = LINE ( 'NONE', #29177, #28779 ) ;
#24403 = CARTESIAN_POINT ( 'NONE',  ( 46.59999999453762598, 168.7903194862797420, 4.480746418436729606 ) ) ;
#24404 = CARTESIAN_POINT ( 'NONE',  ( 11.98450388067348271, 203.0532714938637753, 17.15113791807856458 ) ) ;
#24405 = CARTESIAN_POINT ( 'NONE',  ( -3.499999999999999112, -1.355464348821716625, -2.761841578728549962 ) ) ;
#24406 = VECTOR ( 'NONE', #33160, 1000.000000000000227 ) ;
#24407 = CARTESIAN_POINT ( 'NONE',  ( -7.968863443239230016, -4.547634245050486079, -8.057411785091789014 ) ) ;
#24408 = ORIENTED_EDGE ( 'NONE', *, *, #9529, .F. ) ;
#24409 = CARTESIAN_POINT ( 'NONE',  ( -12.01549611932659722, 210.8513442034533227, 32.64886208192143613 ) ) ;
#24410 = CYLINDRICAL_SURFACE ( 'NONE', #12671, 2.149999999999979483 ) ;
#24411 = CARTESIAN_POINT ( 'NONE',  ( 9.984503880673470277, 203.7031108863295401, 53.15113791807857524 ) ) ;
#24412 = ORIENTED_EDGE ( 'NONE', *, *, #10985, .T. ) ;
#24413 = CARTESIAN_POINT ( 'NONE',  ( -4.984841277089891776, 213.7757310962905990, 8.948862081921433287 ) ) ;
#24414 = PRODUCT_DEFINITION_CONTEXT ( 'detailed design', #22452, 'design' ) ;
#24415 = CARTESIAN_POINT ( 'NONE',  ( -13.75000000000001243, -23.81569860407206107, -18.00000000000000000 ) ) ;
#24416 = ORIENTED_EDGE ( 'NONE', *, *, #5404, .F. ) ;
#24417 = CARTESIAN_POINT ( 'NONE',  ( -2.517493886309087880, 214.5937144450984135, 102.0988620819214532 ) ) ;
#24418 = CIRCLE ( 'NONE', #9732, 19.99999999999998934 ) ;
#24419 = CARTESIAN_POINT ( 'NONE',  ( 7.984503880673485376, 204.3529502787953902, 38.15113791807856813 ) ) ;
#24420 = DIRECTION ( 'NONE',  ( 0.000000000000000000, 0.000000000000000000, -1.000000000000000000 ) ) ;
#24421 = ORIENTED_EDGE ( 'NONE', *, *, #32608, .T. ) ;
#24422 = CARTESIAN_POINT ( 'NONE',  ( 40.62499999726880873, 138.6155565068815463, -3.929120461958505118E-15 ) ) ;
#24423 = AXIS2_PLACEMENT_3D ( 'NONE', #23257, #22921, #15252 ) ;
#24424 = CARTESIAN_POINT ( 'NONE',  ( -6.139770520408224463, 198.4640165459539389, 62.04886208192142050 ) ) ;
#24425 = CARTESIAN_POINT ( 'NONE',  ( 42.47499999726880304, 149.9369285172503510, 15.58253174999999580 ) ) ;
#24426 = LINE ( 'NONE', #21860, #24152 ) ;
#24427 = CARTESIAN_POINT ( 'NONE',  ( 2.426778023690261410, 199.3768101843759837, 95.60113791807857808 ) ) ;
#24428 = AXIS2_PLACEMENT_3D ( 'NONE', #28311, #21131, #10594 ) ;
#24429 = CARTESIAN_POINT ( 'NONE',  ( 56.50000000000000000, 155.0000000000000000, -14.50000000000000711 ) ) ;
#24430 = CYLINDRICAL_SURFACE ( 'NONE', #8761, 19.99999999999998934 ) ;
#24431 = CARTESIAN_POINT ( 'NONE',  ( -2.517493886309087880, 214.5937144450984135, 69.09886208192143897 ) ) ;
#24432 = LINE ( 'NONE', #27157, #27605 ) ;
#24433 = DIRECTION ( 'NONE',  ( -6.106226635438360972E-16, 0.04769215134144213358, -0.9988620819214358848 ) ) ;
#24434 = CARTESIAN_POINT ( 'NONE',  ( 58.32499999726881157, 145.8408176439707802, 12.60653300113718345 ) ) ;
#24435 = CARTESIAN_POINT ( 'NONE',  ( -3.135527875058821579, 197.5041725223112223, 11.90113791807856636 ) ) ;
#24436 = DIRECTION ( 'NONE',  ( 0.000000000000000000, 0.000000000000000000, -1.000000000000000000 ) ) ;
#24437 = CARTESIAN_POINT ( 'NONE',  ( 67.52499999726880731, 169.8198683612136222, -4.815267126137197984 ) ) ;
#24438 = CARTESIAN_POINT ( 'NONE',  ( 79.27499999726880731, 149.9369285172503510, -15.58253175000000823 ) ) ;
#24439 = CARTESIAN_POINT ( 'NONE',  ( 3.753561863808689836, 218.3979405102790565, 76.40113791807856103 ) ) ;
#24440 = CARTESIAN_POINT ( 'NONE',  ( -9.984503880673475606, 210.2968891136704315, 93.65113791807857524 ) ) ;
#24441 = CARTESIAN_POINT ( 'NONE',  ( -10.47863426674271814, 207.9189531262114770, 102.6635298682156758 ) ) ;
#24442 = EDGE_LOOP ( 'NONE', ( #31658, #3994, #22527, #20978 ) ) ;
#24443 = CARTESIAN_POINT ( 'NONE',  ( 10.01549611932659545, 203.7984951890123853, 4.148862081921434353 ) ) ;
#24444 = CARTESIAN_POINT ( 'NONE',  ( -0.05014649552828442242, 219.6175466908591716, 60.24886208192143755 ) ) ;
#24445 = CARTESIAN_POINT ( 'NONE',  ( -10.00000000000000711, 206.9523078486584495, 68.49886208192143044 ) ) ;
#24446 = CARTESIAN_POINT ( 'NONE',  ( 3.662846001189864698, 218.4274158808046593, 6.398862081921435241 ) ) ;
#24447 = CARTESIAN_POINT ( 'NONE',  ( -5.978033218201117549, -4.054134411712201569, -0.5602453477493345435 ) ) ;
#24448 = CARTESIAN_POINT ( 'NONE',  ( 3.044812012440130555, 197.4746971517856764, 23.60113791807857098 ) ) ;
#24449 = CARTESIAN_POINT ( 'NONE',  ( -6.139770520408224463, 198.4640165459539389, 86.04886208192144181 ) ) ;
#24450 = ADVANCED_FACE ( 'NONE', ( #27003 ), #13310, .T. ) ;
#24451 =( REPRESENTATION_RELATIONSHIP ('NONE','NONE', #25663, #22175 ) REPRESENTATION_RELATIONSHIP_WITH_TRANSFORMATION ( #24845 )SHAPE_REPRESENTATION_RELATIONSHIP( ) );
#24452 = VERTEX_POINT ( 'NONE', #28194 ) ;
#24453 = DIRECTION ( 'NONE',  ( -1.000000000000000000, 0.000000000000000000, 0.000000000000000000 ) ) ;
#24454 = EDGE_LOOP ( 'NONE', ( #4263, #31538, #13356 ) ) ;
#24455 = CARTESIAN_POINT ( 'NONE',  ( 43.71132485994280614, 155.0000000000000000, -15.00000000000002487 ) ) ;
#24456 = CARTESIAN_POINT ( 'NONE',  ( 8.015496119326595448, 204.4483345814782638, 70.14886208192142192 ) ) ;
#24457 = ORIENTED_EDGE ( 'NONE', *, *, #10027, .F. ) ;
#24458 = CARTESIAN_POINT ( 'NONE',  ( 86.32499999726880446, 145.8408176439707802, 12.60653300113718345 ) ) ;
#24459 = ORIENTED_EDGE ( 'NONE', *, *, #212, .F. ) ;
#24460 = DIRECTION ( 'NONE',  ( 1.000000000000000000, -0.000000000000000000, -0.000000000000000000 ) ) ;
#24461 = CIRCLE ( 'NONE', #33177, 0.4000000000000001887 ) ;
#24462 = CARTESIAN_POINT ( 'NONE',  ( 76.12499999726881583, 155.0000000000000000, 15.58253174999999402 ) ) ;
#24463 = CARTESIAN_POINT ( 'NONE',  ( 6.500168698208129925, 211.6636982574063381, 67.70113791807857240 ) ) ;
#24464 = CARTESIAN_POINT ( 'NONE',  ( 75.18867513459481700, 169.2658477444273331, -4.635254915624224203 ) ) ;
#24465 = SURFACE_STYLE_USAGE ( .BOTH. , #32126 ) ;
#24466 = CARTESIAN_POINT ( 'NONE',  ( 36.60000000000000853, 159.7113355953771077, -14.50000000000000888 ) ) ;
#24467 = CARTESIAN_POINT ( 'NONE',  ( 4.984841277089891776, 200.2242689037093726, 46.44886208192144039 ) ) ;
#24468 = CARTESIAN_POINT ( 'NONE',  ( 8.062137200540920645, 201.0835637161417822, 86.30113791807856671 ) ) ;
#24469 = CARTESIAN_POINT ( 'NONE',  ( -0.05014649552810635652, 196.4853777576173002, 62.75113791807856956 ) ) ;
#24470 = DIRECTION ( 'NONE',  ( 0.000000000000000000, -1.000000000000000000, 3.227392513445223895E-15 ) ) ;
#24471 = CARTESIAN_POINT ( 'NONE',  ( 8.000000000000008882, 206.9523078486586485, 23.00113791807856600 ) ) ;
#24472 = DIRECTION ( 'NONE',  ( 0.000000000000000000, 0.000000000000000000, 1.000000000000000000 ) ) ;
#24473 = DIRECTION ( 'NONE',  ( 0.1045284632676459352, 1.217938055844715641E-16, 0.9945218953682740670 ) ) ;
#24474 = CARTESIAN_POINT ( 'NONE',  ( 51.72499999726881725, 169.8198683612136222, 4.815267126137181997 ) ) ;
#24475 = CARTESIAN_POINT ( 'NONE',  ( -11.98450388067348804, 210.9467285061362247, 48.65113791807857524 ) ) ;
#24476 = CARTESIAN_POINT ( 'NONE',  ( 32.50000000000000000, 155.0000000000000000, 15.00000000000001243 ) ) ;
#24477 = CARTESIAN_POINT ( 'NONE',  ( -8.062137200540920645, 212.9164362838581894, 93.80113791807858092 ) ) ;
#24478 = CARTESIAN_POINT ( 'NONE',  ( -10.00000000000000711, 207.0476921513413515, 69.50113791807856956 ) ) ;
#24479 = CARTESIAN_POINT ( 'NONE',  ( 0.05014649552828288198, 194.3824533091408000, 34.74886208192142334 ) ) ;
#24480 = CARTESIAN_POINT ( 'NONE',  ( -3.135527875058982783, 216.4958274776886924, 36.09886208192143897 ) ) ;
#24481 = CARTESIAN_POINT ( 'NONE',  ( 84.09999999453761177, 159.7113355953771077, -14.50000000000000888 ) ) ;
#24482 = CARTESIAN_POINT ( 'NONE',  ( -7.375838497908182134, 217.2372850707499765, 81.95113791807858661 ) ) ;
#24483 = CARTESIAN_POINT ( 'NONE',  ( 6.444103211791042618, 202.2591342207267644, 95.30113791807858092 ) ) ;
#24484 = CARTESIAN_POINT ( 'NONE',  ( 3.135527875058981895, 197.5041725223112792, 58.59886208192143897 ) ) ;
#24485 = ADVANCED_FACE ( 'NONE', ( #12182, #12349 ), #27841, .T. ) ;
#24486 = DIRECTION ( 'NONE',  ( -0.000000000000000000, -0.000000000000000000, 1.000000000000000000 ) ) ;
#24487 = ORIENTED_EDGE ( 'NONE', *, *, #11621, .F. ) ;
#24488 = CARTESIAN_POINT ( 'NONE',  ( -0.05014649552828442242, 219.6175466908591716, 66.24886208192143044 ) ) ;
#24489 = ORIENTED_EDGE ( 'NONE', *, *, #17951, .T. ) ;
#24490 = CARTESIAN_POINT ( 'NONE',  ( 70.67499999726881299, 141.7447067706911810, 9.630534252274376428 ) ) ;
#24491 = CARTESIAN_POINT ( 'NONE',  ( -2.517493886309087880, 214.5937144450984135, 39.09886208192143897 ) ) ;
#24492 = EDGE_CURVE ( 'NONE', #16783, #32368, #1640, .T. ) ;
#24493 = ORIENTED_EDGE ( 'NONE', *, *, #19093, .T. ) ;
#24494 = CARTESIAN_POINT ( 'NONE',  ( 84.27499999726879309, 160.0630714827496206, 15.58253174999999224 ) ) ;
#24495 = DIRECTION ( 'NONE',  ( 1.000000000000000000, 0.000000000000000000, 0.000000000000000000 ) ) ;
#24496 = ADVANCED_FACE ( 'NONE', ( #7076 ), #20557, .F. ) ;
#24497 = CARTESIAN_POINT ( 'NONE',  ( -125.0000000000000000, -25.00000000000000000, -20.00000000000000000 ) ) ;
#24498 = CARTESIAN_POINT ( 'NONE',  ( -6.500168698208129925, 202.3363017425936050, 54.20113791807857240 ) ) ;
#24499 = PRESENTATION_STYLE_ASSIGNMENT (( #13768 ) ) ;
#24500 = CARTESIAN_POINT ( 'NONE',  ( 8.118202686958138514, 201.1607312380088501, 28.29886208192143471 ) ) ;
#24501 = CARTESIAN_POINT ( 'NONE',  ( 68.77499999726880731, 140.1801316387863778, 4.815267126137185549 ) ) ;
#24502 = ORIENTED_EDGE ( 'NONE', *, *, #31210, .F. ) ;
#24503 = CARTESIAN_POINT ( 'NONE',  ( 36.31132485994280046, 169.2658477444273331, 4.635254915624208216 ) ) ;
#24504 = FILL_AREA_STYLE ('',( #14110 ) ) ;
#24505 = CARTESIAN_POINT ( 'NONE',  ( -47.49999999999998579, 155.0000000000000000, -12.00000000000001066 ) ) ;
#24506 = FACE_OUTER_BOUND ( 'NONE', #22063, .T. ) ;
#24507 = CARTESIAN_POINT ( 'NONE',  ( -4.984841277089891776, 213.7757310962905990, 17.94886208192143684 ) ) ;
#24508 = CARTESIAN_POINT ( 'NONE',  ( -8.062137200540920645, 212.9164362838581894, 63.80113791807858092 ) ) ;
#24509 = PRODUCT_DEFINITION_SHAPE ( 'NONE', 'NONE',  #33697 ) ;
#24510 = CARTESIAN_POINT ( 'NONE',  ( -0.05014649552810635652, 196.4853777576173002, 35.75113791807857666 ) ) ;
#24511 = CARTESIAN_POINT ( 'NONE',  ( 66.78867513459482552, 155.0000000000000000, -15.00000000000002487 ) ) ;
#24512 = CARTESIAN_POINT ( 'NONE',  ( 2.426778023690261410, 199.3768101843759837, -0.3988620819214340751 ) ) ;
#24513 = CARTESIAN_POINT ( 'NONE',  ( 44.92499999726880588, 145.8408176439707802, -12.60653300113719588 ) ) ;
#24514 = FACE_OUTER_BOUND ( 'NONE', #9603, .T. ) ;
#24515 = DIRECTION ( 'NONE',  ( 0.000000000000000000, 0.000000000000000000, -1.000000000000000000 ) ) ;
#24516 = CARTESIAN_POINT ( 'NONE',  ( 0.05014649552807549926, 219.6175466908591716, 19.25113791807856245 ) ) ;
#24517 = DIRECTION ( 'NONE',  ( -1.000000000000000000, 0.000000000000000000, 0.000000000000000000 ) ) ;
#24518 = EDGE_CURVE ( 'NONE', #13858, #30073, #17458, .T. ) ;
#24519 = CARTESIAN_POINT ( 'NONE',  ( -6.139770520408369237, 215.5359834540460042, 69.95113791807857240 ) ) ;
#24520 = CARTESIAN_POINT ( 'NONE',  ( -10.00000000000000711, 207.0476921513413515, 36.50113791807857666 ) ) ;
#24521 = AXIS2_PLACEMENT_3D ( 'NONE', #20462, #26082, #13290 ) ;
#24522 = LINE ( 'NONE', #25189, #23019 ) ;
#24523 = CARTESIAN_POINT ( 'NONE',  ( 4.515071337844632104, 29.14748715311447924, -16.91127448208919049 ) ) ;
#24524 = CARTESIAN_POINT ( 'NONE',  ( 9.736236675708031640, 199.9851607334238963, 7.298862081921434708 ) ) ;
#24525 = CARTESIAN_POINT ( 'NONE',  ( 8.118202686958138514, 201.1607312380088501, 10.29886208192143471 ) ) ;
#24526 = CIRCLE ( 'NONE', #28878, 19.99999999999998934 ) ;
#24527 = CARTESIAN_POINT ( 'NONE',  ( 68.59999999453762598, 168.7903194862797420, 4.480746418436729606 ) ) ;
#24528 = VERTEX_POINT ( 'NONE', #30753 ) ;
#24529 = CARTESIAN_POINT ( 'NONE',  ( -3.753561863808691168, 195.6020594897209435, 50.90113791807858235 ) ) ;
#24530 = CARTESIAN_POINT ( 'NONE',  ( -8.000000000000008882, 207.0476921513413515, 69.50113791807856956 ) ) ;
#24531 = CARTESIAN_POINT ( 'NONE',  ( 90.49452189536829394, 155.0000000000000000, -32.10452846326766974 ) ) ;
#24532 = CARTESIAN_POINT ( 'NONE',  ( 10.00000000000000711, 207.0476921513415220, 33.99886208192143044 ) ) ;
#24533 = EDGE_CURVE ( 'NONE', #5476, #6338, #33472, .T. ) ;
#24534 = CYLINDRICAL_SURFACE ( 'NONE', #10156, 15.00000000000001776 ) ;
#24535 = EDGE_LOOP ( 'NONE', ( #24457, #9355, #30787, #14361 ) ) ;
#24536 = CARTESIAN_POINT ( 'NONE',  ( 3.044812012440130555, 197.4746971517856764, 80.60113791807857808 ) ) ;
#24537 = ORIENTED_EDGE ( 'NONE', *, *, #30367, .T. ) ;
#24538 = LINE ( 'NONE', #6300, #33624 ) ;
#24539 = CARTESIAN_POINT ( 'NONE',  ( 10.00000000000000888, 207.8771832641648984, -0.04188241574673567946 ) ) ;
#24540 = ORIENTED_EDGE ( 'NONE', *, *, #22643, .T. ) ;
#24541 = CARTESIAN_POINT ( 'NONE',  ( 6.444103211791042618, 202.2591342207267644, 26.30113791807856316 ) ) ;
#24542 = EDGE_CURVE ( 'NONE', #29281, #1664, #7508, .T. ) ;
#24543 = CARTESIAN_POINT ( 'NONE',  ( -59.14727863148851839, 194.9267258542059835, 2.420242894197758510 ) ) ;
#24544 = CARTESIAN_POINT ( 'NONE',  ( -3.662846001189865142, 195.5725841191952838, 103.8988620819214361 ) ) ;
#24545 = CARTESIAN_POINT ( 'NONE',  ( 48.67499999726881299, 141.7447067706911810, 9.630534252274376428 ) ) ;
#24546 = EDGE_LOOP ( 'NONE', ( #22694, #29227, #2216, #19976 ) ) ;
#24547 = CARTESIAN_POINT ( 'NONE',  ( 55.52499999726881441, 169.8198683612136222, -4.815267126137197984 ) ) ;
#24548 = CARTESIAN_POINT ( 'NONE',  ( -6.444103211791042618, 211.7408657792732356, 48.80113791807858092 ) ) ;
#24549 = CARTESIAN_POINT ( 'NONE',  ( 7.808623696107343193, 4.508310992947586193, -7.999704684617482187 ) ) ;
#24550 = AXIS2_PLACEMENT_3D ( 'NONE', #25437, #9431, #12324 ) ;
#24551 = CYLINDRICAL_SURFACE ( 'NONE', #29314, 3.399999999999999911 ) ;
#24552 = CARTESIAN_POINT ( 'NONE',  ( 9.984503880673420539, 210.2968891136705167, 93.84886208192143897 ) ) ;
#24553 = CARTESIAN_POINT ( 'NONE',  ( 61.97499999726881015, 169.8198683612136222, 4.815267126137181997 ) ) ;
#24554 = CARTESIAN_POINT ( 'NONE',  ( 3.135527875058820690, 216.4958274776887492, 22.40113791807856458 ) ) ;
#24555 = CARTESIAN_POINT ( 'NONE',  ( 87.50000000000001421, 155.0000000000000000, 15.00000000000001243 ) ) ;
#24556 = EDGE_CURVE ( 'NONE', #13276, #16396, #10600, .T. ) ;
#24557 = CARTESIAN_POINT ( 'NONE',  ( 3.662846001189864698, 218.4274158808046593, 81.39886208192143613 ) ) ;
#24558 = CARTESIAN_POINT ( 'NONE',  ( 80.30000000000001137, 146.4771138417591203, -11.73074641843674470 ) ) ;
#24559 = CARTESIAN_POINT ( 'NONE',  ( 40.58867513459482268, 146.1832212156128890, -12.13525491562423042 ) ) ;
#24560 = CARTESIAN_POINT ( 'NONE',  ( -0.05014649552810635652, 196.4853777576173002, 95.75113791807856956 ) ) ;
#24561 = DIRECTION ( 'NONE',  ( -0.000000000000000000, -0.000000000000000000, 1.000000000000000000 ) ) ;
#24562 = CARTESIAN_POINT ( 'NONE',  ( 47.37499999726880873, 155.0000000000000000, -15.58253175000000823 ) ) ;
#24563 = EDGE_CURVE ( 'NONE', #24261, #28270, #16656, .T. ) ;
#24564 = CARTESIAN_POINT ( 'NONE',  ( -0.05014649552810635652, 196.4853777576173002, 35.75113791807857666 ) ) ;
#24565 = CARTESIAN_POINT ( 'NONE',  ( 79.02499999726879309, 149.9369285172503510, -15.58253175000000823 ) ) ;
#24566 = VERTEX_POINT ( 'NONE', #22910 ) ;
#24567 = CARTESIAN_POINT ( 'NONE',  ( -3.288228914120473245, 7.217643567644804747, -7.591235721156635030 ) ) ;
#24568 = CARTESIAN_POINT ( 'NONE',  ( -60.00000000000000000, -7.347880794884118356E-15, -20.00000000000001776 ) ) ;
#24569 = CARTESIAN_POINT ( 'NONE',  ( 46.29999999453762882, 167.3344367211045096, -8.961492836873482304 ) ) ;
#24570 =( BOUNDED_SURFACE ( )  B_SPLINE_SURFACE ( 3, 2, ( 
 ( #33413, #17914, #28305 ),
 ( #11410, #21960, #6110 ),
 ( #3564, #21461, #5776 ),
 ( #5948, #16507, #18901 ),
 ( #27072, #5621, #21620 ),
 ( #3734, #10913, #26561 ),
 ( #29459, #32014, #13453 ),
 ( #31843, #16338, #3231 ) ),
 .UNSPECIFIED., .F., .F., .F. ) 
 B_SPLINE_SURFACE_WITH_KNOTS ( ( 4, 2, 2, 4 ),
 ( 3, 3 ),
 ( 0.03861844051980971304, 0.04325213341840643266, 0.04556897986770479247, 0.04788582631700314535 ),
 ( 0.000000000000000000, 1.000000000000000000 ),
 .UNSPECIFIED. ) 
 GEOMETRIC_REPRESENTATION_ITEM ( )  RATIONAL_B_SPLINE_SURFACE ( (
 ( 1.000000000000000000, 0.8047781759831919013, 1.000000000000000000),
 ( 1.000000000000000000, 0.8123762462802479600, 1.000000000000000000),
 ( 1.000000000000000000, 0.8190659850620179983, 1.000000000000000000),
 ( 1.000000000000000000, 0.8191937571011910224, 1.000000000000000000),
 ( 1.000000000000000000, 0.8176092952781196521, 1.000000000000000000),
 ( 1.000000000000000000, 0.8122962088595743202, 1.000000000000000000),
 ( 1.000000000000000000, 0.8086311330828506172, 1.000000000000000000),
 ( 1.000000000000000000, 0.8047712282214323221, 1.000000000000000000) ) ) 
 REPRESENTATION_ITEM ( '' )  SURFACE ( )  );
#24571 = CARTESIAN_POINT ( 'NONE',  ( -9.736236675707914401, 199.9851607334237542, 18.20113791807856529 ) ) ;
#24572 = CARTESIAN_POINT ( 'NONE',  ( 8.000000000000000000, 0.000000000000000000, 0.000000000000000000 ) ) ;
#24573 = FACE_OUTER_BOUND ( 'NONE', #31051, .T. ) ;
#24574 = ORIENTED_EDGE ( 'NONE', *, *, #11903, .F. ) ;
#24575 = CIRCLE ( 'NONE', #18041, 2.149999999999985256 ) ;
#24576 = CARTESIAN_POINT ( 'NONE',  ( -11.98450388067341876, 203.0532714938636047, 41.34886208192143187 ) ) ;
#24577 = CARTESIAN_POINT ( 'NONE',  ( 0.000000000000000000, 0.000000000000000000, 9.480888224575629408 ) ) ;
#24578 = CARTESIAN_POINT ( 'NONE',  ( 0.05014649552810505201, 217.5146222423826714, 55.25113791807858377 ) ) ;
#24579 = CARTESIAN_POINT ( 'NONE',  ( 6.444103211790928043, 211.7408657792734061, 12.69886208192143684 ) ) ;
#24580 = CARTESIAN_POINT ( 'NONE',  ( 125.5000000000000000, 155.0000000000000000, -100.0000000000000284 ) ) ;
#24581 = ORIENTED_EDGE ( 'NONE', *, *, #8451, .T. ) ;
#24582 = CIRCLE ( 'NONE', #9902, 6.500000000000000888 ) ;
#24583 = CARTESIAN_POINT ( 'NONE',  ( 7.984503880673422316, 209.6470497212048372, 99.84886208192143897 ) ) ;
#24584 = EDGE_CURVE ( 'NONE', #5650, #23379, #30914, .T. ) ;
#24585 = ADVANCED_FACE ( 'NONE', ( #20014 ), #29823, .T. ) ;
#24586 = DIRECTION ( 'NONE',  ( 1.000000000000000000, -0.000000000000000000, -0.000000000000000000 ) ) ;
#24587 = CARTESIAN_POINT ( 'NONE',  ( 7.984503880673485376, 204.3529502787953902, 44.15113791807857524 ) ) ;
#24588 = FACE_OUTER_BOUND ( 'NONE', #23710, .T. ) ;
#24589 = ORIENTED_EDGE ( 'NONE', *, *, #4877, .F. ) ;
#24590 = CARTESIAN_POINT ( 'NONE',  ( 37.52499999726881441, 169.8198683612136222, -4.815267126137197984 ) ) ;
#24591 = FACE_OUTER_BOUND ( 'NONE', #25292, .T. ) ;
#24592 = CARTESIAN_POINT ( 'NONE',  ( -6.139770520408224463, 198.4640165459539389, 59.04886208192143471 ) ) ;
#24593 = CARTESIAN_POINT ( 'NONE',  ( 38.57499999726881157, 145.8408176439707802, 12.60653300113718345 ) ) ;
#24594 = DIRECTION ( 'NONE',  ( 0.000000000000000000, -0.04769215134144031559, 0.9988620819214357738 ) ) ;
#24595 = CARTESIAN_POINT ( 'NONE',  ( -4.984841277089726574, 200.2242689037092305, 99.05113791807858092 ) ) ;
#24596 = ADVANCED_FACE ( 'NONE', ( #30241 ), #6899, .F. ) ;
#24597 = CIRCLE ( 'NONE', #14253, 0.9999999999999915623 ) ;
#24598 = CARTESIAN_POINT ( 'NONE',  ( 55.19999999999998863, 167.3344367211045096, 8.961492836873468093 ) ) ;
#24599 = CARTESIAN_POINT ( 'NONE',  ( 59.71132485994280614, 155.0000000000000000, -15.00000000000002487 ) ) ;
#24600 = CARTESIAN_POINT ( 'NONE',  ( 2.426778023690075337, 214.6231898156240447, 84.39886208192143613 ) ) ;
#24601 = CARTESIAN_POINT ( 'NONE',  ( -5.698650001973517121, 4.592339236403562452, -6.344532336093705815 ) ) ;
#24602 = CARTESIAN_POINT ( 'NONE',  ( 115.4999999999999858, 63.20130719884917170, -52.99999999999946709 ) ) ;
#24603 = CARTESIAN_POINT ( 'NONE',  ( 59.42499999726882010, 168.2552932293087906, -9.630534252274385310 ) ) ;
#24605 = ORIENTED_EDGE ( 'NONE', *, *, #15204, .T. ) ;
#24604 = CARTESIAN_POINT ( 'NONE',  ( -3.135527875058821579, 197.5041725223112223, 20.90113791807856813 ) ) ;
#24606 = DIRECTION ( 'NONE',  ( 0.000000000000000000, 0.000000000000000000, 1.000000000000000000 ) ) ;
#24607 = CIRCLE ( 'NONE', #28959, 2.499999999999988454 ) ;
#24608 = CARTESIAN_POINT ( 'NONE',  ( 83.47499999726881015, 160.0630714827496206, -15.58253175000000823 ) ) ;
#24609 = CARTESIAN_POINT ( 'NONE',  ( 0.05014649552807549926, 219.6175466908591716, 82.25113791807856956 ) ) ;
#24610 = CIRCLE ( 'NONE', #27939, 4.199999999999988631 ) ;
#24611 = CARTESIAN_POINT ( 'NONE',  ( 71.78867513459482552, 155.0000000000000000, 15.00000000000001243 ) ) ;
#24612 = CARTESIAN_POINT ( 'NONE',  ( -64.50000000000000000, -95.00000000000000000, 270.4495957273638282 ) ) ;
#24613 = ORIENTED_EDGE ( 'NONE', *, *, #8927, .F. ) ;
#24614 = CARTESIAN_POINT ( 'NONE',  ( 0.05014649552828275708, 196.4853777576173002, 4.748862081921434886 ) ) ;
#24615 = CARTESIAN_POINT ( 'NONE',  ( 12.01549611932659367, 203.1486557965466773, 58.14886208192143613 ) ) ;
#24616 = CARTESIAN_POINT ( 'NONE',  ( -3.044812012439970683, 197.4746971517856196, 76.89886208192143613 ) ) ;
#24617 = CARTESIAN_POINT ( 'NONE',  ( 7.456977232089471386, 196.8216656703012006, 10.44886208192143506 ) ) ;
#24618 = CARTESIAN_POINT ( 'NONE',  ( 16.00000000000000000, 0.000000000000000000, -16.57418492358057094 ) ) ;
#24619 = CARTESIAN_POINT ( 'NONE',  ( -9.984503880673473830, 210.2968891136704315, 21.65113791807856458 ) ) ;
#24620 = CARTESIAN_POINT ( 'NONE',  ( 6.139770520408223575, 215.5359834540460611, 87.54886208192142760 ) ) ;
#24621 = ORIENTED_EDGE ( 'NONE', *, *, #13554, .T. ) ;
#24622 = AXIS2_PLACEMENT_3D ( 'NONE', #9224, #1892, #30005 ) ;
#24623 = CARTESIAN_POINT ( 'NONE',  ( 63.41132485994281609, 142.2402378747194405, -9.270509831248439525 ) ) ;
#24624 = ORIENTED_EDGE ( 'NONE', *, *, #11020, .T. ) ;
#24625 = DIRECTION ( 'NONE',  ( 1.000000000000000000, -0.000000000000000000, -0.000000000000000000 ) ) ;
#24626 = CARTESIAN_POINT ( 'NONE',  ( -4.984841277089891776, 213.7757310962905990, 74.94886208192143329 ) ) ;
#24627 = ORIENTED_EDGE ( 'NONE', *, *, #30981, .T. ) ;
#24628 = CARTESIAN_POINT ( 'NONE',  ( 83.52499999726880731, 169.8198683612136222, -4.815267126137197984 ) ) ;
#24629 = ORIENTED_EDGE ( 'NONE', *, *, #25199, .T. ) ;
#24630 = DIRECTION ( 'NONE',  ( 1.000000000000000000, 0.000000000000000000, 0.000000000000000000 ) ) ;
#24631 = AXIS2_PLACEMENT_3D ( 'NONE', #28183, #2126, #25797 ) ;
#24632 = CIRCLE ( 'NONE', #21897, 1.649999999999999911 ) ;
#24633 = CARTESIAN_POINT ( 'NONE',  ( 73.92499999726881299, 164.1591823560292198, 12.60653300113718167 ) ) ;
#24634 = CARTESIAN_POINT ( 'NONE',  ( -4.903702542908602524, 213.8346818373418898, 66.95113791807857240 ) ) ;
#24635 = CARTESIAN_POINT ( 'NONE',  ( 75.28867513459483973, 170.7719333635740497, -7.904646289410545231E-15 ) ) ;
#24636 = CARTESIAN_POINT ( 'NONE',  ( 32.50000000000000000, 155.0000000000000000, -14.50000000000000711 ) ) ;
#24637 = CARTESIAN_POINT ( 'NONE',  ( -4.903702542908436435, 200.1653181626580249, 47.04886208192144892 ) ) ;
#24638 = CARTESIAN_POINT ( 'NONE',  ( 0.05014649552810505201, 217.5146222423826714, 94.25113791807855534 ) ) ;
#24639 = CARTESIAN_POINT ( 'NONE',  ( 10.01549611932653860, 210.2015048109876716, 73.85113791807857808 ) ) ;
#24640 = VECTOR ( 'NONE', #31199, 1000.000000000000000 ) ;
#24641 = CARTESIAN_POINT ( 'NONE',  ( 4.000000000000000000, -2.639212418033078489, -1.523749999999997273 ) ) ;
#24642 = CARTESIAN_POINT ( 'NONE',  ( -27.50000000000000000, 2.688867821578071471, -17.94295719123740085 ) ) ;
#24643 = CARTESIAN_POINT ( 'NONE',  ( 115.4999999999999858, 54.13214199290997186, 25.91453920131690936 ) ) ;
#24644 = CARTESIAN_POINT ( 'NONE',  ( 52.32499999726881157, 145.8408176439707802, 12.60653300113718345 ) ) ;
#24645 = CARTESIAN_POINT ( 'NONE',  ( 12.01549611932652972, 210.8513442034534933, 52.85113791807857098 ) ) ;
#24646 = DIRECTION ( 'NONE',  ( -0.000000000000000000, -0.000000000000000000, 1.000000000000000000 ) ) ;
#24647 = PRODUCT_DEFINITION_SHAPE ( 'NONE', 'NONE',  #21056 ) ;
#24648 = CARTESIAN_POINT ( 'NONE',  ( 7.456977232089302632, 217.1783343296989131, 4.551137918078565825 ) ) ;
#24649 = CARTESIAN_POINT ( 'NONE',  ( -8.062137200540920645, 212.9164362838581894, 63.80113791807858092 ) ) ;
#24650 = CARTESIAN_POINT ( 'NONE',  ( -12.01549611932659722, 210.8513442034533227, 32.64886208192143613 ) ) ;
#24651 = CARTESIAN_POINT ( 'NONE',  ( 9.984503880673420539, 210.2968891136705736, 48.84886208192143187 ) ) ;
#24652 = CARTESIAN_POINT ( 'NONE',  ( 85.79999999453762882, 146.4771138417591203, -11.73074641843674470 ) ) ;
#24653 = AXIS2_PLACEMENT_3D ( 'NONE', #12494, #33274, #17768 ) ;
#24654 = CARTESIAN_POINT ( 'NONE',  ( 12.01549611932652972, 210.8513442034534933, 79.85113791807857808 ) ) ;
#24655 = CARTESIAN_POINT ( 'NONE',  ( 4.984841277089725686, 213.7757310962907411, 97.55113791807858092 ) ) ;
#24656 = CIRCLE ( 'NONE', #11044, 5.999999999999995559 ) ;
#24657 = CARTESIAN_POINT ( 'NONE',  ( 6.220909254589681581, 198.5229672870052582, 64.44886208192143329 ) ) ;
#24658 = CONICAL_SURFACE ( 'NONE', #9985, 12.00000000000000355, 0.7853981633974503884 ) ;
#24659 = FILL_AREA_STYLE_COLOUR ( '', #21613 ) ;
#24660 = ORIENTED_EDGE ( 'NONE', *, *, #20858, .F. ) ;
#24661 = CARTESIAN_POINT ( 'NONE',  ( 9.736236675708031640, 199.9851607334238963, 61.29886208192144892 ) ) ;
#24662 = ORIENTED_EDGE ( 'NONE', *, *, #24164, .T. ) ;
#24663 = CARTESIAN_POINT ( 'NONE',  ( 68.87499999726881583, 138.6155565068815463, -3.929120461958505118E-15 ) ) ;
#24664 = CARTESIAN_POINT ( 'NONE',  ( 8.000000000000008882, 207.0476921513415220, 45.99886208192144466 ) ) ;
#24665 = ORIENTED_EDGE ( 'NONE', *, *, #33511, .T. ) ;
#24666 = CARTESIAN_POINT ( 'NONE',  ( 81.97499999726881015, 169.8198683612136222, 4.815267126137181997 ) ) ;
#24667 = FACE_OUTER_BOUND ( 'NONE', #2351, .T. ) ;
#24668 = AXIS2_PLACEMENT_3D ( 'NONE', #20427, #31154, #30820 ) ;
#24669 = DIRECTION ( 'NONE',  ( 0.000000000000000000, -1.000000000000000000, 9.682177540335733218E-15 ) ) ;
#24670 = CARTESIAN_POINT ( 'NONE',  ( 8.015496119326531499, 209.5516654185219636, 49.85113791807857808 ) ) ;
#24671 = CARTESIAN_POINT ( 'NONE',  ( 6.139770520408223575, 215.5359834540460611, 30.54886208192142760 ) ) ;
#24672 = CARTESIAN_POINT ( 'NONE',  ( 71.57499999726881867, 164.1591823560292198, -12.60653300113719766 ) ) ;
#24673 = ORIENTED_EDGE ( 'NONE', *, *, #32082, .F. ) ;
#24674 = PLANE ( 'NONE',  #18918 ) ;
#24675 =( BOUNDED_CURVE ( )  B_SPLINE_CURVE ( 2, ( #12271, #19936, #9720, #33228, #9379, #29999, #30169, #23004, #22498, #7001, #12446 ),
 .UNSPECIFIED., .F., .T. ) 
 B_SPLINE_CURVE_WITH_KNOTS ( ( 3, 2, 2, 2, 2, 3 ),
 ( 0.4107142857142856984, 0.4142857142857143127, 0.4178571428571428714, 0.4214285714285714302, 0.4249999999999999889, 0.4285714285714285476 ),
 .UNSPECIFIED. ) 
 CURVE ( )  GEOMETRIC_REPRESENTATION_ITEM ( )  RATIONAL_B_SPLINE_CURVE ( ( 1.000000000000000000, 0.9510565162951534202, 1.000000000000000000, 0.9510565162951534202, 1.000000000000000000, 0.9510565162951534202, 1.000000000000000000, 0.9510565162951534202, 1.000000000000000000, 0.9510565162951534202, 1.000000000000000000 ) ) 
 REPRESENTATION_ITEM ( '' )  );
#24676 = DIRECTION ( 'NONE',  ( -1.000000000000000000, 0.000000000000000000, 0.000000000000000000 ) ) ;
#24677 = CARTESIAN_POINT ( 'NONE',  ( 55.71132485994280614, 155.0000000000000000, -15.00000000000002487 ) ) ;
#24678 = CARTESIAN_POINT ( 'NONE',  ( -6.500168698208244500, 211.6636982574061676, 11.79886208192143648 ) ) ;
#24679 = AXIS2_PLACEMENT_3D ( 'NONE', #23911, #26300, #31742 ) ;
#24680 = CARTESIAN_POINT ( 'NONE',  ( -10.01549611932653860, 203.7984951890123284, 57.35113791807856387 ) ) ;
#24681 = ADVANCED_FACE ( 'NONE', ( #9619, #30417 ), #27095, .F. ) ;
#24682 = CARTESIAN_POINT ( 'NONE',  ( -6.139770520408369237, 215.5359834540460042, 42.95113791807856529 ) ) ;
#24683 = LINE ( 'NONE', #11564, #15065 ) ;
#24684 = AXIS2_PLACEMENT_3D ( 'NONE', #11091, #21471, #26573 ) ;
#24685 = CONTEXT_DEPENDENT_SHAPE_REPRESENTATION ( #26190, #6564 ) ;
#24686 = CARTESIAN_POINT ( 'NONE',  ( 8.000000000000008882, 207.0476921513415220, 102.9988620819214304 ) ) ;
#24687 = CARTESIAN_POINT ( 'NONE',  ( 41.92499999726881299, 164.1591823560292198, 12.60653300113718167 ) ) ;
#24688 = DIRECTION ( 'NONE',  ( 0.000000000000000000, -0.4999999999999995004, 0.8660254037844389297 ) ) ;
#24689 = CARTESIAN_POINT ( 'NONE',  ( 87.50000000000000000, 157.6678010926102047, -15.23241260079973536 ) ) ;
#24690 = CARTESIAN_POINT ( 'NONE',  ( -3.753561863808691168, 195.6020594897209435, 17.90113791807856458 ) ) ;
#24691 = CARTESIAN_POINT ( 'NONE',  ( 115.4999999999999858, 155.0000000000000000, -6.938893903907228378E-15 ) ) ;
#24692 = CARTESIAN_POINT ( 'NONE',  ( 10.00000000000000711, 206.9523078486586201, 65.00113791807856956 ) ) ;
#24693 = CARTESIAN_POINT ( 'NONE',  ( -6.139770520408368348, 215.5359834540460042, 39.95113791807857950 ) ) ;
#24694 = CARTESIAN_POINT ( 'NONE',  ( 127.5000000000000000, 80.04668119422662187, 74.95331880577468553 ) ) ;
#24695 = CIRCLE ( 'NONE', #6178, 2.149999999999999023 ) ;
#24696 = CARTESIAN_POINT ( 'NONE',  ( 27.50000000000000355, 15.87713240271474291, -2.456200930618646971 ) ) ;
#24697 = CARTESIAN_POINT ( 'NONE',  ( -11.98450388067341876, 203.0532714938636047, 8.348862081921435419 ) ) ;
#24698 = CARTESIAN_POINT ( 'NONE',  ( 10.00000000000000711, 207.0476921513415220, 12.99886208192143400 ) ) ;
#24699 = CARTESIAN_POINT ( 'NONE',  ( 66.39999999453763735, 168.7903194862797420, -4.480746418436745593 ) ) ;
#24700 = ORIENTED_EDGE ( 'NONE', *, *, #10784, .F. ) ;
#24701 = CARTESIAN_POINT ( 'NONE',  ( -9.736236675707914401, 199.9851607334237542, 51.20113791807856529 ) ) ;
#24702 = CARTESIAN_POINT ( 'NONE',  ( -4.903702542908602524, 213.8346818373418898, 72.95113791807857240 ) ) ;
#24703 = CARTESIAN_POINT ( 'NONE',  ( 8.062137200540822946, 212.9164362838583315, 27.69886208192143684 ) ) ;
#24704 = SURFACE_STYLE_USAGE ( .BOTH. , #14303 ) ;
#24705 = ORIENTED_EDGE ( 'NONE', *, *, #8477, .F. ) ;
#24706 = AXIS2_PLACEMENT_3D ( 'NONE', #2577, #28123, #18073 ) ;
#24707 = CARTESIAN_POINT ( 'NONE',  ( 10.00000000000000711, 206.9523078486586201, 86.00113791807858377 ) ) ;
#24708 = CONICAL_SURFACE ( 'NONE', #14372, 3.047499999999999876, 1.047197551196590748 ) ;
#24709 = ORIENTED_EDGE ( 'NONE', *, *, #4975, .T. ) ;
#24710 = CARTESIAN_POINT ( 'NONE',  ( 58.18867513459483121, 140.7341522555726669, 4.635254915624211769 ) ) ;
#24711 = CARTESIAN_POINT ( 'NONE',  ( 78.00000000000001421, 0.000000000000000000, 0.000000000000000000 ) ) ;
#24712 = VERTEX_POINT ( 'NONE', #11428 ) ;
#24713 = CARTESIAN_POINT ( 'NONE',  ( 0.05014649552807626948, 215.4116977939061144, 19.25113791807856245 ) ) ;
#24714 = EDGE_CURVE ( 'NONE', #18876, #6936, #20246, .T. ) ;
#24715 = CARTESIAN_POINT ( 'NONE',  ( -18.00000000000000355, 2.204364238465235822E-15, -25.03750572909317285 ) ) ;
#24716 = CARTESIAN_POINT ( 'NONE',  ( 10.01549611932659545, 203.7984951890123853, 1.148862081921433909 ) ) ;
#24717 = CARTESIAN_POINT ( 'NONE',  ( 53.07499999726880446, 141.7447067706911810, -9.630534252274387086 ) ) ;
#24718 = ORIENTED_EDGE ( 'NONE', *, *, #31036, .T. ) ;
#24719 = CARTESIAN_POINT ( 'NONE',  ( -6.500168698208129925, 202.3363017425936050, 45.20113791807857240 ) ) ;
#24720 = CARTESIAN_POINT ( 'NONE',  ( 67.61132485994281183, 150.1262045565062806, -14.99999999999993072 ) ) ;
#24721 = DIRECTION ( 'NONE',  ( 0.000000000000000000, 0.000000000000000000, 1.000000000000000000 ) ) ;
#24722 = CARTESIAN_POINT ( 'NONE',  ( -10.01549611932659722, 210.2015048109875011, 92.64886208192143613 ) ) ;
#24723 = CARTESIAN_POINT ( 'NONE',  ( 61.87499999726881583, 171.3844434931184253, -7.942151717890132712E-15 ) ) ;
#24724 = CARTESIAN_POINT ( 'NONE',  ( 6.220909254589536808, 215.4770327129947702, 34.55113791807855250 ) ) ;
#24725 = DIRECTION ( 'NONE',  ( 0.000000000000000000, 0.000000000000000000, -1.000000000000000000 ) ) ;
#24726 = EDGE_CURVE ( 'NONE', #24155, #7757, #15664, .T. ) ;
#24727 = CARTESIAN_POINT ( 'NONE',  ( 9.680171189290716072, 214.0920067884432854, 78.69886208192143329 ) ) ;
#24728 = B_SPLINE_CURVE_WITH_KNOTS ( 'NONE', 3,
 ( #17730, #17557, #27949, #11947 ),
 .UNSPECIFIED., .F., .F.,
 ( 4, 4 ),
 ( 2.380739282167303683E-07, 0.002044882221487520201 ),
 .UNSPECIFIED. ) ;
#24729 = CARTESIAN_POINT ( 'NONE',  ( 132.3999999999999773, 229.9533188057749555, 74.95331880577313655 ) ) ;
#24730 = VECTOR ( 'NONE', #18368, 1000.000000000000000 ) ;
#24731 = CARTESIAN_POINT ( 'NONE',  ( 79.80000000000002558, 142.6655632788954620, 8.961492836873471646 ) ) ;
#24732 = CARTESIAN_POINT ( 'NONE',  ( -56.51255670714900248, 194.9711358487265613, -1.525379346234926992 ) ) ;
#24733 = DIRECTION ( 'NONE',  ( 1.000000000000000000, 0.000000000000000000, 0.000000000000000000 ) ) ;
#24734 = CARTESIAN_POINT ( 'NONE',  ( 10.00000000000000711, 206.9523078486586201, 95.00113791807856956 ) ) ;
#24735 = CARTESIAN_POINT ( 'NONE',  ( 16.09259079475563325, -22.46320317811879264, -1.422337725029421129E-14 ) ) ;
#24736 = CARTESIAN_POINT ( 'NONE',  ( 41.37499999726880873, 155.0000000000000000, -15.58253175000000823 ) ) ;
#24737 = CARTESIAN_POINT ( 'NONE',  ( -8.062137200540920645, 212.9164362838581894, 33.80113791807857382 ) ) ;
#24738 = CARTESIAN_POINT ( 'NONE',  ( 81.92499999726882720, 164.1591823560292198, 12.60653300113718167 ) ) ;
#24739 = ADVANCED_FACE ( 'NONE', ( #5966 ), #16526, .T. ) ;
#24740 = DIRECTION ( 'NONE',  ( -0.000000000000000000, -0.000000000000000000, 1.000000000000000000 ) ) ;
#24741 = CARTESIAN_POINT ( 'NONE',  ( 18.00000000000000355, 0.000000000000000000, -25.03750572909317285 ) ) ;
#24742 = CARTESIAN_POINT ( 'NONE',  ( 46.09999999453762598, 159.7113355953771077, -14.50000000000000888 ) ) ;
#24743 = ORIENTED_EDGE ( 'NONE', *, *, #21846, .T. ) ;
#24744 = CARTESIAN_POINT ( 'NONE',  ( 0.05014649552807549926, 219.6175466908591716, 19.25113791807856245 ) ) ;
#24745 = CARTESIAN_POINT ( 'NONE',  ( -4.250000000000000000, 5.204748896376250699E-16, -9.449444346342714240 ) ) ;
#24746 = DIRECTION ( 'NONE',  ( 1.000000000000000000, -0.000000000000000000, -0.000000000000000000 ) ) ;
#24747 = ORIENTED_EDGE ( 'NONE', *, *, #25967, .F. ) ;
#24748 = CARTESIAN_POINT ( 'NONE',  ( -7.456977232089471386, 217.1783343296987709, 41.94886208192144039 ) ) ;
#24749 = CARTESIAN_POINT ( 'NONE',  ( -6.220909254589537696, 198.5229672870051161, 6.051137918078566713 ) ) ;
#24750 = CARTESIAN_POINT ( 'NONE',  ( 6.220909254589536808, 215.4770327129947702, 64.55113791807858092 ) ) ;
#24751 = EDGE_CURVE ( 'NONE', #20089, #31949, #31459, .T. ) ;
#24752 = CARTESIAN_POINT ( 'NONE',  ( 6.444103211790928043, 211.7408657792734061, 9.698862081921433287 ) ) ;
#24753 = PRODUCT_DEFINITION_CONTEXT ( 'detailed design', #31172, 'design' ) ;
#24754 = CARTESIAN_POINT ( 'NONE',  ( -52.50000000000002132, 155.0000000000000000, 6.938893903907228378E-15 ) ) ;
#24755 = ORIENTED_EDGE ( 'NONE', *, *, #13543, .T. ) ;
#24756 = CARTESIAN_POINT ( 'NONE',  ( -8.101690028313589309, 224.0100459381558267, 105.4832055762867782 ) ) ;
#24757 = EDGE_CURVE ( 'NONE', #20656, #15312, #17827, .T. ) ;
#24758 = DIRECTION ( 'NONE',  ( 0.000000000000000000, 0.5000000000000011102, 0.8660254037844379305 ) ) ;
#24759 = CARTESIAN_POINT ( 'NONE',  ( 2.517493886308900919, 214.5937144450984420, 43.40113791807856813 ) ) ;
#24760 = DIRECTION ( 'NONE',  ( 0.5526942671207023539, 0.1536855300543050473, 0.8190908404712123891 ) ) ;
#24761 = ORIENTED_EDGE ( 'NONE', *, *, #27431, .T. ) ;
#24762 = CARTESIAN_POINT ( 'NONE',  ( 37.22499999726881015, 160.0630714827496206, -15.58253175000000823 ) ) ;
#24763 = CARTESIAN_POINT ( 'NONE',  ( 39.28867513459483263, 170.7719333635740497, -7.904646289410545231E-15 ) ) ;
#24764 = CARTESIAN_POINT ( 'NONE',  ( -6.220909254589682469, 215.4770327129946850, 65.94886208192144750 ) ) ;
#24765 = CARTESIAN_POINT ( 'NONE',  ( 40.37499999726880873, 155.0000000000000000, 15.58253174999999402 ) ) ;
#24766 = CYLINDRICAL_SURFACE ( 'NONE', #31437, 3.500000000000000000 ) ;
#24767 = CARTESIAN_POINT ( 'NONE',  ( -0.05014649552810635652, 196.4853777576173002, -0.2488620819214343305 ) ) ;
#24768 = CARTESIAN_POINT ( 'NONE',  ( 63.60000000000000142, 150.2886644046228639, 14.49999999999999645 ) ) ;
#24769 = FACE_OUTER_BOUND ( 'NONE', #28321, .T. ) ;
#24770 = CARTESIAN_POINT ( 'NONE',  ( -2.517493886309087880, 214.5937144450984135, 84.09886208192143897 ) ) ;
#24771 = FACE_OUTER_BOUND ( 'NONE', #27682, .T. ) ;
#24772 = DIRECTION ( 'NONE',  ( 1.000000000000000000, 0.000000000000000000, 0.000000000000000000 ) ) ;
#24773 = CARTESIAN_POINT ( 'NONE',  ( 63.22499999726881725, 160.0630714827496206, -15.58253175000000823 ) ) ;
#24775 = EDGE_LOOP ( 'NONE', ( #11661, #30156, #14014, #6044 ) ) ;
#24774 = CARTESIAN_POINT ( 'NONE',  ( 3.135527875058820690, 216.4958274776887492, 16.40113791807856813 ) ) ;
#24776 = CARTESIAN_POINT ( 'NONE',  ( -63.50000000000004263, 215.0000000000000000, 0.000000000000000000 ) ) ;
#24777 = CARTESIAN_POINT ( 'NONE',  ( 85.57499999726880446, 164.1591823560292198, -12.60653300113719766 ) ) ;
#24778 = CARTESIAN_POINT ( 'NONE',  ( -9.680171189290831535, 214.0920067884431148, 87.80113791807858092 ) ) ;
#24779 = ADVANCED_FACE ( 'NONE', ( #1037 ), #8210, .F. ) ;
#24780 = ADVANCED_FACE ( 'NONE', ( #18763 ), #19089, .F. ) ;
#24781 = CARTESIAN_POINT ( 'NONE',  ( -10.01549611932653860, 203.7984951890123000, 102.3511379180785781 ) ) ;
#24782 = CARTESIAN_POINT ( 'NONE',  ( 52.88867513459483405, 159.8737954434939752, -14.99999999999974420 ) ) ;
#24783 = ORIENTED_EDGE ( 'NONE', *, *, #20863, .T. ) ;
#24784 = CARTESIAN_POINT ( 'NONE',  ( 11.98450388067341876, 210.9467285061363953, 69.84886208192143897 ) ) ;
#24785 = CARTESIAN_POINT ( 'NONE',  ( 3.044812012439969795, 216.5253028482143520, 81.39886208192145034 ) ) ;
#24786 = CARTESIAN_POINT ( 'NONE',  ( -3.662846001189865142, 195.5725841191952838, 10.89886208192143613 ) ) ;
#24787 = CARTESIAN_POINT ( 'NONE',  ( -7.500000000000000000, 4.330127018922191873, -7.422398894150032511 ) ) ;
#24788 = CARTESIAN_POINT ( 'NONE',  ( -8.062137200540920645, 212.9164362838581894, 24.80113791807857027 ) ) ;
#24789 = ADVANCED_FACE ( 'NONE', ( #8527 ), #10240, .T. ) ;
#24790 = CARTESIAN_POINT ( 'NONE',  ( -0.05014649552828403384, 217.5146222423826714, 87.24886208192143044 ) ) ;
#24791 = B_SPLINE_CURVE_WITH_KNOTS ( 'NONE', 3,
 ( #25664, #5387, #33675, #2677, #2332, #12720, #28395, #33501, #13057, #23447, #112, #10173, #10514, #23280, #279, #15772, #7952, #5053, #15444, #20894, #31291, #28728, #10674, #10349, #21053, #24266, #16099, #8441, #32109, #936, #29902, #3161, #14220, #774 ),
 .UNSPECIFIED., .F., .F.,
 ( 4, 2, 2, 2, 2, 2, 2, 2, 2, 2, 2, 2, 2, 2, 2, 2, 4 ),
 ( 0.000000000000000000, 0.03125000000000000000, 0.06250000000000000000, 0.09375000000000000000, 0.1250000000000000000, 0.1562500000000000000, 0.1875000000000000000, 0.2187500000000000000, 0.2500000000000000000, 0.2812500000000000000, 0.3125000000000000000, 0.3437500000000000000, 0.3750000000000000000, 0.4062500000000000000, 0.4375000000000000000, 0.4687500000000000000, 0.5000000000000000000 ),
 .UNSPECIFIED. ) ;
#24792 = CARTESIAN_POINT ( 'NONE',  ( -7.922281120364393914, 4.573931137438271399, -8.047472243342930653 ) ) ;
#24793 = VERTEX_POINT ( 'NONE', #695 ) ;
#24794 = DIRECTION ( 'NONE',  ( 0.1045284632676470454, 0.000000000000000000, -0.9945218953682739560 ) ) ;
#24795 = CARTESIAN_POINT ( 'NONE',  ( -4.903702542908436435, 200.1653181626580249, 68.04886208192144181 ) ) ;
#24796 = ADVANCED_FACE ( 'NONE', ( #13636 ), #29318, .F. ) ;
#24797 = VERTEX_POINT ( 'NONE', #26749 ) ;
#24798 = CARTESIAN_POINT ( 'NONE',  ( 86.22499999726882436, 149.9369285172503510, 15.58253174999999580 ) ) ;
#24799 = ORIENTED_EDGE ( 'NONE', *, *, #29161, .F. ) ;
#24800 = CARTESIAN_POINT ( 'NONE',  ( 69.01132485994283172, 142.2402378747194405, 9.270509831248432420 ) ) ;
#24801 = CARTESIAN_POINT ( 'NONE',  ( 73.72499999726881015, 169.8198683612136222, 4.815267126137181997 ) ) ;
#24802 = CYLINDRICAL_SURFACE ( 'NONE', #16484, 15.00000000000001776 ) ;
#24803 = CARTESIAN_POINT ( 'NONE',  ( -7.984503880673488041, 209.6470497212046098, 72.65113791807856103 ) ) ;
#24804 = DIRECTION ( 'NONE',  ( -0.000000000000000000, -0.000000000000000000, -1.000000000000000000 ) ) ;
#24805 = CARTESIAN_POINT ( 'NONE',  ( 41.30000000000000426, 163.5228861582408797, 11.73074641843673049 ) ) ;
#24806 = CARTESIAN_POINT ( 'NONE',  ( 6.444103211790928043, 211.7408657792734061, 51.69886208192144039 ) ) ;
#24807 = DIRECTION ( 'NONE',  ( 1.000000000000000000, 0.000000000000000000, 0.000000000000000000 ) ) ;
#24808 = DIRECTION ( 'NONE',  ( -0.8191520442889912434, 0.000000000000000000, -0.5735764363510469366 ) ) ;
#24809 = CARTESIAN_POINT ( 'NONE',  ( 32.50000000000000000, 155.0000000000000000, 15.00000000000001243 ) ) ;
#24810 = CARTESIAN_POINT ( 'NONE',  ( 53.92499999726881299, 164.1591823560292198, 12.60653300113718167 ) ) ;
#24811 = CARTESIAN_POINT ( 'NONE',  ( -0.05014649552807705357, 194.3824533091408000, 56.75113791807857666 ) ) ;
#24812 = CARTESIAN_POINT ( 'NONE',  ( -126.3741763928862269, -5.113356552508659725, 35.00001199999999812 ) ) ;
#24813 = CARTESIAN_POINT ( 'NONE',  ( 7.456977232089302632, 217.1783343296989131, 1.551137918078565603 ) ) ;
#24814 = CARTESIAN_POINT ( 'NONE',  ( -8.062137200540920645, 212.9164362838581894, 78.80113791807858092 ) ) ;
#24815 = CARTESIAN_POINT ( 'NONE',  ( -0.05014649552828442242, 219.6175466908591716, 39.24886208192143755 ) ) ;
#24816 = CARTESIAN_POINT ( 'NONE',  ( 6.220909254589680693, 198.5229672870052582, 52.44886208192143329 ) ) ;
#24817 = CARTESIAN_POINT ( 'NONE',  ( 84.59999999453762598, 168.7903194862797420, 4.480746418436729606 ) ) ;
#24818 = CARTESIAN_POINT ( 'NONE',  ( -11.98450388067348804, 210.9467285061362247, 90.65113791807857524 ) ) ;
#24819 = CARTESIAN_POINT ( 'NONE',  ( 2.517493886308900919, 214.5937144450984420, 94.40113791807857524 ) ) ;
#24820 =( BOUNDED_CURVE ( )  B_SPLINE_CURVE ( 2, ( #11962, #19962, #22526, #32569, #25075, #12130, #11788, #16897, #22181, #14683, #1570 ),
 .UNSPECIFIED., .F., .F. ) 
 B_SPLINE_CURVE_WITH_KNOTS ( ( 3, 2, 2, 2, 2, 3 ),
 ( 0.5714285714285712858, 0.5749999999999998446, 0.5785714285714285143, 0.5821428571428569620, 0.5857142857142855208, 0.5892857142857140795 ),
 .UNSPECIFIED. ) 
 CURVE ( )  GEOMETRIC_REPRESENTATION_ITEM ( )  RATIONAL_B_SPLINE_CURVE ( ( 1.000000000000001554, 0.9510565162951518658, 1.000000000000000000, 0.9510565162951534202, 1.000000000000000000, 0.9510565162951534202, 1.000000000000000000, 0.9510565162951534202, 1.000000000000000000, 0.9510565162951564178, 0.9999999999999970024 ) ) 
 REPRESENTATION_ITEM ( '' )  );
#24821 = CARTESIAN_POINT ( 'NONE',  ( -10.01549611932659722, 210.2015048109875011, 62.64886208192143613 ) ) ;
#24822 = CARTESIAN_POINT ( 'NONE',  ( -6.127431526422343306E-17, 9.147862274876549904, -8.047472243342932430 ) ) ;
#24823 = EDGE_LOOP ( 'NONE', ( #19340, #22045, #5106, #17885 ) ) ;
#24824 = CARTESIAN_POINT ( 'NONE',  ( 9.680171189290716072, 214.0920067884432854, 72.69886208192143329 ) ) ;
#24825 = ORIENTED_EDGE ( 'NONE', *, *, #115, .F. ) ;
#24826 = CARTESIAN_POINT ( 'NONE',  ( 69.77499999726880731, 169.8198683612136222, -4.815267126137197984 ) ) ;
#24827 = CARTESIAN_POINT ( 'NONE',  ( 4.984841277089891776, 200.2242689037093726, 43.44886208192144039 ) ) ;
#24828 = EDGE_LOOP ( 'NONE', ( #5263, #28700 ) ) ;
#24829 = AXIS2_PLACEMENT_3D ( 'NONE', #1912, #6337, #32912 ) ;
#24830 = CARTESIAN_POINT ( 'NONE',  ( 84.47499999726883857, 149.9369285172503510, 15.58253174999999580 ) ) ;
#24831 = FACE_BOUND ( 'NONE', #22781, .T. ) ;
#24832 = CARTESIAN_POINT ( 'NONE',  ( -4.555094537983154446, -5.243183837310248840, -6.208110906918257399 ) ) ;
#24833 = CARTESIAN_POINT ( 'NONE',  ( 0.05014649552807626948, 215.4116977939061144, 61.25113791807857666 ) ) ;
#24834 = DIRECTION ( 'NONE',  ( -1.000000000000000000, 0.000000000000000000, 0.000000000000000000 ) ) ;
#24835 = CARTESIAN_POINT ( 'NONE',  ( 8.118202686958138514, 201.1607312380088501, 43.29886208192143471 ) ) ;
#24836 = ORIENTED_EDGE ( 'NONE', *, *, #6032, .F. ) ;
#24837 = CIRCLE ( 'NONE', #28667, 5.400000000000002132 ) ;
#24838 = FACE_BOUND ( 'NONE', #26834, .T. ) ;
#24839 = LINE ( 'NONE', #15879, #5265 ) ;
#24840 = DIRECTION ( 'NONE',  ( 0.000000000000000000, 0.000000000000000000, -1.000000000000000000 ) ) ;
#24841 = CARTESIAN_POINT ( 'NONE',  ( -4.903702542908436435, 200.1653181626580249, 26.04886208192144181 ) ) ;
#24842 = CARTESIAN_POINT ( 'NONE',  ( -10.01549611932653860, 203.7984951890123284, 60.35113791807857808 ) ) ;
#24843 = CARTESIAN_POINT ( 'NONE',  ( -8.118202686958039038, 201.1607312380087080, 42.20113791807857240 ) ) ;
#24844 = CARTESIAN_POINT ( 'NONE',  ( 71.31132485994280046, 140.7341522555726669, -4.635254915624220651 ) ) ;
#24845 = ITEM_DEFINED_TRANSFORMATION ( 'NONE', 'NONE', #30066,  #2404 ) ;
#24846 = CARTESIAN_POINT ( 'NONE',  ( -0.05014649552810635652, 196.4853777576173002, 17.75113791807856245 ) ) ;
#24847 = CARTESIAN_POINT ( 'NONE',  ( 0.05014649552828262524, 198.5883022060938572, 97.74886208192141623 ) ) ;
#24848 = CARTESIAN_POINT ( 'NONE',  ( 42.12499999726881583, 155.0000000000000000, 15.58253174999999402 ) ) ;
#24849 =( LENGTH_UNIT ( ) NAMED_UNIT ( * ) SI_UNIT ( .MILLI., .METRE. ) );
#24850 = CARTESIAN_POINT ( 'NONE',  ( 87.50000000000000000, 158.3354728270139447, -15.12515773927365181 ) ) ;
#24851 = CARTESIAN_POINT ( 'NONE',  ( -7.375838497908182134, 217.2372850707499765, 27.95113791807857240 ) ) ;
#24852 = DIRECTION ( 'NONE',  ( -1.000000000000000000, 0.000000000000000000, 0.000000000000000000 ) ) ;
#24853 = CARTESIAN_POINT ( 'NONE',  ( -8.062137200540920645, 212.9164362838581894, 78.80113791807858092 ) ) ;
#24854 = CARTESIAN_POINT ( 'NONE',  ( -0.05014649552810635652, 196.4853777576173002, 47.75113791807856245 ) ) ;
#24855 = DIRECTION ( 'NONE',  ( 0.000000000000000000, 0.000000000000000000, -1.000000000000000000 ) ) ;
#24856 = AXIS2_PLACEMENT_3D ( 'NONE', #29829, #31867, #8531 ) ;
#24857 = DIRECTION ( 'NONE',  ( -6.106226635438360972E-16, 0.04769215134144213358, -0.9988620819214358848 ) ) ;
#24858 = CARTESIAN_POINT ( 'NONE',  ( 12.01549611932659367, 203.1486557965466773, 1.148862081921433909 ) ) ;
#24859 = CARTESIAN_POINT ( 'NONE',  ( -10.01549611932659545, 210.2015048109875011, 23.64886208192143613 ) ) ;
#24860 = CARTESIAN_POINT ( 'NONE',  ( 69.09999999453764019, 150.2886644046228639, 14.49999999999999645 ) ) ;
#24861 = ORIENTED_EDGE ( 'NONE', *, *, #814, .F. ) ;
#24862 = CARTESIAN_POINT ( 'NONE',  ( -12.01549611932652972, 203.1486557965464499, 60.35113791807857098 ) ) ;
#24863 = CARTESIAN_POINT ( 'NONE',  ( 4.984841277089725686, 213.7757310962907411, 67.55113791807856671 ) ) ;
#24864 = CARTESIAN_POINT ( 'NONE',  ( -10.00000000000000711, 206.9523078486584495, 35.49886208192143044 ) ) ;
#24865 = VECTOR ( 'NONE', #16838, 1000.000000000000000 ) ;
#24866 = EDGE_LOOP ( 'NONE', ( #1700, #20471, #29911, #11175, #5669, #6951, #32444 ) ) ;
#24867 = CARTESIAN_POINT ( 'NONE',  ( 8.118202686958039038, 212.8392687619912635, 85.70113791807858661 ) ) ;
#24868 = ORIENTED_EDGE ( 'NONE', *, *, #32456, .T. ) ;
#24869 = EDGE_CURVE ( 'NONE', #8405, #14565, #24538, .T. ) ;
#24870 = CARTESIAN_POINT ( 'NONE',  ( -125.0000000000000000, 25.00000000000000000, 20.00000000000000000 ) ) ;
#24871 = LINE ( 'NONE', #30159, #23083 ) ;
#24872 = VERTEX_POINT ( 'NONE', #16694 ) ;
#24873 = CARTESIAN_POINT ( 'NONE',  ( 4.903702542908601636, 200.1653181626581102, 29.45113791807856529 ) ) ;
#24874 = CIRCLE ( 'NONE', #9088, 24.99999999999999289 ) ;
#24875 = VECTOR ( 'NONE', #32988, 1000.000000000000000 ) ;
#24876 = CARTESIAN_POINT ( 'NONE',  ( 3.135527875058981895, 197.5041725223112792, 13.59886208192143719 ) ) ;
#24877 = CARTESIAN_POINT ( 'NONE',  ( 49.77499999726880731, 169.8198683612136222, -4.815267126137197984 ) ) ;
#24878 = ORIENTED_EDGE ( 'NONE', *, *, #31264, .T. ) ;
#24879 = CARTESIAN_POINT ( 'NONE',  ( -7.984503880673488041, 209.6470497212046098, 51.65113791807857524 ) ) ;
#24880 = DIRECTION ( 'NONE',  ( -0.1045284632676468234, 0.000000000000000000, 0.9945218953682740670 ) ) ;
#24881 = AXIS2_PLACEMENT_3D ( 'NONE', #17677, #2349, #33353 ) ;
#24882 = VECTOR ( 'NONE', #65, 1000.000000000000000 ) ;
#24883 =( NAMED_UNIT ( * ) PLANE_ANGLE_UNIT ( ) SI_UNIT ( $, .RADIAN. ) );
#24884 = DIRECTION ( 'NONE',  ( 1.000000000000000000, 0.000000000000000000, 0.000000000000000000 ) ) ;
#24885 = CARTESIAN_POINT ( 'NONE',  ( 8.062137200540822946, 212.9164362838583315, 87.69886208192144750 ) ) ;
#24886 = CARTESIAN_POINT ( 'NONE',  ( 60.07499999726879736, 168.2552932293087906, 9.630534252274372875 ) ) ;
#24887 = CARTESIAN_POINT ( 'NONE',  ( -8.062137200540920645, 212.9164362838581894, 30.80113791807856671 ) ) ;
#24888 = CYLINDRICAL_SURFACE ( 'NONE', #14346, 2.149999999999984812 ) ;
#24889 = CARTESIAN_POINT ( 'NONE',  ( -8.062137200540920645, 212.9164362838581894, 21.80113791807856671 ) ) ;
#24890 = VECTOR ( 'NONE', #19656, 1000.000000000000000 ) ;
#24891 = DIRECTION ( 'NONE',  ( 0.000000000000000000, -0.7071067811865389130, 0.7071067811865561215 ) ) ;
#24892 = CARTESIAN_POINT ( 'NONE',  ( 77.89999999999999147, 141.2096805137202580, 4.480746418436733158 ) ) ;
#24893 =( NAMED_UNIT ( * ) PLANE_ANGLE_UNIT ( ) SI_UNIT ( $, .RADIAN. ) );
#24894 = CARTESIAN_POINT ( 'NONE',  ( 125.5000000000000000, 81.56696077377769427, 76.47359838532574372 ) ) ;
#24895 = CARTESIAN_POINT ( 'NONE',  ( 6.139770520408368348, 198.4640165459539674, 92.45113791807857240 ) ) ;
#24896 = CARTESIAN_POINT ( 'NONE',  ( 4.000000000000000000, 0.000000000000000000, 0.000000000000000000 ) ) ;
#24897 = CARTESIAN_POINT ( 'NONE',  ( 47.47499999726881015, 160.0630714827496206, -15.58253175000000823 ) ) ;
#24898 = CARTESIAN_POINT ( 'NONE',  ( -9.984503880673473830, 210.2968891136704315, 42.65113791807856813 ) ) ;
#24899 = CARTESIAN_POINT ( 'NONE',  ( 86.02499999726880731, 160.0630714827496206, 15.58253174999999402 ) ) ;
#24900 = CARTESIAN_POINT ( 'NONE',  ( -64.96121601855533356, -1.809269760319439646, -19.53878398144470907 ) ) ;
#24901 = DIRECTION ( 'NONE',  ( 1.000000000000000000, 0.000000000000000000, 0.000000000000000000 ) ) ;
#24902 = CARTESIAN_POINT ( 'NONE',  ( 44.79999999453762882, 163.5228861582408797, 11.73074641843673049 ) ) ;
#24903 = ORIENTED_EDGE ( 'NONE', *, *, #13066, .T. ) ;
#24904 = CARTESIAN_POINT ( 'NONE',  ( 7.375838497908181246, 196.7627149292499666, 17.45113791807856174 ) ) ;
#24905 = AXIS2_PLACEMENT_3D ( 'NONE', #15625, #26027, #2699 ) ;
#24906 = PLANE ( 'NONE',  #22493 ) ;
#24907 = AXIS2_PLACEMENT_3D ( 'NONE', #19259, #8375, #31863 ) ;
#24908 = CARTESIAN_POINT ( 'NONE',  ( -54.79999999999999716, -6.711064459327494323E-15, -20.00000000000001776 ) ) ;
#24909 = ORIENTED_EDGE ( 'NONE', *, *, #31152, .T. ) ;
#24910 = AXIS2_PLACEMENT_3D ( 'NONE', #23463, #22957, #9847 ) ;
#24911 = CARTESIAN_POINT ( 'NONE',  ( 3.753561863808876797, 195.6020594897209719, 43.59886208192143897 ) ) ;
#24912 = CARTESIAN_POINT ( 'NONE',  ( -3.135527875058821579, 197.5041725223112223, -0.09886208192143428053 ) ) ;
#24913 = CARTESIAN_POINT ( 'NONE',  ( -6.220909254589537696, 198.5229672870051161, 63.05113791807858092 ) ) ;
#24914 = CARTESIAN_POINT ( 'NONE',  ( -8.000000000000008882, 206.9523078486584780, 26.49886208192143400 ) ) ;
#24915 = EDGE_CURVE ( 'NONE', #2597, #32104, #864, .T. ) ;
#24916 = VECTOR ( 'NONE', #14339, 1000.000000000000000 ) ;
#24917 = DIRECTION ( 'NONE',  ( 1.000000000000000000, 0.000000000000000000, 0.000000000000000000 ) ) ;
#24918 = ORIENTED_EDGE ( 'NONE', *, *, #26611, .T. ) ;
#24919 = CARTESIAN_POINT ( 'NONE',  ( -6.500168698208244500, 211.6636982574061676, 98.79886208192142760 ) ) ;
#24920 = EDGE_CURVE ( 'NONE', #18184, #4076, #29477, .T. ) ;
#24921 = DIRECTION ( 'NONE',  ( 1.000000000000000000, 0.000000000000000000, 0.000000000000000000 ) ) ;
#24922 = CARTESIAN_POINT ( 'NONE',  ( 2.426778023690261410, 199.3768101843759837, 38.60113791807857098 ) ) ;
#24923 = CARTESIAN_POINT ( 'NONE',  ( 9.379977934355910207, 208.8253170565643870, -1.014254689207407356 ) ) ;
#24924 = ORIENTED_EDGE ( 'NONE', *, *, #12870, .F. ) ;
#24925 = CARTESIAN_POINT ( 'NONE',  ( 35.22499999726881015, 160.0630714827496206, -15.58253175000000823 ) ) ;
#24926 = CARTESIAN_POINT ( 'NONE',  ( 40.71132485994280614, 155.0000000000000000, 15.00000000000001243 ) ) ;
#24927 = EDGE_CURVE ( 'NONE', #19762, #9319, #28440, .T. ) ;
#24928 = CARTESIAN_POINT ( 'NONE',  ( -10.01549611932653860, 203.7984951890123284, 3.351137918078566091 ) ) ;
#24929 = CARTESIAN_POINT ( 'NONE',  ( -9.984503880673420539, 203.7031108863293980, 62.34886208192143897 ) ) ;
#24930 = CARTESIAN_POINT ( 'NONE',  ( 37.87499999726880873, 171.3844434931184253, -7.942151717890132712E-15 ) ) ;
#24931 = CYLINDRICAL_SURFACE ( 'NONE', #503, 15.00000000000001776 ) ;
#24932 = CARTESIAN_POINT ( 'NONE',  ( 9.984503880673470277, 203.7031108863295401, -0.8488620819214341973 ) ) ;
#24933 = PRODUCT_DEFINITION_SHAPE ( 'NONE', 'NONE',  #17286 ) ;
#24934 = CARTESIAN_POINT ( 'NONE',  ( -16.08713178458081217, -22.46635493911272619, -0.07154745401829776252 ) ) ;
#24935 = CONICAL_SURFACE ( 'NONE', #33105, 12.00000000000001066, 0.1047197551196464710 ) ;
#24936 = CARTESIAN_POINT ( 'NONE',  ( 60.50000000000000000, 155.0000000000000000, -14.50000000000000711 ) ) ;
#24937 = CARTESIAN_POINT ( 'NONE',  ( -27.49999999999999289, -14.58598892539970215, -2.083479913523507587 ) ) ;
#24938 = CARTESIAN_POINT ( 'NONE',  ( -8.015496119326597224, 209.5516654185217362, 80.64886208192145034 ) ) ;
#24939 = CARTESIAN_POINT ( 'NONE',  ( 42.49999999999999289, -72.99999999999998579, 20.00000000000000000 ) ) ;
#24940 = CARTESIAN_POINT ( 'NONE',  ( 107.5000000000000000, 155.0000000000000000, -6.938893903907228378E-15 ) ) ;
#24941 = EDGE_CURVE ( 'NONE', #8938, #16276, #2625, .T. ) ;
#24942 = CARTESIAN_POINT ( 'NONE',  ( 65.12499999726881583, 155.0000000000000000, -15.58253175000000823 ) ) ;
#24944 = ORIENTED_EDGE ( 'NONE', *, *, #31847, .T. ) ;
#24943 = CARTESIAN_POINT ( 'NONE',  ( 6.220909254589536808, 215.4770327129947987, 16.55113791807857027 ) ) ;
#24945 = CARTESIAN_POINT ( 'NONE',  ( 107.5000000000000000, 155.0000000000000000, -70.00000000000000000 ) ) ;
#24946 = CARTESIAN_POINT ( 'NONE',  ( 84.67499999726881299, 141.7447067706911810, 9.630534252274376428 ) ) ;
#24947 = CARTESIAN_POINT ( 'NONE',  ( 0.05014649552807549926, 219.6175466908591716, 91.25113791807856956 ) ) ;
#24948 = EDGE_CURVE ( 'NONE', #3951, #28893, #6989, .T. ) ;
#24949 = CARTESIAN_POINT ( 'NONE',  ( -9.998182820724316855, 207.4287148614901071, 102.5187279279133037 ) ) ;
#24950 = ORIENTED_EDGE ( 'NONE', *, *, #757, .T. ) ;
#24951 = CARTESIAN_POINT ( 'NONE',  ( 0.05014649552828288198, 194.3824533091408000, 73.74886208192144466 ) ) ;
#24952 = CARTESIAN_POINT ( 'NONE',  ( -6.139770520408224463, 198.4640165459539105, 80.04886208192142760 ) ) ;
#24953 = CARTESIAN_POINT ( 'NONE',  ( -3.662846001189865142, 195.5725841191952838, 16.89886208192143613 ) ) ;
#24954 = DIRECTION ( 'NONE',  ( 0.000000000000000000, 0.4999999999999993339, -0.8660254037844389297 ) ) ;
#24955 = VECTOR ( 'NONE', #24982, 1000.000000000000000 ) ;
#24956 = CARTESIAN_POINT ( 'NONE',  ( 0.05014649552810505201, 217.5146222423826714, 34.25113791807856956 ) ) ;
#24957 = B_SPLINE_CURVE_WITH_KNOTS ( 'NONE', 3,
 ( #28809, #19075, #850, #29464, #23690, #13134, #21466, #18749, #26567 ),
 .UNSPECIFIED., .F., .F.,
 ( 4, 2, 1, 2, 4 ),
 ( 0.000000000000000000, 0.002165063509461097498, 0.004330127018922194995, 0.006495190528383292493, 0.008660254037844389990 ),
 .UNSPECIFIED. ) ;
#24958 = CARTESIAN_POINT ( 'NONE',  ( 66.48867513459482836, 142.2402378747194405, -9.270509831248439525 ) ) ;
#24959 = CARTESIAN_POINT ( 'NONE',  ( -8.062137200540822946, 201.0835637161416400, 89.19886208192144750 ) ) ;
#24960 = CIRCLE ( 'NONE', #3186, 3.499999999999999556 ) ;
#24961 = CIRCLE ( 'NONE', #10296, 5.249999999999991118 ) ;
#24962 = CARTESIAN_POINT ( 'NONE',  ( -0.2813450144774468642, 7.667988119308851047, -6.122077150241852728 ) ) ;
#24963 = ORIENTED_EDGE ( 'NONE', *, *, #11562, .F. ) ;
#24964 = CARTESIAN_POINT ( 'NONE',  ( -3.755786496842903988E-16, -7.505553499465146494, -6.064240316920404439 ) ) ;
#24965 = CARTESIAN_POINT ( 'NONE',  ( 6.444103211790928043, 211.7408657792734061, 72.69886208192143329 ) ) ;
#24966 = ORIENTED_EDGE ( 'NONE', *, *, #20611, .T. ) ;
#24967 = AXIS2_PLACEMENT_3D ( 'NONE', #14841, #25239, #22683 ) ;
#24968 = CARTESIAN_POINT ( 'NONE',  ( 87.32499999726880446, 164.1591823560292198, -12.60653300113719766 ) ) ;
#24969 = VERTEX_POINT ( 'NONE', #25207 ) ;
#24970 = DIRECTION ( 'NONE',  ( 1.000000000000000000, -0.000000000000000000, -0.000000000000000000 ) ) ;
#24971 = CARTESIAN_POINT ( 'NONE',  ( 74.02499999726879309, 160.0630714827496206, 15.58253174999999402 ) ) ;
#24972 = CARTESIAN_POINT ( 'NONE',  ( -7.499999999999998224, 1.489914625143999416, -0.1187923833806747292 ) ) ;
#24973 = CARTESIAN_POINT ( 'NONE',  ( 6.500168698208129925, 211.6636982574063381, 79.70113791807857240 ) ) ;
#24974 = ADVANCED_FACE ( 'NONE', ( #12093 ), #1874, .T. ) ;
#24975 = CARTESIAN_POINT ( 'NONE',  ( 75.08867513459483689, 167.7597621252805880, -9.270509831248443078 ) ) ;
#24976 = CARTESIAN_POINT ( 'NONE',  ( 40.70000000000000284, 163.5228861582408797, -11.73074641843674470 ) ) ;
#24977 = CARTESIAN_POINT ( 'NONE',  ( 6.444103211790928043, 211.7408657792734061, 54.69886208192144039 ) ) ;
#24978 = CIRCLE ( 'NONE', #29331, 10.62447292484156947 ) ;
#24979 = EDGE_CURVE ( 'NONE', #9541, #31511, #4122, .T. ) ;
#24980 = AXIS2_PLACEMENT_3D ( 'NONE', #23834, #30850, #7680 ) ;
#24981 = CARTESIAN_POINT ( 'NONE',  ( 32.50000000000000000, 155.0000000000000000, 15.00000000000001243 ) ) ;
#24982 = DIRECTION ( 'NONE',  ( 1.000000000000000000, 0.000000000000000000, 0.000000000000000000 ) ) ;
#24983 = CARTESIAN_POINT ( 'NONE',  ( 27.50000000000000355, 2.688867821578065698, -17.94295719123739730 ) ) ;
#24984 = CARTESIAN_POINT ( 'NONE',  ( 51.82499999726881157, 168.2552932293087906, 9.630534252274372875 ) ) ;
#24985 = CARTESIAN_POINT ( 'NONE',  ( 62.27499999726880020, 160.0630714827496206, 15.58253174999999402 ) ) ;
#24986 = CARTESIAN_POINT ( 'NONE',  ( 12.01549611932652972, 210.8513442034534933, 58.85113791807857098 ) ) ;
#24987 = LINE ( 'NONE', #16967, #4262 ) ;
#24988 = ADVANCED_FACE ( 'NONE', ( #14309 ), #25467, .T. ) ;
#24989 = CARTESIAN_POINT ( 'NONE',  ( 0.05014649552807549926, 219.6175466908591716, 1.251137918078565558 ) ) ;
#24990 = CARTESIAN_POINT ( 'NONE',  ( 8.062137200540920645, 201.0835637161417822, 77.30113791807858092 ) ) ;
#24991 = CARTESIAN_POINT ( 'NONE',  ( 0.05014649552828288198, 194.3824533091408000, 43.74886208192143755 ) ) ;
#24992 = CARTESIAN_POINT ( 'NONE',  ( 3.044812012439969795, 216.5253028482143520, 45.39886208192143613 ) ) ;
#24993 = CARTESIAN_POINT ( 'NONE',  ( 2.000000000000000000, 1.773042676681340968, -2.276824562219559311E-15 ) ) ;
#24994 = CARTESIAN_POINT ( 'NONE',  ( 3.753561863808689836, 218.3979405102790565, 91.40113791807857524 ) ) ;
#24995 = CARTESIAN_POINT ( 'NONE',  ( 10.01549611932653860, 210.2015048109876716, 1.851137918078565203 ) ) ;
#24996 = CARTESIAN_POINT ( 'NONE',  ( 0.05014649552828275708, 196.4853777576173002, 55.74886208192143755 ) ) ;
#24997 = VERTEX_POINT ( 'NONE', #17540 ) ;
#24998 = CARTESIAN_POINT ( 'NONE',  ( -9.680171189290716072, 199.9079932115567146, 71.19886208192144750 ) ) ;
#24999 = VERTEX_POINT ( 'NONE', #22314 ) ;
#25000 = CARTESIAN_POINT ( 'NONE',  ( 70.37499999726881583, 155.0000000000000000, 15.58253174999999402 ) ) ;
#25001 = CARTESIAN_POINT ( 'NONE',  ( 8.000000000000008882, 207.0476921513415220, 42.99886208192143755 ) ) ;
#25002 = CIRCLE ( 'NONE', #27165, 24.99999999999999289 ) ;
#25003 = ORIENTED_EDGE ( 'NONE', *, *, #25333, .T. ) ;
#25004 = CARTESIAN_POINT ( 'NONE',  ( 85.77499999726880731, 169.8198683612136222, -4.815267126137197984 ) ) ;
#25005 = FACE_BOUND ( 'NONE', #29606, .T. ) ;
#25006 = CARTESIAN_POINT ( 'NONE',  ( 16.00000000000000000, 0.000000000000000000, 0.000000000000000000 ) ) ;
#25007 = CARTESIAN_POINT ( 'NONE',  ( 2.426778023690261410, 199.3768101843759837, 62.60113791807857808 ) ) ;
#25008 = DIRECTION ( 'NONE',  ( -0.000000000000000000, -0.000000000000000000, 1.000000000000000000 ) ) ;
#25009 = EDGE_CURVE ( 'NONE', #20526, #3157, #8072, .T. ) ;
#25010 = CARTESIAN_POINT ( 'NONE',  ( -6.139770520408224463, 198.4640165459539389, 44.04886208192143471 ) ) ;
#25011 = VERTEX_POINT ( 'NONE', #6814 ) ;
#25012 = FACE_OUTER_BOUND ( 'NONE', #16977, .T. ) ;
#25013 = DIRECTION ( 'NONE',  ( -0.8191520442889912434, 1.003171929053524007E-16, 0.5735764363510469366 ) ) ;
#25014 = DIRECTION ( 'NONE',  ( -0.000000000000000000, 0.8660254037844390407, 0.4999999999999993894 ) ) ;
#25015 = CARTESIAN_POINT ( 'NONE',  ( 8.015496119326595448, 204.4483345814782638, 25.14886208192143258 ) ) ;
#25016 = CARTESIAN_POINT ( 'NONE',  ( 8.118202686958039038, 212.8392687619912635, 61.70113791807857240 ) ) ;
#25017 = EDGE_CURVE ( 'NONE', #22659, #18140, #11589, .T. ) ;
#25018 = CARTESIAN_POINT ( 'NONE',  ( -9.984503880673473830, 210.2968891136704315, 42.65113791807856813 ) ) ;
#25019 = CARTESIAN_POINT ( 'NONE',  ( 67.18867513459483121, 169.2658477444273331, -4.635254915624224203 ) ) ;
#25020 = CONTEXT_DEPENDENT_SHAPE_REPRESENTATION ( #4192, #8450 ) ;
#25021 = CARTESIAN_POINT ( 'NONE',  ( 6.139770520408368348, 198.4640165459539674, 20.45113791807855819 ) ) ;
#25022 = CARTESIAN_POINT ( 'NONE',  ( -2.426778023690262742, 214.6231898156240163, 10.10113791807856742 ) ) ;
#25023 = CARTESIAN_POINT ( 'NONE',  ( 43.32499999726881157, 164.1591823560292198, -12.60653300113719766 ) ) ;
#25024 = CARTESIAN_POINT ( 'NONE',  ( 117.5000000000000000, 54.13214199290997897, 25.91453920131689515 ) ) ;
#25025 = CARTESIAN_POINT ( 'NONE',  ( 87.50000000000008527, 146.2573930672651841, -12.23674163361536316 ) ) ;
#25026 = CARTESIAN_POINT ( 'NONE',  ( 7.456977232089302632, 217.1783343296989131, 25.55113791807857027 ) ) ;
#25027 = LINE ( 'NONE', #30302, #6973 ) ;
#25028 =( BOUNDED_SURFACE ( )  B_SPLINE_SURFACE ( 3, 2, ( 
 ( #8796, #23971, #19193 ),
 ( #8467, #26688, #3191 ),
 ( #23644, #31640, #3349 ),
 ( #13580, #21572, #16629 ),
 ( #31485, #5577, #29590 ),
 ( #633, #6241, #11032 ) ),
 .UNSPECIFIED., .F., .F., .T. ) 
 B_SPLINE_SURFACE_WITH_KNOTS ( ( 4, 2, 4 ),
 ( 3, 3 ),
 ( 0.003190620565844218184, 0.007281897438794484971, 0.01137317431174475132 ),
 ( 0.000000000000000000, 1.000000000000000000 ),
 .UNSPECIFIED. ) 
 GEOMETRIC_REPRESENTATION_ITEM ( )  RATIONAL_B_SPLINE_SURFACE ( (
 ( 1.000000000000000000, 0.8047731410850399447, 1.000000000000000000),
 ( 1.000000000000000000, 0.8125552299156222347, 1.000000000000000000),
 ( 1.000000000000000000, 0.8191520442889872466, 1.000000000000000000),
 ( 1.000000000000000000, 0.8191520442889872466, 1.000000000000000000),
 ( 1.000000000000000000, 0.8125552299156223457, 1.000000000000000000),
 ( 1.000000000000000000, 0.8047731410850402778, 1.000000000000000000) ) ) 
 REPRESENTATION_ITEM ( '' )  SURFACE ( )  );
#25029 = CARTESIAN_POINT ( 'NONE',  ( -10.00000000000000711, 207.0476921513413515, 75.50113791807858377 ) ) ;
#25030 = CARTESIAN_POINT ( 'NONE',  ( -3.135527875058821579, 197.5041725223112223, 47.90113791807857524 ) ) ;
#25031 = CARTESIAN_POINT ( 'NONE',  ( 0.000000000000000000, 0.000000000000000000, -1.540456584061364431 ) ) ;
#25032 = LINE ( 'NONE', #1684, #21200 ) ;
#25033 = CARTESIAN_POINT ( 'NONE',  ( -3.662846001189865142, 195.5725841191952838, 13.89886208192143613 ) ) ;
#25034 = CARTESIAN_POINT ( 'NONE',  ( 3.135527875058981895, 197.5041725223112792, 16.59886208192143542 ) ) ;
#25035 = CARTESIAN_POINT ( 'NONE',  ( 64.99999999453761745, 155.0000000000000000, 14.49999999999999467 ) ) ;
#25036 = ORIENTED_EDGE ( 'NONE', *, *, #1000, .T. ) ;
#25037 = CARTESIAN_POINT ( 'NONE',  ( 7.456977232089302632, 217.1783343296989131, 61.55113791807858092 ) ) ;
#25038 = CARTESIAN_POINT ( 'NONE',  ( 0.05014649552807626948, 215.4116977939061144, 70.25113791807856956 ) ) ;
#25039 = CARTESIAN_POINT ( 'NONE',  ( -0.05014649552828403384, 217.5146222423826714, 27.24886208192142689 ) ) ;
#25040 = CARTESIAN_POINT ( 'NONE',  ( 4.366061277241453098, -4.984806845751389659, -0.09463688534107157768 ) ) ;
#25041 = VERTEX_POINT ( 'NONE', #12260 ) ;
#25042 = ORIENTED_EDGE ( 'NONE', *, *, #8713, .F. ) ;
#25043 = CARTESIAN_POINT ( 'NONE',  ( 9.984503880673470277, 203.7031108863295401, 92.15113791807856103 ) ) ;
#25044 = ORIENTED_EDGE ( 'NONE', *, *, #16055, .T. ) ;
#25045 = CARTESIAN_POINT ( 'NONE',  ( 87.50000000000000000, 166.7234620888311838, -10.31567525671095531 ) ) ;
#25046 = FACE_OUTER_BOUND ( 'NONE', #7464, .T. ) ;
#25047 = ORIENTED_EDGE ( 'NONE', *, *, #10771, .F. ) ;
#25048 = CARTESIAN_POINT ( 'NONE',  ( 6.500168698208129925, 211.6636982574063381, 31.70113791807857240 ) ) ;
#25049 = CARTESIAN_POINT ( 'NONE',  ( 85.51132485994281751, 146.1832212156128890, -12.13525491562423042 ) ) ;
#25050 = CARTESIAN_POINT ( 'NONE',  ( 6.220909254589681581, 198.5229672870052582, 16.44886208192143329 ) ) ;
#25051 = CARTESIAN_POINT ( 'NONE',  ( 55.47499999726881015, 160.0630714827496206, -15.58253175000000823 ) ) ;
#25052 = ORIENTED_EDGE ( 'NONE', *, *, #17424, .F. ) ;
#25053 = CARTESIAN_POINT ( 'NONE',  ( -4.984841277089726574, 200.2242689037092305, 51.05113791807858092 ) ) ;
#25054 = CARTESIAN_POINT ( 'NONE',  ( 97.20416941062678973, 155.0000000000000000, 32.00000000000000000 ) ) ;
#25055 = CARTESIAN_POINT ( 'NONE',  ( -6.139770520408224463, 198.4640165459539389, 104.0488620819214276 ) ) ;
#25056 = CARTESIAN_POINT ( 'NONE',  ( 67.37499999726881583, 155.0000000000000000, -15.58253175000000823 ) ) ;
#25057 = CARTESIAN_POINT ( 'NONE',  ( 0.05014649552810505201, 217.5146222423826714, 34.25113791807856956 ) ) ;
#25058 = CARTESIAN_POINT ( 'NONE',  ( 70.48867513459484258, 142.2402378747194405, -9.270509831248439525 ) ) ;
#25059 = CARTESIAN_POINT ( 'NONE',  ( 8.062137200540920645, 201.0835637161417822, 20.30113791807856671 ) ) ;
#25060 = DIRECTION ( 'NONE',  ( 0.000000000000000000, 1.000000000000000000, -3.491481338843133355E-15 ) ) ;
#25061 = TOROIDAL_SURFACE ( 'NONE', #31063, 69.99999999999998579, 30.00000000000000000 ) ;
#25062 = CARTESIAN_POINT ( 'NONE',  ( 78.00000000000000000, 139.7537977485451393, -4.138211985947621020E-15 ) ) ;
#25063 = DIRECTION ( 'NONE',  ( 0.01265860800194867734, -0.08535984102820122488, -0.9962697712884263090 ) ) ;
#25064 = CARTESIAN_POINT ( 'NONE',  ( 3.135527875058820690, 216.4958274776887492, 100.4011379180785752 ) ) ;
#25065 = DIRECTION ( 'NONE',  ( 0.000000000000000000, 0.000000000000000000, 1.000000000000000000 ) ) ;
#25066 = CARTESIAN_POINT ( 'NONE',  ( 41.57499999726881157, 164.1591823560292198, -12.60653300113719766 ) ) ;
#25067 = CARTESIAN_POINT ( 'NONE',  ( -6.220909254589537696, 198.5229672870051161, 48.05113791807858092 ) ) ;
#25068 = CARTESIAN_POINT ( 'NONE',  ( 82.22499999726882436, 149.9369285172503510, 15.58253174999999580 ) ) ;
#25069 = DIRECTION ( 'NONE',  ( 0.000000000000000000, 0.000000000000000000, 1.000000000000000000 ) ) ;
#25070 = FACE_OUTER_BOUND ( 'NONE', #1583, .T. ) ;
#25071 = CARTESIAN_POINT ( 'NONE',  ( 45.49999999453763166, 139.7537977485451393, -4.138211985947621020E-15 ) ) ;
#25072 = ORIENTED_EDGE ( 'NONE', *, *, #11562, .T. ) ;
#25073 = CARTESIAN_POINT ( 'NONE',  ( 9.736236675707914401, 214.0148392665762458, 28.70113791807857240 ) ) ;
#25074 = DIRECTION ( 'NONE',  ( 0.000000000000000000, 0.000000000000000000, 1.000000000000000000 ) ) ;
#25075 = CARTESIAN_POINT ( 'NONE',  ( 66.11132485994281183, 169.2658477444273331, -4.635254915624224203 ) ) ;
#25076 = VERTEX_POINT ( 'NONE', #14987 ) ;
#25077 = CARTESIAN_POINT ( 'NONE',  ( -6.220909254589537696, 198.5229672870051161, 0.05113791807856577637 ) ) ;
#25078 = CARTESIAN_POINT ( 'NONE',  ( 3.044812012440130555, 197.4746971517856764, 62.60113791807857098 ) ) ;
#25079 = CARTESIAN_POINT ( 'NONE',  ( 7.984503880673422316, 209.6470497212048372, 21.84886208192143542 ) ) ;
#25080 = DIRECTION ( 'NONE',  ( 0.000000000000000000, 0.000000000000000000, 1.000000000000000000 ) ) ;
#25081 = VERTEX_POINT ( 'NONE', #1192 ) ;
#25082 = CARTESIAN_POINT ( 'NONE',  ( -0.05014649552807731031, 198.5883022060938572, 2.751137918078566003 ) ) ;
#25083 = CARTESIAN_POINT ( 'NONE',  ( 32.50000000000000000, 155.0000000000000000, -6.938893903907228378E-15 ) ) ;
#25084 = CARTESIAN_POINT ( 'NONE',  ( 12.01549611932659367, 203.1486557965466773, 85.14886208192143613 ) ) ;
#25085 = CARTESIAN_POINT ( 'NONE',  ( 36.67499999726879878, 141.7447067706911810, 9.630534252274376428 ) ) ;
#25086 = ORIENTED_EDGE ( 'NONE', *, *, #31667, .T. ) ;
#25087 = CARTESIAN_POINT ( 'NONE',  ( 41.22499999726881015, 160.0630714827496206, -15.58253175000000823 ) ) ;
#25088 = FACE_OUTER_BOUND ( 'NONE', #10316, .T. ) ;
#25089 = CARTESIAN_POINT ( 'NONE',  ( 10.00000000000000711, 206.9523078486586201, -0.9988620819214343305 ) ) ;
#25090 = CARTESIAN_POINT ( 'NONE',  ( 10.01549611932659545, 203.7984951890123853, 76.14886208192143613 ) ) ;
#25091 = CARTESIAN_POINT ( 'NONE',  ( 39.57499999726881157, 164.1591823560292198, -12.60653300113719766 ) ) ;
#25092 = CARTESIAN_POINT ( 'NONE',  ( 105.0134430565187387, 155.0000000000000000, 31.00000000000000000 ) ) ;
#25093 = CARTESIAN_POINT ( 'NONE',  ( -3.044812012440131443, 216.5253028482142952, 7.101137918078566535 ) ) ;
#25094 = DIRECTION ( 'NONE',  ( 1.000000000000000000, 0.000000000000000000, 0.000000000000000000 ) ) ;
#25095 = CARTESIAN_POINT ( 'NONE',  ( 62.30000000000000426, 146.4771138417591203, -11.73074641843674470 ) ) ;
#25096 = CARTESIAN_POINT ( 'NONE',  ( 64.01132485994281751, 167.7597621252805880, -9.270509831248443078 ) ) ;
#25097 = CARTESIAN_POINT ( 'NONE',  ( 0.05014649552828262524, 198.5883022060938572, 79.74886208192143044 ) ) ;
#25098 = CYLINDRICAL_SURFACE ( 'NONE', #32489, 15.00000000000001776 ) ;
#25099 = CARTESIAN_POINT ( 'NONE',  ( -13.75000000000001954, 23.81569860407205752, 0.000000000000000000 ) ) ;
#25100 = CARTESIAN_POINT ( 'NONE',  ( 7.375838497908012492, 217.2372850707501186, 90.54886208192144181 ) ) ;
#25101 = EDGE_CURVE ( 'NONE', #15366, #15702, #19145, .T. ) ;
#25102 = CARTESIAN_POINT ( 'NONE',  ( 65.52499999726880731, 169.8198683612136222, -4.815267126137197984 ) ) ;
#25104 = VERTEX_POINT ( 'NONE', #4255 ) ;
#25103 = CARTESIAN_POINT ( 'NONE',  ( -9.984503880673475606, 210.2968891136704315, 18.65113791807856458 ) ) ;
#25105 = CIRCLE ( 'NONE', #17491, 2.149999999999974598 ) ;
#25106 = CARTESIAN_POINT ( 'NONE',  ( 80.57499999726880446, 145.8408176439707802, 12.60653300113718345 ) ) ;
#25107 = CARTESIAN_POINT ( 'NONE',  ( 9.680171189290831535, 199.9079932115568852, 83.30113791807858092 ) ) ;
#25108 = DIRECTION ( 'NONE',  ( 0.000000000000000000, 0.000000000000000000, -1.000000000000000000 ) ) ;
#25109 = ORIENTED_EDGE ( 'NONE', *, *, #27506, .T. ) ;
#25110 = CARTESIAN_POINT ( 'NONE',  ( 12.00000000000000711, 207.0476921513415220, 69.99886208192144466 ) ) ;
#25111 = CARTESIAN_POINT ( 'NONE',  ( 9.984503880673420539, 210.2968891136705736, 78.84886208192142476 ) ) ;
#25112 = CARTESIAN_POINT ( 'NONE',  ( 12.00000000000000711, 207.0476921513415220, 12.99886208192143400 ) ) ;
#25113 = DIRECTION ( 'NONE',  ( 0.000000000000000000, 0.000000000000000000, 1.000000000000000000 ) ) ;
#25114 = CARTESIAN_POINT ( 'NONE',  ( -3.135527875058821579, 197.5041725223112223, 32.90113791807857524 ) ) ;
#25115 = DIRECTION ( 'NONE',  ( -1.000000000000000000, 0.000000000000000000, 0.000000000000000000 ) ) ;
#25116 = CARTESIAN_POINT ( 'NONE',  ( -8.118202686958138514, 212.8392687619910930, 101.7988620819214418 ) ) ;
#25117 = CARTESIAN_POINT ( 'NONE',  ( 127.5000000000000000, 229.9533188057739039, -74.95331880577418815 ) ) ;
#25118 = VERTEX_POINT ( 'NONE', #14649 ) ;
#25119 = CARTESIAN_POINT ( 'NONE',  ( 99.30625411593993590, 155.0000000000000000, 0.000000000000000000 ) ) ;
#25120 = CARTESIAN_POINT ( 'NONE',  ( 7.984503880673422316, 209.6470497212048372, 78.84886208192143897 ) ) ;
#25121 = ORIENTED_EDGE ( 'NONE', *, *, #19289, .F. ) ;
#25122 = CARTESIAN_POINT ( 'NONE',  ( 84.92499999726882720, 145.8408176439707802, -12.60653300113719588 ) ) ;
#25123 = ORIENTED_EDGE ( 'NONE', *, *, #5370, .T. ) ;
#25124 = CARTESIAN_POINT ( 'NONE',  ( 69.41132485994282320, 142.2402378747194405, -9.270509831248439525 ) ) ;
#25125 = EDGE_CURVE ( 'NONE', #33036, #18870, #19482, .T. ) ;
#25126 = CARTESIAN_POINT ( 'NONE',  ( 74.52499999726880731, 140.1801316387863778, 4.815267126137185549 ) ) ;
#25127 = CYLINDRICAL_SURFACE ( 'NONE', #26825, 4.000000000000000000 ) ;
#25128 = CARTESIAN_POINT ( 'NONE',  ( -7.984503880673488041, 209.6470497212046098, 75.65113791807856103 ) ) ;
#25129 = CARTESIAN_POINT ( 'NONE',  ( 92.60208470531341618, 155.0000000000000000, -32.00000000000002842 ) ) ;
#25131 = VECTOR ( 'NONE', #19533, 1000.000000000000000 ) ;
#25130 =( NAMED_UNIT ( * ) SI_UNIT ( $, .STERADIAN. ) SOLID_ANGLE_UNIT ( ) );
#25132 = CARTESIAN_POINT ( 'NONE',  ( 43.39999999999999147, 159.7113355953771077, 14.49999999999999289 ) ) ;
#25133 = CARTESIAN_POINT ( 'NONE',  ( -2.517493886309087880, 214.5937144450984135, 57.09886208192145318 ) ) ;
#25134 = ADVANCED_FACE ( 'NONE', ( #25550 ), #31335, .T. ) ;
#25135 = B_SPLINE_CURVE_WITH_KNOTS ( 'NONE', 3,
 ( #22328, #19941, #4777, #33056, #22840, #20281 ),
 .UNSPECIFIED., .F., .F.,
 ( 4, 2, 4 ),
 ( 0.000000000000000000, 0.001990940508721414457, 0.003981881017442828914 ),
 .UNSPECIFIED. ) ;
#25136 = LINE ( 'NONE', #1800, #12132 ) ;
#25137 = CARTESIAN_POINT ( 'NONE',  ( 77.98867513459482836, 146.1832212156128890, 12.13525491562421976 ) ) ;
#25138 = CARTESIAN_POINT ( 'NONE',  ( 32.50000000000000000, 155.0000000000000000, 15.00000000000001243 ) ) ;
#25139 = CARTESIAN_POINT ( 'NONE',  ( 53.32499999726881157, 164.1591823560292198, -12.60653300113719766 ) ) ;
#25140 = CARTESIAN_POINT ( 'NONE',  ( 62.17499999726882010, 164.1591823560292198, 12.60653300113718167 ) ) ;
#25141 = CARTESIAN_POINT ( 'NONE',  ( 9.680171189290831535, 199.9079932115568852, 53.30113791807857382 ) ) ;
#25142 = CARTESIAN_POINT ( 'NONE',  ( -10.00000000000000711, 207.0476921513413515, 102.5011379180785838 ) ) ;
#25143 = CARTESIAN_POINT ( 'NONE',  ( 6.220909254589536808, 215.4770327129947987, 79.55113791807856671 ) ) ;
#25144 = EDGE_CURVE ( 'NONE', #24969, #2588, #16191, .T. ) ;
#25145 = CARTESIAN_POINT ( 'NONE',  ( 12.01549611932659367, 203.1486557965466773, 40.14886208192143613 ) ) ;
#25146 = CARTESIAN_POINT ( 'NONE',  ( 10.00000000000000711, 207.0476921513415220, 45.99886208192143755 ) ) ;
#25147 = CARTESIAN_POINT ( 'NONE',  ( -63.49999999999884892, 215.0000000000003979, 0.000000000000000000 ) ) ;
#25148 = CARTESIAN_POINT ( 'NONE',  ( -11.98450388067348804, 210.9467285061362247, 84.65113791807856103 ) ) ;
#25149 = CARTESIAN_POINT ( 'NONE',  ( 82.81132485994282888, 150.1262045565062806, 14.99999999999992006 ) ) ;
#25150 = CARTESIAN_POINT ( 'NONE',  ( -8.118202686958039038, 201.1607312380087080, 6.201137918078566180 ) ) ;
#25151 = CARTESIAN_POINT ( 'NONE',  ( -10.00000000000000711, 206.9523078486584495, 71.49886208192144466 ) ) ;
#25152 = CARTESIAN_POINT ( 'NONE',  ( 2.000000000000000888, 0.000000000000000000, -25.03750572909317285 ) ) ;
#25153 = EDGE_LOOP ( 'NONE', ( #10066, #14464, #17537 ) ) ;
#25154 = CARTESIAN_POINT ( 'NONE',  ( -12.01549611932659722, 210.8513442034533227, 74.64886208192143613 ) ) ;
#25155 = TOROIDAL_SURFACE ( 'NONE', #12105, 4.400000000000001243, 0.4000000000000000222 ) ;
#25156 = ORIENTED_EDGE ( 'NONE', *, *, #18714, .F. ) ;
#25157 = CARTESIAN_POINT ( 'NONE',  ( 80.57499999726880446, 145.8408176439707802, 12.60653300113718345 ) ) ;
#25158 = CARTESIAN_POINT ( 'NONE',  ( -8.000000000000008882, 206.9523078486584780, 41.49886208192143755 ) ) ;
#25159 = AXIS2_PLACEMENT_3D ( 'NONE', #29222, #16273, #31775 ) ;
#25160 = ORIENTED_EDGE ( 'NONE', *, *, #17671, .F. ) ;
#25161 = EDGE_CURVE ( 'NONE', #12632, #33078, #22992, .T. ) ;
#25162 = CARTESIAN_POINT ( 'NONE',  ( 84.07499999726879025, 168.2552932293087906, 9.630534252274372875 ) ) ;
#25163 = FACE_BOUND ( 'NONE', #13810, .T. ) ;
#25164 = DIRECTION ( 'NONE',  ( -1.000000000000000000, 0.000000000000000000, -0.000000000000000000 ) ) ;
#25165 = ADVANCED_FACE ( 'NONE', ( #18052 ), #28446, .T. ) ;
#25166 = CARTESIAN_POINT ( 'NONE',  ( 54.02499999726880020, 160.0630714827496206, 15.58253174999999402 ) ) ;
#25167 = CARTESIAN_POINT ( 'NONE',  ( -52.50000000000002132, 155.0000000000000000, 6.938893903907228378E-15 ) ) ;
#25168 = CARTESIAN_POINT ( 'NONE',  ( -6.220909254589682469, 215.4770327129946850, 38.94886208192144039 ) ) ;
#25169 = VERTEX_POINT ( 'NONE', #15496 ) ;
#25170 = CARTESIAN_POINT ( 'NONE',  ( 84.78867513459482552, 155.0000000000000000, -15.00000000000002487 ) ) ;
#25171 = AXIS2_PLACEMENT_3D ( 'NONE', #14293, #14128, #30141 ) ;
#25172 = FACE_OUTER_BOUND ( 'NONE', #25153, .T. ) ;
#25173 = CARTESIAN_POINT ( 'NONE',  ( 86.21132485994283456, 170.7719333635740497, -7.904646289410545231E-15 ) ) ;
#25174 = CARTESIAN_POINT ( 'NONE',  ( -6.500168698208244500, 211.6636982574061676, 20.79886208192143826 ) ) ;
#25175 = CARTESIAN_POINT ( 'NONE',  ( 6.139770520408368348, 198.4640165459539674, 56.45113791807857950 ) ) ;
#25176 = CARTESIAN_POINT ( 'NONE',  ( 3.044812012440130555, 197.4746971517856764, 47.60113791807857098 ) ) ;
#25177 = ITEM_DEFINED_TRANSFORMATION ( 'NONE', 'NONE', #30609,  #2404 ) ;
#25178 = CARTESIAN_POINT ( 'NONE',  ( 10.01549611932653860, 210.2015048109876716, 16.85113791807856032 ) ) ;
#25179 = CARTESIAN_POINT ( 'NONE',  ( 6.444103211791042618, 202.2591342207267644, 2.301137918078565825 ) ) ;
#25180 = CARTESIAN_POINT ( 'NONE',  ( 47.52499999726881441, 169.8198683612136222, -4.815267126137197984 ) ) ;
#25181 = CARTESIAN_POINT ( 'NONE',  ( -125.0000000000000000, 0.000000000000000000, 20.00000000000000000 ) ) ;
#25182 = DIRECTION ( 'NONE',  ( 1.000000000000000000, 0.000000000000000000, 0.000000000000000000 ) ) ;
#25183 = CARTESIAN_POINT ( 'NONE',  ( 11.98450388067348271, 203.0532714938637753, 29.15113791807857169 ) ) ;
#25184 = CARTESIAN_POINT ( 'NONE',  ( 82.08867513459485110, 142.2402378747194405, 9.270509831248432420 ) ) ;
#25185 = VECTOR ( 'NONE', #32955, 1000.000000000000000 ) ;
#25186 = CARTESIAN_POINT ( 'NONE',  ( 9.984503880673470277, 203.7031108863295401, 71.15113791807857524 ) ) ;
#25187 = CARTESIAN_POINT ( 'NONE',  ( -8.118202686958039038, 201.1607312380087080, 45.20113791807857240 ) ) ;
#25188 = VECTOR ( 'NONE', #1245, 1000.000000000000000 ) ;
#25189 = CARTESIAN_POINT ( 'NONE',  ( 5.000000000000000000, 4.685197434473814759, -5.637851296924623057E-15 ) ) ;
#25190 = CARTESIAN_POINT ( 'NONE',  ( 60.78867513459481842, 155.0000000000000000, -15.00000000000002487 ) ) ;
#25191 = CARTESIAN_POINT ( 'NONE',  ( -12.01549611932659722, 210.8513442034533227, 14.64886208192143258 ) ) ;
#25192 = CARTESIAN_POINT ( 'NONE',  ( -10.00000000000000711, 206.9523078486584495, 20.49886208192143755 ) ) ;
#25193 = CARTESIAN_POINT ( 'NONE',  ( 74.39999999453763735, 168.7903194862797420, -4.480746418436745593 ) ) ;
#25194 = ORIENTED_EDGE ( 'NONE', *, *, #1625, .F. ) ;
#25195 = CARTESIAN_POINT ( 'NONE',  ( -0.05014649552807705357, 194.3824533091408000, 62.75113791807856245 ) ) ;
#25196 = CARTESIAN_POINT ( 'NONE',  ( 6.500168698208129925, 211.6636982574063381, 82.70113791807858661 ) ) ;
#25197 = EDGE_CURVE ( 'NONE', #21727, #15375, #26791, .T. ) ;
#25198 = CARTESIAN_POINT ( 'NONE',  ( 10.00000000000000711, 207.0476921513415220, 36.99886208192143755 ) ) ;
#25199 = EDGE_CURVE ( 'NONE', #27213, #8568, #11315, .T. ) ;
#25200 = DIRECTION ( 'NONE',  ( 0.000000000000000000, 0.000000000000000000, 1.000000000000000000 ) ) ;
#25201 = ORIENTED_EDGE ( 'NONE', *, *, #29982, .T. ) ;
#25202 = AXIS2_PLACEMENT_3D ( 'NONE', #91, #25472, #20530 ) ;
#25203 = ORIENTED_EDGE ( 'NONE', *, *, #7954, .F. ) ;
#25204 = EDGE_LOOP ( 'NONE', ( #21226, #2036, #31013, #16435 ) ) ;
#25205 = PRODUCT ( 'BR-600', 'BR-600', '', ( #7522 ) ) ;
#25206 = EDGE_CURVE ( 'NONE', #161, #747, #18951, .T. ) ;
#25207 = CARTESIAN_POINT ( 'NONE',  ( 78.00000000000001421, 0.000000000000000000, 3.309499999999999886 ) ) ;
#25208 = CARTESIAN_POINT ( 'NONE',  ( 4.000000000000000000, -1.759474945355381958, 3.047500000000001208 ) ) ;
#25209 = VERTEX_POINT ( 'NONE', #20770 ) ;
#25210 = CARTESIAN_POINT ( 'NONE',  ( 8.015496119326531499, 209.5516654185219636, 31.85113791807857453 ) ) ;
#25211 = AXIS2_PLACEMENT_3D ( 'NONE', #17081, #4808, #14688 ) ;
#25212 = EDGE_CURVE ( 'NONE', #17290, #26453, #18426, .T. ) ;
#25213 = DIRECTION ( 'NONE',  ( 0.000000000000000000, 0.000000000000000000, 1.000000000000000000 ) ) ;
#25214 = CARTESIAN_POINT ( 'NONE',  ( 8.118202686958138514, 201.1607312380088501, 10.29886208192143471 ) ) ;
#25215 = AXIS2_PLACEMENT_3D ( 'NONE', #33250, #4971, #33423 ) ;
#25216 = CARTESIAN_POINT ( 'NONE',  ( 57.77499999726881441, 169.8198683612136222, -4.815267126137197984 ) ) ;
#25217 = ORIENTED_EDGE ( 'NONE', *, *, #24869, .T. ) ;
#25218 = CARTESIAN_POINT ( 'NONE',  ( 4.984841277089725686, 213.7757310962907411, 52.55113791807858092 ) ) ;
#25219 = CARTESIAN_POINT ( 'NONE',  ( -64.50000000000000000, -2.605762844159085212, -20.00000000000000000 ) ) ;
#25220 =( NAMED_UNIT ( * ) SI_UNIT ( $, .STERADIAN. ) SOLID_ANGLE_UNIT ( ) );
#25221 = LINE ( 'NONE', #20276, #31504 ) ;
#25222 = CARTESIAN_POINT ( 'NONE',  ( 10.00000000000000711, 207.0476921513415220, 99.99886208192143044 ) ) ;
#25223 = CARTESIAN_POINT ( 'NONE',  ( 63.17499999726880588, 145.8408176439707802, -12.60653300113719588 ) ) ;
#25224 = CARTESIAN_POINT ( 'NONE',  ( 10.00000000000000711, 206.9523078486586201, 32.00113791807856956 ) ) ;
#25225 = DIRECTION ( 'NONE',  ( 1.000000000000000000, 0.000000000000000000, 0.000000000000000000 ) ) ;
#25226 =( BOUNDED_CURVE ( )  B_SPLINE_CURVE ( 2, ( #3037, #31498, #23491, #29265, #8323, #19040, #13421, #23817, #2725, #24149, #158 ),
 .UNSPECIFIED., .F., .F. ) 
 B_SPLINE_CURVE_WITH_KNOTS ( ( 3, 2, 2, 2, 2, 3 ),
 ( 0.6785714285714283811, 0.6821428571428569398, 0.6857142857142854986, 0.6892857142857141683, 0.6928571428571427271, 0.6964285714285712858 ),
 .UNSPECIFIED. ) 
 CURVE ( )  GEOMETRIC_REPRESENTATION_ITEM ( )  RATIONAL_B_SPLINE_CURVE ( ( 1.000000000000003109, 0.9510565162951504226, 1.000000000000000000, 0.9510565162951534202, 1.000000000000000000, 0.9510565162951534202, 1.000000000000000000, 0.9510565162951534202, 1.000000000000000000, 0.9510565162951549745, 0.9999999999999984457 ) ) 
 REPRESENTATION_ITEM ( '' )  );
#25227 = CARTESIAN_POINT ( 'NONE',  ( -0.05014649552810635652, 196.4853777576173002, 14.75113791807856245 ) ) ;
#25228 = DIRECTION ( 'NONE',  ( 1.000000000000000000, 0.000000000000000000, 0.000000000000000000 ) ) ;
#25229 = AXIS2_PLACEMENT_3D ( 'NONE', #13684, #13862, #26637 ) ;
#25230 = CARTESIAN_POINT ( 'NONE',  ( 79.60000000000000853, 150.2886644046228639, 14.49999999999999645 ) ) ;
#25231 = CARTESIAN_POINT ( 'NONE',  ( -56.07926260655170836, 194.9951118559247050, 0.6454098859825110335 ) ) ;
#25232 = CARTESIAN_POINT ( 'NONE',  ( -1.269541193505925744E-15, 7.895640089090863789, -6.564402953523717166 ) ) ;
#25233 = CARTESIAN_POINT ( 'NONE',  ( -8.118202686958039038, 201.1607312380087080, 102.2011379180785866 ) ) ;
#25234 = CARTESIAN_POINT ( 'NONE',  ( 3.500000000000004885, -2.020725942163716038, -2.899999999999999911 ) ) ;
#25235 = CARTESIAN_POINT ( 'NONE',  ( 51.97499999726881725, 169.8198683612136222, 4.815267126137181997 ) ) ;
#25236 = CARTESIAN_POINT ( 'NONE',  ( -0.05014649552810635652, 196.4853777576173002, 50.75113791807856956 ) ) ;
#25237 = CARTESIAN_POINT ( 'NONE',  ( 82.52499999726880731, 140.1801316387863778, 4.815267126137185549 ) ) ;
#25238 = FACE_OUTER_BOUND ( 'NONE', #11541, .T. ) ;
#25239 = DIRECTION ( 'NONE',  ( -1.000000000000000000, -0.000000000000000000, -0.000000000000000000 ) ) ;
#25240 = CARTESIAN_POINT ( 'NONE',  ( 53.39999999453763024, 141.2096805137202580, 4.480746418436733158 ) ) ;
#25241 = ORIENTED_EDGE ( 'NONE', *, *, #29511, .F. ) ;
#25242 = CARTESIAN_POINT ( 'NONE',  ( -3.662846001190052991, 218.4274158808045740, 31.10113791807856742 ) ) ;
#25243 = AXIS2_PLACEMENT_3D ( 'NONE', #31702, #29653, #8376 ) ;
#25244 = DIRECTION ( 'NONE',  ( -0.5000000000000006661, 0.8660254037844382635, 0.000000000000000000 ) ) ;
#25245 = B_SPLINE_CURVE_WITH_KNOTS ( 'NONE', 3,
 ( #3329, #3169, #10522, #7960, #24114, #20902 ),
 .UNSPECIFIED., .F., .F.,
 ( 4, 2, 4 ),
 ( -5.145455527296316946E-06, 0.0004153350442917303517, 0.0008358155441107569450 ),
 .UNSPECIFIED. ) ;
#25246 = CARTESIAN_POINT ( 'NONE',  ( 6.139770520408223575, 215.5359834540460611, 6.548862081921434708 ) ) ;
#25247 = VERTEX_POINT ( 'NONE', #23165 ) ;
#25248 = CYLINDRICAL_SURFACE ( 'NONE', #21922, 6.500000000000000000 ) ;
#25249 = CARTESIAN_POINT ( 'NONE',  ( 3.135527875058820690, 216.4958274776887492, 58.40113791807857524 ) ) ;
#25250 = VERTEX_POINT ( 'NONE', #4763 ) ;
#25251 = CARTESIAN_POINT ( 'NONE',  ( -2.517493886309087880, 214.5937144450984135, 21.09886208192143897 ) ) ;
#25252 = LINE ( 'NONE', #14856, #8371 ) ;
#25253 = ORIENTED_EDGE ( 'NONE', *, *, #12276, .T. ) ;
#25254 = CARTESIAN_POINT ( 'NONE',  ( 8.015496119326531499, 209.5516654185219636, 1.851137918078566091 ) ) ;
#25255 = CARTESIAN_POINT ( 'NONE',  ( 32.50000000000000000, 155.0000000000000000, 15.00000000000001243 ) ) ;
#25256 = CARTESIAN_POINT ( 'NONE',  ( 7.456977232089471386, 196.8216656703012006, 91.44886208192143329 ) ) ;
#25257 = CARTESIAN_POINT ( 'NONE',  ( 34.97499999726881015, 140.1801316387863778, -4.815267126137194431 ) ) ;
#25258 = ORIENTED_EDGE ( 'NONE', *, *, #27364, .T. ) ;
#25259 = CARTESIAN_POINT ( 'NONE',  ( 44.72499999726881015, 140.1801316387863778, -4.815267126137194431 ) ) ;
#25260 = DIRECTION ( 'NONE',  ( -1.000000000000000000, 0.000000000000000000, 0.000000000000000000 ) ) ;
#25261 = CARTESIAN_POINT ( 'NONE',  ( -3.135527875058821579, 197.5041725223112223, -0.09886208192143428053 ) ) ;
#25262 =( GEOMETRIC_REPRESENTATION_CONTEXT ( 3 ) GLOBAL_UNCERTAINTY_ASSIGNED_CONTEXT ( ( #23957 ) ) GLOBAL_UNIT_ASSIGNED_CONTEXT ( ( #24849, #25352, #9684 ) ) REPRESENTATION_CONTEXT ( 'NONE', 'WORKASPACE' ) );
#25263 = CARTESIAN_POINT ( 'NONE',  ( 3.044812012439969795, 216.5253028482143520, 72.39886208192143613 ) ) ;
#25264 = CARTESIAN_POINT ( 'NONE',  ( 49.47499999726881725, 160.0630714827496206, -15.58253175000000823 ) ) ;
#25265 = DIRECTION ( 'NONE',  ( 1.000000000000000000, 0.000000000000000000, 0.000000000000000000 ) ) ;
#25266 = CARTESIAN_POINT ( 'NONE',  ( -10.00000000000000711, 207.0476921513413515, 3.501137918078566003 ) ) ;
#25267 = CARTESIAN_POINT ( 'NONE',  ( 6.500000000000000888, 2.536640449112275153, -0.3753468889000217690 ) ) ;
#25268 = CARTESIAN_POINT ( 'NONE',  ( 63.39999999999999858, 159.7113355953771077, 14.49999999999999289 ) ) ;
#25269 = CARTESIAN_POINT ( 'NONE',  ( -6.220909254589537696, 198.5229672870051161, 93.05113791807853829 ) ) ;
#25270 = CARTESIAN_POINT ( 'NONE',  ( 64.41132485994282320, 167.7597621252805880, 9.270509831248428867 ) ) ;
#25271 = CARTESIAN_POINT ( 'NONE',  ( -3.135527875058821579, 197.5041725223112223, 77.90113791807857524 ) ) ;
#25272 = DIRECTION ( 'NONE',  ( 1.000000000000000000, 0.000000000000000000, 0.000000000000000000 ) ) ;
#25273 = CARTESIAN_POINT ( 'NONE',  ( 33.87499999726881583, 171.3844434931184253, -7.942151717890132712E-15 ) ) ;
#25274 = CARTESIAN_POINT ( 'NONE',  ( -12.01549611932659722, 210.8513442034533227, 86.64886208192143613 ) ) ;
#25275 = CARTESIAN_POINT ( 'NONE',  ( 61.82499999726881157, 168.2552932293087906, 9.630534252274372875 ) ) ;
#25276 = STYLED_ITEM ( 'NONE', ( #5727 ), #21775 ) ;
#25278 = ORIENTED_EDGE ( 'NONE', *, *, #15725, .F. ) ;
#25277 = CARTESIAN_POINT ( 'NONE',  ( 9.984503880673473830, 203.7031108863295401, 20.15113791807856813 ) ) ;
#25279 = LINE ( 'NONE', #6546, #27141 ) ;
#25280 = CARTESIAN_POINT ( 'NONE',  ( 85.07499999726880446, 141.7447067706911810, -9.630534252274385310 ) ) ;
#25281 = CARTESIAN_POINT ( 'NONE',  ( -12.01549611932652972, 203.1486557965464499, 87.35113791807857808 ) ) ;
#25282 = CARTESIAN_POINT ( 'NONE',  ( 72.68867513459484542, 150.1262045565066785, -15.00000000000021316 ) ) ;
#25283 = EDGE_LOOP ( 'NONE', ( #20860, #14766, #18260, #31136 ) ) ;
#25284 = CARTESIAN_POINT ( 'NONE',  ( 11.98450388067341876, 210.9467285061363953, 72.84886208192143897 ) ) ;
#25285 = CARTESIAN_POINT ( 'NONE',  ( -10.01549611932659545, 210.2015048109875011, 77.64886208192143613 ) ) ;
#25286 = CARTESIAN_POINT ( 'NONE',  ( 7.375838497908012492, 217.2372850707501186, 12.54886208192143826 ) ) ;
#25287 = CARTESIAN_POINT ( 'NONE',  ( -6.815830331203685866, -1.210827632163352847E-13, -6.171384342982610960 ) ) ;
#25288 = CARTESIAN_POINT ( 'NONE',  ( -3.044812012440131443, 216.5253028482142952, 37.10113791807857098 ) ) ;
#25289 = CARTESIAN_POINT ( 'NONE',  ( 66.08867513459483689, 142.2402378747194405, 9.270509831248432420 ) ) ;
#25290 = CARTESIAN_POINT ( 'NONE',  ( -0.05014649552828403384, 217.5146222423826714, 99.24886208192143044 ) ) ;
#25291 = DIRECTION ( 'NONE',  ( 0.000000000000000000, -0.7071067811865475727, -0.7071067811865475727 ) ) ;
#25292 = EDGE_LOOP ( 'NONE', ( #25042, #32449, #30206, #14010, #29913 ) ) ;
#25293 = CARTESIAN_POINT ( 'NONE',  ( 112.4999999999999858, 155.0000000000000000, -6.938893903907228378E-15 ) ) ;
#25294 = CARTESIAN_POINT ( 'NONE',  ( -8.015496119326597224, 209.5516654185217362, 80.64886208192145034 ) ) ;
#25295 = ORIENTED_EDGE ( 'NONE', *, *, #19354, .F. ) ;
#25296 = EDGE_CURVE ( 'NONE', #2428, #11008, #3165, .T. ) ;
#25297 = APPLICATION_CONTEXT ( 'automotive_design' ) ;
#25298 = CARTESIAN_POINT ( 'NONE',  ( 10.40000000000000036, 0.000000000000000000, 0.000000000000000000 ) ) ;
#25299 = ORIENTED_EDGE ( 'NONE', *, *, #32414, .F. ) ;
#25300 = CARTESIAN_POINT ( 'NONE',  ( 7.847095227763521308, 4.129731495738485414, -7.493596212620238894 ) ) ;
#25301 = CARTESIAN_POINT ( 'NONE',  ( 72.87499999726881583, 138.6155565068815747, -3.929120461958505118E-15 ) ) ;
#25302 = CARTESIAN_POINT ( 'NONE',  ( 80.62499999726880162, 138.6155565068815463, -3.929120461958505118E-15 ) ) ;
#25303 = DIRECTION ( 'NONE',  ( 0.000000000000000000, -0.04769215134144196705, 0.9988620819214357738 ) ) ;
#25304 = CARTESIAN_POINT ( 'NONE',  ( 6.500168698208129925, 211.6636982574063381, 82.70113791807858661 ) ) ;
#25305 = DIRECTION ( 'NONE',  ( 1.000000000000000000, 1.804112415015879625E-16, 0.000000000000000000 ) ) ;
#25306 = SURFACE_STYLE_FILL_AREA ( #17642 ) ;
#25307 = CARTESIAN_POINT ( 'NONE',  ( 42.40000000000000568, 150.2886644046228639, -14.50000000000000888 ) ) ;
#25308 = CARTESIAN_POINT ( 'NONE',  ( -7.984503880673422316, 204.3529502787951628, 56.34886208192144608 ) ) ;
#25309 = B_SPLINE_CURVE_WITH_KNOTS ( 'NONE', 3,
 ( #14045, #8274, #6034, #24441 ),
 .UNSPECIFIED., .F., .F.,
 ( 4, 4 ),
 ( 1.680513367352531873E-18, 0.0005135163888283047259 ),
 .UNSPECIFIED. ) ;
#25310 = CARTESIAN_POINT ( 'NONE',  ( 2.000000000000000000, -1.329782007511006281, -0.7677499999999984892 ) ) ;
#25311 = CARTESIAN_POINT ( 'NONE',  ( 95.59906517536109050, 155.0000000000000000, 0.000000000000000000 ) ) ;
#25312 = CARTESIAN_POINT ( 'NONE',  ( 27.50000000000001066, 13.30988860919481986, -16.28489851701342417 ) ) ;
#25313 = CARTESIAN_POINT ( 'NONE',  ( 57.32499999726881157, 164.1591823560292198, -12.60653300113719766 ) ) ;
#25314 = CARTESIAN_POINT ( 'NONE',  ( 64.27499999726880731, 160.0630714827496206, 15.58253174999999402 ) ) ;
#25315 = CARTESIAN_POINT ( 'NONE',  ( -12.00000000000000711, 207.0476921513413515, 60.50113791807856956 ) ) ;
#25316 = LINE ( 'NONE', #30604, #8617 ) ;
#25317 = CARTESIAN_POINT ( 'NONE',  ( 7.375838497908181246, 196.7627149292499666, 2.451137918078565736 ) ) ;
#25318 = CARTESIAN_POINT ( 'NONE',  ( 6.220909254589536808, 215.4770327129947987, 73.55113791807858092 ) ) ;
#25319 = CARTESIAN_POINT ( 'NONE',  ( 0.05014649552828288198, 194.3824533091408000, 46.74886208192143755 ) ) ;
#25320 = CARTESIAN_POINT ( 'NONE',  ( -3.135527875058982783, 216.4958274776886924, 51.09886208192143897 ) ) ;
#25321 = DIRECTION ( 'NONE',  ( 1.000000000000000000, 0.000000000000000000, 0.000000000000000000 ) ) ;
#25322 = CARTESIAN_POINT ( 'NONE',  ( 3.753561863808689836, 218.3979405102790565, 85.40113791807856103 ) ) ;
#25323 = CARTESIAN_POINT ( 'NONE',  ( 83.01132485994280330, 142.2402378747194405, 9.270509831248432420 ) ) ;
#25324 = CARTESIAN_POINT ( 'NONE',  ( -10.00000000000000711, 207.0476921513413515, 6.501137918078566003 ) ) ;
#25325 = CARTESIAN_POINT ( 'NONE',  ( 6.220909254589681581, 198.5229672870052582, 70.44886208192144750 ) ) ;
#25326 = PLANE ( 'NONE',  #12382 ) ;
#25327 = VERTEX_POINT ( 'NONE', #18223 ) ;
#25328 = CARTESIAN_POINT ( 'NONE',  ( 12.01549611932659367, 203.1486557965466773, 70.14886208192142192 ) ) ;
#25329 = ORIENTED_EDGE ( 'NONE', *, *, #3314, .T. ) ;
#25330 = CARTESIAN_POINT ( 'NONE',  ( 75.87499999726881583, 171.3844434931184253, -7.942151717890132712E-15 ) ) ;
#25331 = CARTESIAN_POINT ( 'NONE',  ( 2.426778023690075337, 214.6231898156240447, 54.39886208192144323 ) ) ;
#25332 = ORIENTED_EDGE ( 'NONE', *, *, #1661, .T. ) ;
#25333 = EDGE_CURVE ( 'NONE', #7786, #30423, #8703, .T. ) ;
#25334 = CARTESIAN_POINT ( 'NONE',  ( 68.92499999726881299, 145.8408176439707802, -12.60653300113719588 ) ) ;
#25335 = CARTESIAN_POINT ( 'NONE',  ( 79.50000000000000000, 155.0000000000000000, -13.50000000000001776 ) ) ;
#25336 = DIRECTION ( 'NONE',  ( -0.000000000000000000, -0.000000000000000000, 1.000000000000000000 ) ) ;
#25337 = CARTESIAN_POINT ( 'NONE',  ( 59.42499999726882010, 168.2552932293087906, -9.630534252274385310 ) ) ;
#25338 = CARTESIAN_POINT ( 'NONE',  ( -62.70000000000000284, -88.00000000000000000, 20.00000000000000000 ) ) ;
#25339 = CARTESIAN_POINT ( 'NONE',  ( -10.00000000000000711, 206.9523078486584495, 44.49886208192143755 ) ) ;
#25340 = ORIENTED_EDGE ( 'NONE', *, *, #31069, .F. ) ;
#25341 = CARTESIAN_POINT ( 'NONE',  ( 125.0000000000000000, 4.592425496802574367E-14, -35.00000000000000000 ) ) ;
#25342 = EDGE_CURVE ( 'NONE', #6856, #27493, #20943, .T. ) ;
#25343 = CARTESIAN_POINT ( 'NONE',  ( 112.4999999999999858, 155.0000000000000000, -6.938893903907228378E-15 ) ) ;
#25344 = CARTESIAN_POINT ( 'NONE',  ( 2.000000000000000888, 0.000000000000000000, -2.899999999999999911 ) ) ;
#25345 = CARTESIAN_POINT ( 'NONE',  ( -6.444103211790928043, 202.2591342207265939, 29.19886208192143684 ) ) ;
#25346 = CARTESIAN_POINT ( 'NONE',  ( -3.044812012440131443, 216.5253028482142952, 67.10113791807857808 ) ) ;
#25347 = CARTESIAN_POINT ( 'NONE',  ( 45.28867513459482552, 170.7719333635740497, -7.904646289410545231E-15 ) ) ;
#25348 = CARTESIAN_POINT ( 'NONE',  ( 10.00000000000000711, 206.9523078486586201, 44.00113791807857666 ) ) ;
#25349 = ITEM_DEFINED_TRANSFORMATION ( 'NONE', 'NONE', #32226,  #2404 ) ;
#25350 = CARTESIAN_POINT ( 'NONE',  ( -9.984503880673473830, 210.2968891136704315, 21.65113791807856458 ) ) ;
#25351 = CARTESIAN_POINT ( 'NONE',  ( 4.903702542908601636, 200.1653181626581102, 5.451137918078566180 ) ) ;
#25352 =( NAMED_UNIT ( * ) PLANE_ANGLE_UNIT ( ) SI_UNIT ( $, .RADIAN. ) );
#25353 = CARTESIAN_POINT ( 'NONE',  ( 125.0000000000000000, 25.00000000000004619, 35.00000000000000000 ) ) ;
#25354 = CARTESIAN_POINT ( 'NONE',  ( -9.736236675707914401, 199.9851607334237542, 27.20113791807857240 ) ) ;
#25355 = DIRECTION ( 'NONE',  ( -1.000000000000000000, -0.000000000000000000, -0.000000000000000000 ) ) ;
#25356 = ADVANCED_FACE ( 'NONE', ( #18388 ), #17887, .F. ) ;
#25357 = CARTESIAN_POINT ( 'NONE',  ( 0.05014649552810505201, 217.5146222423826714, 76.25113791807855534 ) ) ;
#25358 = CARTESIAN_POINT ( 'NONE',  ( 9.984503880673473830, 203.7031108863295401, 53.15113791807857524 ) ) ;
#25359 = CARTESIAN_POINT ( 'NONE',  ( -3.499999999999999556, -3.004629197474309385E-15, 0.000000000000000000 ) ) ;
#25360 = CARTESIAN_POINT ( 'NONE',  ( 85.48867513459482836, 167.7597621252805880, 9.270509831248428867 ) ) ;
#25361 = CARTESIAN_POINT ( 'NONE',  ( -9.680171189290716072, 199.9079932115567146, 11.19886208192143506 ) ) ;
#25362 = CARTESIAN_POINT ( 'NONE',  ( 0.05014649552828275014, 196.4853777576173002, 22.74886208192143400 ) ) ;
#25363 = CARTESIAN_POINT ( 'NONE',  ( 75.29999999453762882, 142.6655632788954620, 8.961492836873471646 ) ) ;
#25364 = EDGE_LOOP ( 'NONE', ( #10808, #1248, #5344, #287 ) ) ;
#25365 = CARTESIAN_POINT ( 'NONE',  ( 3.662846001190051659, 195.5725841191953691, 56.60113791807857808 ) ) ;
#25366 = CARTESIAN_POINT ( 'NONE',  ( -4.903702542908602524, 213.8346818373418898, 75.95113791807857240 ) ) ;
#25367 = ADVANCED_FACE ( 'NONE', ( #17713 ), #7336, .T. ) ;
#25368 = CARTESIAN_POINT ( 'NONE',  ( 10.01549611932659545, 203.7984951890123853, 37.14886208192142192 ) ) ;
#25369 = AXIS2_PLACEMENT_3D ( 'NONE', #7394, #28347, #20161 ) ;
#25370 = CARTESIAN_POINT ( 'NONE',  ( 102.4138169258850581, 155.0000000000000000, 32.10452846326769816 ) ) ;
#25371 = ORIENTED_EDGE ( 'NONE', *, *, #4985, .T. ) ;
#25372 = AXIS2_PLACEMENT_3D ( 'NONE', #12344, #25115, #27836 ) ;
#25373 = VERTEX_POINT ( 'NONE', #29437 ) ;
#25374 = ORIENTED_EDGE ( 'NONE', *, *, #17849, .T. ) ;
#25375 = AXIS2_PLACEMENT_3D ( 'NONE', #6270, #21774, #23717 ) ;
#25376 = DIRECTION ( 'NONE',  ( 0.000000000000000000, 0.000000000000000000, -1.000000000000000000 ) ) ;
#25377 = CARTESIAN_POINT ( 'NONE',  ( 1.860380241283018377, 6.431462466365323927, -0.1499059597315287040 ) ) ;
#25378 = EDGE_LOOP ( 'NONE', ( #16181, #12390, #9788, #14607 ) ) ;
#25379 = CARTESIAN_POINT ( 'NONE',  ( -2.517493886308901807, 199.4062855549015012, 35.90113791807856813 ) ) ;
#25380 = CARTESIAN_POINT ( 'NONE',  ( 54.81132485994282177, 150.1262045565065364, 15.00000000000011191 ) ) ;
#25381 = CARTESIAN_POINT ( 'NONE',  ( -10.01549611932659722, 210.2015048109875011, 14.64886208192143258 ) ) ;
#25382 = CARTESIAN_POINT ( 'NONE',  ( 56.77499999726881441, 140.1801316387863778, 4.815267126137185549 ) ) ;
#25383 = EDGE_LOOP ( 'NONE', ( #12936, #18386 ) ) ;
#25384 = CARTESIAN_POINT ( 'NONE',  ( -4.903702542908602524, 213.8346818373418898, 60.95113791807857240 ) ) ;
#25385 = CARTESIAN_POINT ( 'NONE',  ( 4.000000000000000000, 1.759474945355386399, 3.047499999999995879 ) ) ;
#25386 = CARTESIAN_POINT ( 'NONE',  ( -10.00000000000000711, 206.9523078486584495, 98.49886208192143044 ) ) ;
#25387 = CARTESIAN_POINT ( 'NONE',  ( 68.37499999726881583, 155.0000000000000000, 15.58253174999999402 ) ) ;
#25388 = CARTESIAN_POINT ( 'NONE',  ( -8.062137200540920645, 212.9164362838581894, 36.80113791807856671 ) ) ;
#25389 = CARTESIAN_POINT ( 'NONE',  ( -67.50000000000000000, 155.0000000000000000, 6.938893903907228378E-15 ) ) ;
#25390 = EDGE_CURVE ( 'NONE', #73, #17702, #8815, .T. ) ;
#25391 = EDGE_CURVE ( 'NONE', #10405, #23340, #2646, .T. ) ;
#25392 = CARTESIAN_POINT ( 'NONE',  ( -10.01549611932653860, 203.7984951890123284, 18.35113791807856742 ) ) ;
#25393 = CONICAL_SURFACE ( 'NONE', #21561, 32.00000000000005684, 0.1047197551196217685 ) ;
#25394 = CARTESIAN_POINT ( 'NONE',  ( 85.50000000000000000, 155.0000000000000000, 14.49999999999999467 ) ) ;
#25395 = CARTESIAN_POINT ( 'NONE',  ( 58.50000000000001421, -88.00000000000000000, 30.00000000000000000 ) ) ;
#25396 = CARTESIAN_POINT ( 'NONE',  ( -6.220909254589537696, 198.5229672870051161, 102.0511379180785383 ) ) ;
#25397 = FACE_OUTER_BOUND ( 'NONE', #9156, .T. ) ;
#25398 = CARTESIAN_POINT ( 'NONE',  ( 52.47499999726881015, 149.9369285172503510, 15.58253174999999580 ) ) ;
#25399 = EDGE_CURVE ( 'NONE', #5869, #13101, #26881, .T. ) ;
#25400 = CARTESIAN_POINT ( 'NONE',  ( -6.139770520408369237, 215.5359834540460042, 42.95113791807856529 ) ) ;
#25401 = CIRCLE ( 'NONE', #27021, 16.00000000000000000 ) ;
#25402 = CARTESIAN_POINT ( 'NONE',  ( 80.72499999726881015, 140.1801316387863778, -4.815267126137194431 ) ) ;
#25403 = CARTESIAN_POINT ( 'NONE',  ( 52.71132485994279904, 155.0000000000000000, 15.00000000000001243 ) ) ;
#25404 = DIRECTION ( 'NONE',  ( 0.000000000000000000, 0.000000000000000000, 1.000000000000000000 ) ) ;
#25405 = CARTESIAN_POINT ( 'NONE',  ( 54.69999999453763451, 167.3344367211045096, 8.961492836873468093 ) ) ;
#25406 = ORIENTED_EDGE ( 'NONE', *, *, #26845, .T. ) ;
#25407 = CARTESIAN_POINT ( 'NONE',  ( -12.01549611932652972, 203.1486557965464499, 33.35113791807857098 ) ) ;
#25408 = EDGE_CURVE ( 'NONE', #31608, #12687, #28756, .T. ) ;
#25409 = CARTESIAN_POINT ( 'NONE',  ( 2.000000000000000000, 0.8865213383406687075, -1.535500000000000975 ) ) ;
#25410 = CARTESIAN_POINT ( 'NONE',  ( 9.984503880673420539, 210.2968891136705167, 12.84886208192143187 ) ) ;
#25411 = FACE_OUTER_BOUND ( 'NONE', #20220, .T. ) ;
#25412 = ORIENTED_EDGE ( 'NONE', *, *, #12909, .F. ) ;
#25413 = CARTESIAN_POINT ( 'NONE',  ( -0.05014649552810635652, 196.4853777576173002, 2.751137918078565114 ) ) ;
#25414 = CARTESIAN_POINT ( 'NONE',  ( -3.135527875058821579, 197.5041725223112223, 56.90113791807857524 ) ) ;
#25415 = AXIS2_PLACEMENT_3D ( 'NONE', #8871, #18773, #16041 ) ;
#25416 = ORIENTED_EDGE ( 'NONE', *, *, #6994, .T. ) ;
#25417 = CARTESIAN_POINT ( 'NONE',  ( -4.984841277089891776, 213.7757310962905990, 23.94886208192143684 ) ) ;
#25418 = AXIS2_PLACEMENT_3D ( 'NONE', #22280, #19720, #6779 ) ;
#25419 = CARTESIAN_POINT ( 'NONE',  ( -64.50000000000000000, -95.00000000000000000, 20.00000000000001776 ) ) ;
#25420 = ORIENTED_EDGE ( 'NONE', *, *, #18979, .F. ) ;
#25421 = CARTESIAN_POINT ( 'NONE',  ( -6.500168698208129925, 202.3363017425936050, 6.201137918078567068 ) ) ;
#25422 = PLANE ( 'NONE',  #20310 ) ;
#25423 = CARTESIAN_POINT ( 'NONE',  ( -12.01549611932659722, 210.8513442034533227, 92.64886208192143613 ) ) ;
#25424 = CARTESIAN_POINT ( 'NONE',  ( 35.17499999726881299, 145.8408176439707802, -12.60653300113719588 ) ) ;
#25425 = EDGE_LOOP ( 'NONE', ( #19770, #9670 ) ) ;
#25426 = CARTESIAN_POINT ( 'NONE',  ( 46.72499999726881015, 140.1801316387863778, -4.815267126137194431 ) ) ;
#25427 = CARTESIAN_POINT ( 'NONE',  ( -64.50000000000000000, 2.605762844159070557, 20.00000000000000000 ) ) ;
#25428 = CARTESIAN_POINT ( 'NONE',  ( -9.984503880673473830, 210.2968891136704315, 0.6511379180785656917 ) ) ;
#25429 = CARTESIAN_POINT ( 'NONE',  ( 8.062137200540822946, 212.9164362838583315, 66.69886208192143329 ) ) ;
#25430 = CARTESIAN_POINT ( 'NONE',  ( 45.67499999726881299, 168.2552932293087906, -9.630534252274385310 ) ) ;
#25431 = CARTESIAN_POINT ( 'NONE',  ( -67.50001199999999812, 139.7198396726429053, -7.533570508255913900 ) ) ;
#25432 = CARTESIAN_POINT ( 'NONE',  ( -8.062137200540920645, 212.9164362838581894, 3.801137918078565825 ) ) ;
#25433 = CARTESIAN_POINT ( 'NONE',  ( 6.500000000000000888, 0.3213925021621134026, 6.640738306473707756E-16 ) ) ;
#25434 = EDGE_CURVE ( 'NONE', #18140, #30922, #13520, .T. ) ;
#25435 = CARTESIAN_POINT ( 'NONE',  ( 60.80000000000001137, 167.3344367211045096, -8.961492836873482304 ) ) ;
#25436 = CARTESIAN_POINT ( 'NONE',  ( -8.062137200540920645, 212.9164362838581894, 87.80113791807856671 ) ) ;
#25437 = CARTESIAN_POINT ( 'NONE',  ( 125.5000000000000000, 155.0000000000000000, -6.938893903907228378E-15 ) ) ;
#25438 = CARTESIAN_POINT ( 'NONE',  ( 8.062137200540920645, 201.0835637161417822, 77.30113791807858092 ) ) ;
#25439 = AXIS2_PLACEMENT_3D ( 'NONE', #4945, #2890, #15832 ) ;
#25440 = FACE_OUTER_BOUND ( 'NONE', #14819, .T. ) ;
#25441 = DIRECTION ( 'NONE',  ( 0.1045284632676459352, 0.000000000000000000, -0.9945218953682740670 ) ) ;
#25442 = CARTESIAN_POINT ( 'NONE',  ( 7.456977232089471386, 196.8216656703012006, 82.44886208192144750 ) ) ;
#25443 = AXIS2_PLACEMENT_3D ( 'NONE', #21388, #26341, #21224 ) ;
#25444 = CARTESIAN_POINT ( 'NONE',  ( 64.12499999726881583, 155.0000000000000000, 15.58253174999999402 ) ) ;
#25445 = AXIS2_PLACEMENT_3D ( 'NONE', #3339, #29577, #3674 ) ;
#25447 = ORIENTED_EDGE ( 'NONE', *, *, #14363, .T. ) ;
#25446 = CARTESIAN_POINT ( 'NONE',  ( 0.05014649552810506589, 217.5146222423826714, 34.25113791807856956 ) ) ;
#25448 = CARTESIAN_POINT ( 'NONE',  ( -125.0000000000000000, -25.00000000000000000, -35.00000000000000000 ) ) ;
#25449 = CARTESIAN_POINT ( 'NONE',  ( 34.49999999453763166, 170.2462022514548323, -7.872454543227099337E-15 ) ) ;
#25450 = CARTESIAN_POINT ( 'NONE',  ( -12.00000000000000711, 207.0476921513413515, 93.50113791807858377 ) ) ;
#25451 = FACE_OUTER_BOUND ( 'NONE', #14039, .T. ) ;
#25452 = CIRCLE ( 'NONE', #29807, 112.0000000000000426 ) ;
#25453 = ORIENTED_EDGE ( 'NONE', *, *, #20177, .T. ) ;
#25454 = CARTESIAN_POINT ( 'NONE',  ( -8.118202686958138514, 212.8392687619910930, 89.79886208192144181 ) ) ;
#25455 = CARTESIAN_POINT ( 'NONE',  ( -0.05014649552828442242, 219.6175466908591716, 27.24886208192143755 ) ) ;
#25456 = CARTESIAN_POINT ( 'NONE',  ( 0.000000000000000000, 0.000000000000000000, 0.000000000000000000 ) ) ;
#25457 = CARTESIAN_POINT ( 'NONE',  ( 9.984503880673470277, 203.7031108863295401, 32.15113791807857524 ) ) ;
#25458 = FACE_OUTER_BOUND ( 'NONE', #11750, .T. ) ;
#25459 = CARTESIAN_POINT ( 'NONE',  ( 3.135527875058981895, 197.5041725223112792, 100.5988620819214390 ) ) ;
#25460 = DIRECTION ( 'NONE',  ( -1.000000000000000000, -0.000000000000000000, -0.000000000000000000 ) ) ;
#25461 = ORIENTED_EDGE ( 'NONE', *, *, #15577, .F. ) ;
#25462 = CARTESIAN_POINT ( 'NONE',  ( -31.74999999999995737, 0.000000000000000000, 0.000000000000000000 ) ) ;
#25463 = CARTESIAN_POINT ( 'NONE',  ( -2.517493886309087880, 214.5937144450984135, 81.09886208192143897 ) ) ;
#25464 =( BOUNDED_CURVE ( )  B_SPLINE_CURVE ( 2, ( #32258, #29540, #16758, #19144, #29887, #16921, #29205, #18988, #11820, #11156, #26975 ),
 .UNSPECIFIED., .F., .F. ) 
 B_SPLINE_CURVE_WITH_KNOTS ( ( 3, 2, 2, 2, 2, 3 ),
 ( 0.1785714285714282146, 0.1821428571428567733, 0.1857142857142854431, 0.1892857142857139741, 0.1928571428571425328, 0.1964285714285710915 ),
 .UNSPECIFIED. ) 
 CURVE ( )  GEOMETRIC_REPRESENTATION_ITEM ( )  RATIONAL_B_SPLINE_CURVE ( ( 1.000000000000003775, 0.9510565162951496454, 1.000000000000000000, 0.9510565162951534202, 1.000000000000000000, 0.9510565162951534202, 1.000000000000000000, 0.9510565162951534202, 1.000000000000000000, 0.9510565162951576390, 0.9999999999999957812 ) ) 
 REPRESENTATION_ITEM ( '' )  );
#25465 = CIRCLE ( 'NONE', #18946, 2.149999999999994138 ) ;
#25466 = VERTEX_POINT ( 'NONE', #3539 ) ;
#25467 = CONICAL_SURFACE ( 'NONE', #10793, 3.499999999999999556, 1.047197551196589638 ) ;
#25468 = DIRECTION ( 'NONE',  ( 0.3362851123284906207, 0.04491457122451913281, 0.9406885799869860731 ) ) ;
#25469 = ORIENTED_EDGE ( 'NONE', *, *, #1901, .T. ) ;
#25470 = DIRECTION ( 'NONE',  ( -1.000000000000000000, 0.000000000000000000, 0.000000000000000000 ) ) ;
#25471 = CARTESIAN_POINT ( 'NONE',  ( 82.12499999726881583, 155.0000000000000000, 15.58253174999999402 ) ) ;
#25472 = DIRECTION ( 'NONE',  ( 1.000000000000000000, 0.000000000000000000, 0.000000000000000000 ) ) ;
#25473 = CARTESIAN_POINT ( 'NONE',  ( 6.444103211791042618, 202.2591342207267644, 74.30113791807858092 ) ) ;
#25474 = DIRECTION ( 'NONE',  ( 1.000000000000000000, 0.000000000000000000, 0.000000000000000000 ) ) ;
#25475 = CIRCLE ( 'NONE', #23319, 5.200000000000002842 ) ;
#25476 =( NAMED_UNIT ( * ) PLANE_ANGLE_UNIT ( ) SI_UNIT ( $, .RADIAN. ) );
#25477 = CARTESIAN_POINT ( 'NONE',  ( 40.90000000000000568, 168.7903194862797420, -4.480746418436745593 ) ) ;
#25478 = CARTESIAN_POINT ( 'NONE',  ( -4.984841277089891776, 213.7757310962905990, 50.94886208192143329 ) ) ;
#25479 = CARTESIAN_POINT ( 'NONE',  ( -3.135527875058821579, 197.5041725223112223, 5.901137918078566358 ) ) ;
#25480 = CARTESIAN_POINT ( 'NONE',  ( -128.2263702798683767, 4.198250922590450074, 35.00001200000001234 ) ) ;
#25481 = CARTESIAN_POINT ( 'NONE',  ( 54.52499999726881441, 140.1801316387863778, 4.815267126137185549 ) ) ;
#25482 = CARTESIAN_POINT ( 'NONE',  ( 71.27499999726880731, 149.9369285172503510, -15.58253175000000823 ) ) ;
#25483 = CARTESIAN_POINT ( 'NONE',  ( 7.456977232089302632, 217.1783343296989131, 55.55113791807858092 ) ) ;
#25484 = FACE_BOUND ( 'NONE', #13387, .T. ) ;
#25485 = AXIS2_PLACEMENT_3D ( 'NONE', #8634, #29588, #31639 ) ;
#25486 = CARTESIAN_POINT ( 'NONE',  ( 7.375838497908181246, 196.7627149292499666, 8.451137918078563516 ) ) ;
#25487 = EDGE_CURVE ( 'NONE', #27043, #982, #23859, .T. ) ;
#25488 = CARTESIAN_POINT ( 'NONE',  ( 3.044812012440130555, 197.4746971517856764, 77.60113791807857808 ) ) ;
#25489 = CIRCLE ( 'NONE', #30930, 4.200000000000001954 ) ;
#25490 = CARTESIAN_POINT ( 'NONE',  ( -12.00000000000000711, 206.9523078486584780, 38.49886208192143044 ) ) ;
#25491 = CARTESIAN_POINT ( 'NONE',  ( 6.139770520408223575, 215.5359834540460611, 60.54886208192142760 ) ) ;
#25492 = DIRECTION ( 'NONE',  ( -1.000000000000000000, 0.000000000000000000, 0.000000000000000000 ) ) ;
#25493 = CARTESIAN_POINT ( 'NONE',  ( 9.680171189290831535, 199.9079932115568852, 89.30113791807858092 ) ) ;
#25494 = CARTESIAN_POINT ( 'NONE',  ( 32.50000000000000000, 155.0000000000000000, -15.00000000000002487 ) ) ;
#25495 = CARTESIAN_POINT ( 'NONE',  ( 10.00000000000000711, 206.9523078486586201, 5.001137918078565114 ) ) ;
#25496 = CARTESIAN_POINT ( 'NONE',  ( 8.118202686958138514, 201.1607312380088501, 67.29886208192144181 ) ) ;
#25497 = DIRECTION ( 'NONE',  ( 0.000000000000000000, 0.000000000000000000, -1.000000000000000000 ) ) ;
#25498 = CIRCLE ( 'NONE', #30963, 1.610000000000000098 ) ;
#25499 = ORIENTED_EDGE ( 'NONE', *, *, #16789, .F. ) ;
#25500 = CARTESIAN_POINT ( 'NONE',  ( 12.01549611932659367, 203.1486557965466773, 73.14886208192142192 ) ) ;
#25501 = VERTEX_POINT ( 'NONE', #321 ) ;
#25502 = CARTESIAN_POINT ( 'NONE',  ( 78.37499999726883004, 155.0000000000000000, 15.58253174999999402 ) ) ;
#25503 = CARTESIAN_POINT ( 'NONE',  ( -2.517493886309087880, 214.5937144450984135, 48.09886208192143897 ) ) ;
#25504 = B_SPLINE_CURVE_WITH_KNOTS ( 'NONE', 3,
 ( #28338, #28506, #17948, #33444, #10453, #17766, #20827, #33613, #10620, #23050, #31066, #31232, #25431, #2613, #10115, #17598, #23217, #28664, #12492, #28163, #7724, #4820, #25605, #23553, #22881, #25775, #20494, #30726, #5323, #4994, #33272, #15381, #30897, #2270 ),
 .UNSPECIFIED., .F., .F.,
 ( 4, 2, 2, 2, 2, 2, 2, 2, 2, 2, 2, 2, 2, 2, 2, 2, 4 ),
 ( 0.5000000000000000000, 0.5312500000000000000, 0.5625000000000000000, 0.5937500000000001110, 0.6250000000000001110, 0.6562500000000001110, 0.6875000000000002220, 0.7187500000000002220, 0.7500000000000002220, 0.7812500000000002220, 0.8125000000000002220, 0.8437500000000001110, 0.8750000000000001110, 0.9062500000000000000, 0.9375000000000000000, 0.9687500000000000000, 1.000000000000000000 ),
 .UNSPECIFIED. ) ;
#25505 = EDGE_LOOP ( 'NONE', ( #10997, #8002, #14509, #6480 ) ) ;
#25506 = CARTESIAN_POINT ( 'NONE',  ( 70.02499999726879309, 160.0630714827496206, 15.58253174999999224 ) ) ;
#25507 = CARTESIAN_POINT ( 'NONE',  ( 1.500000000000001332, 0.000000000000000000, 8.000000000000000000 ) ) ;
#25508 = CARTESIAN_POINT ( 'NONE',  ( -57.24307706584514932, 194.9404480003898925, -2.185445380844633689 ) ) ;
#25509 = AXIS2_PLACEMENT_3D ( 'NONE', #15431, #15591, #28717 ) ;
#25510 = CARTESIAN_POINT ( 'NONE',  ( 65.62499999726880162, 171.3844434931184253, -7.942151717890132712E-15 ) ) ;
#25511 = SURFACE_SIDE_STYLE ('',( #30630 ) ) ;
#25512 = CARTESIAN_POINT ( 'NONE',  ( 6.139770520408223575, 215.5359834540460611, 45.54886208192144181 ) ) ;
#25513 = EDGE_LOOP ( 'NONE', ( #14717, #13228, #17203, #21477 ) ) ;
#25514 = CARTESIAN_POINT ( 'NONE',  ( 25.25629716696158411, 17.17253483735094832, -16.29170001372757071 ) ) ;
#25515 = CIRCLE ( 'NONE', #21695, 0.4000000000000001887 ) ;
#25516 = CARTESIAN_POINT ( 'NONE',  ( -3.135527875058821579, 197.5041725223112223, 56.90113791807857524 ) ) ;
#25517 = SURFACE_STYLE_USAGE ( .BOTH. , #15467 ) ;
#25518 = CYLINDRICAL_SURFACE ( 'NONE', #31626, 13.00000000000002487 ) ;
#25519 = CARTESIAN_POINT ( 'NONE',  ( -2.517493886309087880, 214.5937144450984135, 24.09886208192143897 ) ) ;
#25520 = CARTESIAN_POINT ( 'NONE',  ( 3.044812012440130555, 197.4746971517856764, 71.60113791807857808 ) ) ;
#25521 = CARTESIAN_POINT ( 'NONE',  ( 0.000000000000000000, 0.000000000000000000, -25.03750572909317285 ) ) ;
#25522 = CARTESIAN_POINT ( 'NONE',  ( -6.220909254589537696, 198.5229672870051161, 57.05113791807857382 ) ) ;
#25523 = AXIS2_PLACEMENT_3D ( 'NONE', #30213, #25265, #19479 ) ;
#25524 = CARTESIAN_POINT ( 'NONE',  ( 0.05014649552810505201, 217.5146222423826714, 16.25113791807856600 ) ) ;
#25525 = CARTESIAN_POINT ( 'NONE',  ( 7.984503880673485376, 204.3529502787953902, 2.151137918078566802 ) ) ;
#25526 = CARTESIAN_POINT ( 'NONE',  ( -125.0000000000000000, 25.00000000000000000, -35.00000000000000000 ) ) ;
#25527 = CARTESIAN_POINT ( 'NONE',  ( 36.22499999726881015, 149.9369285172503510, 15.58253174999999580 ) ) ;
#25528 = CARTESIAN_POINT ( 'NONE',  ( 12.00000000000000711, 206.9523078486586485, 32.00113791807856956 ) ) ;
#25529 = CARTESIAN_POINT ( 'NONE',  ( -4.250000000000000000, 5.204748896376250699E-16, -10.00000000000000000 ) ) ;
#25530 = CARTESIAN_POINT ( 'NONE',  ( -10.00000000000000711, 207.0476921513413515, 72.50113791807858377 ) ) ;
#25531 = EDGE_CURVE ( 'NONE', #562, #7373, #11300, .T. ) ;
#25532 = CARTESIAN_POINT ( 'NONE',  ( 6.220909254589536808, 215.4770327129947987, 49.55113791807855961 ) ) ;
#25533 = CARTESIAN_POINT ( 'NONE',  ( -130.2500000000000000, 6.429395695523609083E-16, 35.00000599999999906 ) ) ;
#25534 = CARTESIAN_POINT ( 'NONE',  ( -3.753561863808878130, 218.3979405102790281, 15.09886208192143719 ) ) ;
#25535 = CARTESIAN_POINT ( 'NONE',  ( -6.139770520408224463, 198.4640165459539105, 17.04886208192143471 ) ) ;
#25536 = CARTESIAN_POINT ( 'NONE',  ( 72.59999999453762598, 168.7903194862797420, 4.480746418436729606 ) ) ;
#25537 = VERTEX_POINT ( 'NONE', #24321 ) ;
#25538 = CARTESIAN_POINT ( 'NONE',  ( -9.736236675707914401, 199.9851607334237542, 60.20113791807857240 ) ) ;
#25539 = EDGE_CURVE ( 'NONE', #8613, #1044, #31503, .T. ) ;
#25540 = CIRCLE ( 'NONE', #4331, 2.149999999999996803 ) ;
#25541 = CARTESIAN_POINT ( 'NONE',  ( -2.517493886308901807, 199.4062855549015012, 80.90113791807858945 ) ) ;
#25542 = CARTESIAN_POINT ( 'NONE',  ( -8.062137200540822946, 201.0835637161416400, 38.19886208192143329 ) ) ;
#25543 = CARTESIAN_POINT ( 'NONE',  ( -54.30000000000001847, -88.00000000000000000, -20.00000000000000000 ) ) ;
#25544 = VERTEX_POINT ( 'NONE', #19215 ) ;
#25545 = EDGE_CURVE ( 'NONE', #2476, #5152, #14593, .T. ) ;
#25546 = CARTESIAN_POINT ( 'NONE',  ( -12.00000000000000711, 206.9523078486584780, 41.49886208192143044 ) ) ;
#25547 = VERTEX_POINT ( 'NONE', #18555 ) ;
#25548 = ORIENTED_EDGE ( 'NONE', *, *, #3126, .F. ) ;
#25549 =( REPRESENTATION_RELATIONSHIP ('NONE','NONE', #25663, #22175 ) REPRESENTATION_RELATIONSHIP_WITH_TRANSFORMATION ( #12065 )SHAPE_REPRESENTATION_RELATIONSHIP( ) );
#25550 = FACE_OUTER_BOUND ( 'NONE', #6598, .T. ) ;
#25551 = CARTESIAN_POINT ( 'NONE',  ( -64.50000000000000000, 120.3589838486224437, 20.00000000000000000 ) ) ;
#25552 = ORIENTED_EDGE ( 'NONE', *, *, #17712, .T. ) ;
#25553 = CARTESIAN_POINT ( 'NONE',  ( -4.984841277089726574, 200.2242689037092305, 36.05113791807856671 ) ) ;
#25554 = DIRECTION ( 'NONE',  ( 0.000000000000000000, 0.000000000000000000, -1.000000000000000000 ) ) ;
#25555 = CARTESIAN_POINT ( 'NONE',  ( 9.984503880673420539, 210.2968891136705167, 15.84886208192143719 ) ) ;
#25556 = CARTESIAN_POINT ( 'NONE',  ( 55.77499999726881441, 169.8198683612136222, -4.815267126137197984 ) ) ;
#25557 = ORIENTED_EDGE ( 'NONE', *, *, #22273, .T. ) ;
#25558 = CARTESIAN_POINT ( 'NONE',  ( -2.517493886308901807, 199.4062855549015012, 59.90113791807856813 ) ) ;
#25559 = DIRECTION ( 'NONE',  ( 0.000000000000000000, 0.000000000000000000, 1.000000000000000000 ) ) ;
#25560 = CIRCLE ( 'NONE', #15231, 15.50000000000001066 ) ;
#25561 = CARTESIAN_POINT ( 'NONE',  ( -0.05014649552828403384, 217.5146222423826714, 96.24886208192144466 ) ) ;
#25562 = EDGE_CURVE ( 'NONE', #20431, #33389, #27649, .T. ) ;
#25563 = CARTESIAN_POINT ( 'NONE',  ( 67.47499999726879594, 160.0630714827496206, -15.58253175000000823 ) ) ;
#25564 = CARTESIAN_POINT ( 'NONE',  ( -6.220909254589537696, 198.5229672870051161, 42.05113791807857382 ) ) ;
#25565 = FACE_OUTER_BOUND ( 'NONE', #15450, .T. ) ;
#25566 = CARTESIAN_POINT ( 'NONE',  ( -3.135527875058821579, 197.5041725223112223, 20.90113791807856813 ) ) ;
#25567 = DIRECTION ( 'NONE',  ( 0.000000000000000000, 0.000000000000000000, -1.000000000000000000 ) ) ;
#25568 = PRODUCT_CONTEXT ( 'NONE', #29421, 'mechanical' ) ;
#25569 = CARTESIAN_POINT ( 'NONE',  ( 33.82499999726880446, 168.2552932293087906, 9.630534252274372875 ) ) ;
#25570 = DIRECTION ( 'NONE',  ( 0.000000000000000000, -1.000000000000000000, 0.000000000000000000 ) ) ;
#25571 = DIRECTION ( 'NONE',  ( 0.000000000000000000, 0.000000000000000000, -1.000000000000000000 ) ) ;
#25572 = CARTESIAN_POINT ( 'NONE',  ( -6.139770520408369237, 215.5359834540460042, 99.95113791807855819 ) ) ;
#25573 = CARTESIAN_POINT ( 'NONE',  ( 86.71132485994282035, 155.0000000000000000, 15.00000000000001243 ) ) ;
#25574 = CARTESIAN_POINT ( 'NONE',  ( 51.07499999726879736, 141.7447067706911810, -9.630534252274385310 ) ) ;
#25575 = CARTESIAN_POINT ( 'NONE',  ( 10.00000000000000711, 206.9523078486586201, 47.00113791807856956 ) ) ;
#25576 = EDGE_CURVE ( 'NONE', #780, #24055, #16483, .T. ) ;
#25577 = DIRECTION ( 'NONE',  ( 0.000000000000000000, 0.000000000000000000, -1.000000000000000000 ) ) ;
#25578 = CARTESIAN_POINT ( 'NONE',  ( 52.31132485994280046, 169.2658477444273331, 4.635254915624208216 ) ) ;
#25579 = CYLINDRICAL_SURFACE ( 'NONE', #18984, 4.000000000000000888 ) ;
#25580 = CARTESIAN_POINT ( 'NONE',  ( 50.89999999453763735, 159.7113355953771077, 14.49999999999999289 ) ) ;
#25581 = ORIENTED_EDGE ( 'NONE', *, *, #11366, .F. ) ;
#25582 = CARTESIAN_POINT ( 'NONE',  ( -7.375838497908182134, 217.2372850707499765, 33.95113791807856529 ) ) ;
#25583 = CARTESIAN_POINT ( 'NONE',  ( 102.4138169258850581, 155.0000000000000000, 0.000000000000000000 ) ) ;
#25584 = CARTESIAN_POINT ( 'NONE',  ( 10.01549611932659545, 203.7984951890123853, 16.14886208192143613 ) ) ;
#25585 = DIRECTION ( 'NONE',  ( -1.000000000000000000, 0.000000000000000000, -0.000000000000000000 ) ) ;
#25586 = ORIENTED_EDGE ( 'NONE', *, *, #25197, .F. ) ;
#25587 = ADVANCED_FACE ( 'NONE', ( #32155 ), #24935, .F. ) ;
#25588 = CARTESIAN_POINT ( 'NONE',  ( -8.062137200540920645, 212.9164362838581894, 9.801137918078566713 ) ) ;
#25589 = CARTESIAN_POINT ( 'NONE',  ( 9.984503880673470277, 203.7031108863295401, 74.15113791807854682 ) ) ;
#25590 = ORIENTED_EDGE ( 'NONE', *, *, #16647, .F. ) ;
#25591 = CARTESIAN_POINT ( 'NONE',  ( 7.984503880673422316, 209.6470497212048372, 18.84886208192143187 ) ) ;
#25592 = CARTESIAN_POINT ( 'NONE',  ( 3.809068165403724393, 5.306386968807659699, 9.757819552369535962E-16 ) ) ;
#25593 = ORIENTED_EDGE ( 'NONE', *, *, #32425, .T. ) ;
#25594 = CARTESIAN_POINT ( 'NONE',  ( 2.426778023690261410, 199.3768101843759837, 5.601137918078567424 ) ) ;
#25595 = EDGE_CURVE ( 'NONE', #12632, #11089, #28712, .T. ) ;
#25596 = CARTESIAN_POINT ( 'NONE',  ( -7.375838497908014268, 196.7627149292498530, 86.04886208192145602 ) ) ;
#25597 = CARTESIAN_POINT ( 'NONE',  ( 36.47499999726881015, 149.9369285172503510, 15.58253174999999580 ) ) ;
#25598 = ORIENTED_EDGE ( 'NONE', *, *, #17095, .F. ) ;
#25599 = CARTESIAN_POINT ( 'NONE',  ( 46.82499999726880446, 141.7447067706911810, -9.630534252274385310 ) ) ;
#25600 = LINE ( 'NONE', #28501, #6636 ) ;
#25601 = CARTESIAN_POINT ( 'NONE',  ( 0.05014649552810505201, 217.5146222423826714, 7.251137918078566003 ) ) ;
#25602 = CARTESIAN_POINT ( 'NONE',  ( -3.135527875058982783, 216.4958274776886924, 72.09886208192143897 ) ) ;
#25603 = EDGE_CURVE ( 'NONE', #11640, #25501, #12980, .T. ) ;
#25604 = CARTESIAN_POINT ( 'NONE',  ( 44.57499999726881157, 145.8408176439707802, 12.60653300113718345 ) ) ;
#25605 = CARTESIAN_POINT ( 'NONE',  ( -67.50001199999998391, 140.2468628165998439, 8.519561460567032896 ) ) ;
#25606 = CARTESIAN_POINT ( 'NONE',  ( 6.139770520408368348, 198.4640165459539674, 17.45113791807855819 ) ) ;
#25607 = CARTESIAN_POINT ( 'NONE',  ( -63.49999999999884892, 212.5000000000003695, -3.061616997868142046E-16 ) ) ;
#25608 = CARTESIAN_POINT ( 'NONE',  ( 70.00000000000000000, 139.7537977485451393, -4.138211985947621020E-15 ) ) ;
#25609 = CARTESIAN_POINT ( 'NONE',  ( 6.220909254589536808, 215.4770327129947702, 94.55113791807858092 ) ) ;
#25610 = CARTESIAN_POINT ( 'NONE',  ( -6.139770520408369237, 215.5359834540460042, 72.95113791807854398 ) ) ;
#25611 = CARTESIAN_POINT ( 'NONE',  ( -2.352174619740013739, 7.302225387956623237, -7.450218641348505422 ) ) ;
#25612 = CARTESIAN_POINT ( 'NONE',  ( 27.50000000000000355, 15.87713240271474291, -2.456200930618646971 ) ) ;
#25613 = CARTESIAN_POINT ( 'NONE',  ( 12.01549611932659367, 203.1486557965466773, 88.14886208192143613 ) ) ;
#25614 = CARTESIAN_POINT ( 'NONE',  ( 72.42499999726881299, 141.7447067706911810, 9.630534252274376428 ) ) ;
#25616 = ORIENTED_EDGE ( 'NONE', *, *, #23828, .T. ) ;
#25615 = CARTESIAN_POINT ( 'NONE',  ( -3.044812012440131443, 216.5253028482142952, 28.10113791807857098 ) ) ;
#25617 = DIRECTION ( 'NONE',  ( -1.000000000000000000, 0.000000000000000000, 0.000000000000000000 ) ) ;
#25618 = CARTESIAN_POINT ( 'NONE',  ( 88.37499999726880162, 155.0000000000000000, 15.58253174999999402 ) ) ;
#25619 = CARTESIAN_POINT ( 'NONE',  ( -3.753561863808691168, 195.6020594897209435, 92.90113791807857524 ) ) ;
#25620 = CARTESIAN_POINT ( 'NONE',  ( -10.90161837886387808, 206.5319970171666455, 103.9075498093380645 ) ) ;
#25621 = VERTEX_POINT ( 'NONE', #17335 ) ;
#25622 = CARTESIAN_POINT ( 'NONE',  ( 6.220909254589680693, 198.5229672870052582, 85.44886208192143329 ) ) ;
#25623 = AXIS2_PLACEMENT_3D ( 'NONE', #15629, #23139, #12573 ) ;
#25624 = CARTESIAN_POINT ( 'NONE',  ( 7.375838497908012492, 217.2372850707501186, 24.54886208192144181 ) ) ;
#25625 = CARTESIAN_POINT ( 'NONE',  ( 9.092171885314265012, -26.50489691992491714, -0.2827231011780930725 ) ) ;
#25626 = CARTESIAN_POINT ( 'NONE',  ( 8.062137200540920645, 201.0835637161417822, 32.30113791807857382 ) ) ;
#25627 = EDGE_LOOP ( 'NONE', ( #19830, #32231, #10177, #32766 ) ) ;
#25628 = CARTESIAN_POINT ( 'NONE',  ( 9.984503880673420539, 210.2968891136705167, 96.84886208192139634 ) ) ;
#25629 = EDGE_CURVE ( 'NONE', #13926, #26841, #11548, .T. ) ;
#25630 = ADVANCED_FACE ( 'NONE', ( #32997 ), #14101, .F. ) ;
#25631 = CARTESIAN_POINT ( 'NONE',  ( 1.098735407079667992, 7.248058225760153128, -6.326622577870739228 ) ) ;
#25632 = ORIENTED_EDGE ( 'NONE', *, *, #17842, .T. ) ;
#25633 = CARTESIAN_POINT ( 'NONE',  ( -9.963617232950836566, 205.9538967796982547, 104.4520962529709465 ) ) ;
#25634 = CARTESIAN_POINT ( 'NONE',  ( -6.444103211790928043, 202.2591342207265939, 77.19886208192143329 ) ) ;
#25635 = ADVANCED_FACE ( 'NONE', ( #9496 ), #30112, .F. ) ;
#25636 = EDGE_LOOP ( 'NONE', ( #4171, #2088, #15026, #27515 ) ) ;
#25637 = EDGE_CURVE ( 'NONE', #32991, #13221, #9360, .T. ) ;
#25638 = CARTESIAN_POINT ( 'NONE',  ( 34.61132485994281183, 159.8737954434934636, 15.00000000000012967 ) ) ;
#25639 = ORIENTED_EDGE ( 'NONE', *, *, #637, .F. ) ;
#25640 = CARTESIAN_POINT ( 'NONE',  ( 80.91132485994280898, 146.1832212156128890, 12.13525491562421976 ) ) ;
#25641 = CARTESIAN_POINT ( 'NONE',  ( 2.426778023690261410, 199.3768101843759837, 59.60113791807857808 ) ) ;
#25642 = CARTESIAN_POINT ( 'NONE',  ( 83.92499999726882720, 164.1591823560292198, 12.60653300113718167 ) ) ;
#25643 = CARTESIAN_POINT ( 'NONE',  ( 101.3062541159399075, 155.0000000000000000, 12.00000000000001066 ) ) ;
#25644 = CARTESIAN_POINT ( 'NONE',  ( -6.500168698208129925, 202.3363017425936050, 87.20113791807858661 ) ) ;
#25645 = CARTESIAN_POINT ( 'NONE',  ( 99.99999999999998579, 0.000000000000000000, 4.171999999999999709 ) ) ;
#25646 = CIRCLE ( 'NONE', #3309, 19.99999999999998934 ) ;
#25647 = CARTESIAN_POINT ( 'NONE',  ( 47.39999999999999147, 159.7113355953771077, 14.49999999999999289 ) ) ;
#25648 = CARTESIAN_POINT ( 'NONE',  ( -2.517493886309087880, 214.5937144450984135, 63.09886208192143187 ) ) ;
#25649 = CARTESIAN_POINT ( 'NONE',  ( 37.71132485994279904, 155.0000000000000000, -15.00000000000002487 ) ) ;
#25650 = CARTESIAN_POINT ( 'NONE',  ( 112.4999999999999858, 155.0000000000000000, -6.938893903907228378E-15 ) ) ;
#25651 = CARTESIAN_POINT ( 'NONE',  ( -6.500000000000000888, 2.759383090082417667, -5.880088986491048608 ) ) ;
#25652 = CARTESIAN_POINT ( 'NONE',  ( -120.4126214611401338, 2.643999646947222892, 35.00001199999999812 ) ) ;
#25653 = CARTESIAN_POINT ( 'NONE',  ( 54.62499999726880873, 138.6155565068815747, -3.929120461958505118E-15 ) ) ;
#25654 = CARTESIAN_POINT ( 'NONE',  ( 71.77499999726882152, 169.8198683612136222, -4.815267126137197984 ) ) ;
#25655 = CARTESIAN_POINT ( 'NONE',  ( -9.680171189290831535, 214.0920067884431148, 66.80113791807858092 ) ) ;
#25656 = DIRECTION ( 'NONE',  ( 1.000000000000000000, 0.000000000000000000, 0.000000000000000000 ) ) ;
#25657 = CARTESIAN_POINT ( 'NONE',  ( -9.680171189290831535, 214.0920067884431148, 12.80113791807856849 ) ) ;
#25658 = CARTESIAN_POINT ( 'NONE',  ( -6.139770520408368348, 215.5359834540460042, 90.95113791807855819 ) ) ;
#25659 = CARTESIAN_POINT ( 'NONE',  ( 11.98450388067341876, 210.9467285061363953, 54.84886208192143187 ) ) ;
#25660 = CARTESIAN_POINT ( 'NONE',  ( 8.062137200540822946, 212.9164362838583315, 54.69886208192143329 ) ) ;
#25661 = FACE_OUTER_BOUND ( 'NONE', #27875, .T. ) ;
#25662 = CARTESIAN_POINT ( 'NONE',  ( -9.736236675707914401, 199.9851607334237542, 93.20113791807858661 ) ) ;
#25663 = SHAPE_REPRESENTATION ( 'BR-600', ( #8823, #10489, #15911, #11556, #1754, #1224, #12656, #9367, #29507, #30609, #24080, #17541, #18642, #24622, #14812, #139, #20808, #6094, #20265, #30066, #19168, #8304, #28979, #22422, #14275, #15384, #5573, #22993, #2859, #21354, #4482, #6676, #33331, #32226, #23537, #31698, #692 ), #26775 ) ;
#25664 = CARTESIAN_POINT ( 'NONE',  ( -67.50000599999999906, 155.0000000000000000, 17.00000000000001421 ) ) ;
#25665 = CARTESIAN_POINT ( 'NONE',  ( 6.220909254589536808, 215.4770327129947702, 1.551137918078565825 ) ) ;
#25666 = CARTESIAN_POINT ( 'NONE',  ( 6.220909254589681581, 198.5229672870052582, 73.44886208192139065 ) ) ;
#25667 = DIRECTION ( 'NONE',  ( 1.000000000000000000, 0.000000000000000000, 0.000000000000000000 ) ) ;
#25668 = EDGE_LOOP ( 'NONE', ( #6863, #22182, #6224, #8238 ) ) ;
#25669 = CARTESIAN_POINT ( 'NONE',  ( -3.753561863808878130, 218.3979405102790281, 81.09886208192143897 ) ) ;
#25670 = AXIS2_PLACEMENT_3D ( 'NONE', #6505, #8393, #1059 ) ;
#25671 = CARTESIAN_POINT ( 'NONE',  ( -8.118202686958039038, 201.1607312380087080, 90.20113791807857240 ) ) ;
#25672 = ORIENTED_EDGE ( 'NONE', *, *, #26191, .T. ) ;
#25673 = CARTESIAN_POINT ( 'NONE',  ( 77.57499999726881867, 164.1591823560292198, -12.60653300113719766 ) ) ;
#25674 = CARTESIAN_POINT ( 'NONE',  ( -0.05014649552828365914, 215.4116977939061144, 48.24886208192144466 ) ) ;
#25675 = ORIENTED_EDGE ( 'NONE', *, *, #32214, .F. ) ;
#25676 = CARTESIAN_POINT ( 'NONE',  ( 72.42499999726881299, 141.7447067706911810, 9.630534252274376428 ) ) ;
#25677 = CARTESIAN_POINT ( 'NONE',  ( 6.826575449902429149, 2.663085462279306981, -6.347418139105299950 ) ) ;
#25678 = CARTESIAN_POINT ( 'NONE',  ( -55.99986651211894184, 195.0000083429897586, 0.1629166443388770646 ) ) ;
#25679 = AXIS2_PLACEMENT_3D ( 'NONE', #20823, #7890, #23549 ) ;
#25680 = CARTESIAN_POINT ( 'NONE',  ( 66.42499999726879878, 141.7447067706911810, 9.630534252274376428 ) ) ;
#25681 = DIRECTION ( 'NONE',  ( 1.000000000000000000, 0.000000000000000000, 0.000000000000000000 ) ) ;
#25682 = CARTESIAN_POINT ( 'NONE',  ( -8.118202686958138514, 212.8392687619910930, 56.79886208192143471 ) ) ;
#25683 = VERTEX_POINT ( 'NONE', #1829 ) ;
#25684 = CARTESIAN_POINT ( 'NONE',  ( 14.33345751131667889, 23.47883925285266571, -18.00000000000000000 ) ) ;
#25685 = CARTESIAN_POINT ( 'NONE',  ( -61.00000000000002842, 209.9999999999999716, -3.061616997868380183E-16 ) ) ;
#25686 = CARTESIAN_POINT ( 'NONE',  ( 6.444103211790928043, 211.7408657792734061, 30.69886208192143684 ) ) ;
#25687 = CARTESIAN_POINT ( 'NONE',  ( 9.984503880673470277, 203.7031108863295401, 68.15113791807857524 ) ) ;
#25688 = DIRECTION ( 'NONE',  ( 0.000000000000000000, 0.000000000000000000, 1.000000000000000000 ) ) ;
#25689 = CARTESIAN_POINT ( 'NONE',  ( -8.118202686958039038, 201.1607312380087080, 54.20113791807857240 ) ) ;
#25690 = CARTESIAN_POINT ( 'NONE',  ( 3.135527875058820690, 216.4958274776887492, 28.40113791807856813 ) ) ;
#25691 = CARTESIAN_POINT ( 'NONE',  ( -6.500168698208129925, 202.3363017425936050, 9.201137918078563516 ) ) ;
#25692 = LINE ( 'NONE', #20924, #11892 ) ;
#25693 = FACE_OUTER_BOUND ( 'NONE', #24535, .T. ) ;
#25694 = CARTESIAN_POINT ( 'NONE',  ( 40.92499999726881299, 145.8408176439707802, -12.60653300113719588 ) ) ;
#25695 = CARTESIAN_POINT ( 'NONE',  ( -12.01549611932652972, 203.1486557965464499, 42.35113791807857098 ) ) ;
#25696 = DIRECTION ( 'NONE',  ( -1.000000000000000000, -1.804112415015879378E-16, 0.000000000000000000 ) ) ;
#25697 = CARTESIAN_POINT ( 'NONE',  ( -10.00000000000000711, 207.0476921513413515, 81.50113791807856956 ) ) ;
#25698 = CARTESIAN_POINT ( 'NONE',  ( 6.139770520408367460, 198.4640165459539389, 62.45113791807857950 ) ) ;
#25699 = CARTESIAN_POINT ( 'NONE',  ( 3.469446951953614189E-15, -4.041451884327432076, -2.899999999999999911 ) ) ;
#25700 = CARTESIAN_POINT ( 'NONE',  ( 12.01549611932659367, 203.1486557965466773, 16.14886208192143613 ) ) ;
#25701 = CARTESIAN_POINT ( 'NONE',  ( -10.00000000000000711, 206.9523078486584495, 26.49886208192143755 ) ) ;
#25702 = CARTESIAN_POINT ( 'NONE',  ( 74.89999999453760893, 159.7113355953771077, 14.49999999999999289 ) ) ;
#25703 = AXIS2_PLACEMENT_3D ( 'NONE', #24293, #26517, #6063 ) ;
#25704 = ORIENTED_EDGE ( 'NONE', *, *, #6446, .T. ) ;
#25705 = CARTESIAN_POINT ( 'NONE',  ( 3.662846001190051659, 195.5725841191953691, 71.60113791807857808 ) ) ;
#25706 = CARTESIAN_POINT ( 'NONE',  ( 6.500168698208129925, 211.6636982574063381, 79.70113791807857240 ) ) ;
#25707 = AXIS2_PLACEMENT_3D ( 'NONE', #23580, #18296, #31252 ) ;
#25708 = CARTESIAN_POINT ( 'NONE',  ( 8.118202686958138514, 201.1607312380088501, 37.29886208192143471 ) ) ;
#25709 = CARTESIAN_POINT ( 'NONE',  ( 0.000000000000000000, 0.000000000000000000, 0.000000000000000000 ) ) ;
#25710 = ORIENTED_EDGE ( 'NONE', *, *, #22179, .F. ) ;
#25711 = CARTESIAN_POINT ( 'NONE',  ( 7.456977232089471386, 196.8216656703012006, 46.44886208192143329 ) ) ;
#25712 = ORIENTED_EDGE ( 'NONE', *, *, #17849, .F. ) ;
#25713 = EDGE_LOOP ( 'NONE', ( #24581, #31169, #10305, #28948 ) ) ;
#25714 = CARTESIAN_POINT ( 'NONE',  ( 78.00000000000001421, 0.000000000000000000, 0.000000000000000000 ) ) ;
#25715 = CARTESIAN_POINT ( 'NONE',  ( -3.499999999999997780, -2.020725942163716038, -2.899999999999999911 ) ) ;
#25716 = CARTESIAN_POINT ( 'NONE',  ( 55.78867513459481842, 155.0000000000000000, 15.00000000000001243 ) ) ;
#25717 = ORIENTED_EDGE ( 'NONE', *, *, #18090, .T. ) ;
#25718 = CARTESIAN_POINT ( 'NONE',  ( 0.05014649552807626948, 215.4116977939061144, 43.25113791807856956 ) ) ;
#25719 = SURFACE_STYLE_FILL_AREA ( #168 ) ;
#25720 = EDGE_CURVE ( 'NONE', #17462, #31129, #13499, .T. ) ;
#25721 = CARTESIAN_POINT ( 'NONE',  ( -3.044812012439970683, 197.4746971517856196, 19.89886208192143613 ) ) ;
#25722 = CARTESIAN_POINT ( 'NONE',  ( 54.37499999726881583, 155.0000000000000000, 15.58253174999999402 ) ) ;
#25723 = EDGE_LOOP ( 'NONE', ( #4148, #20487, #32822 ) ) ;
#25724 = CARTESIAN_POINT ( 'NONE',  ( 5.000000000000000000, 4.685197434473814759, -5.637851296924623057E-15 ) ) ;
#25725 = CONICAL_SURFACE ( 'NONE', #18124, 3.309499999999999886, 0.7853981633974710386 ) ;
#25726 = PRESENTATION_STYLE_ASSIGNMENT (( #28292 ) ) ;
#25727 = DIRECTION ( 'NONE',  ( -1.000000000000000000, 0.000000000000000000, -0.000000000000000000 ) ) ;
#25728 = CARTESIAN_POINT ( 'NONE',  ( -10.01549611932659722, 210.2015048109875011, 95.64886208192140771 ) ) ;
#25729 = AXIS2_PLACEMENT_3D ( 'NONE', #31737, #8409, #24234 ) ;
#25730 = CARTESIAN_POINT ( 'NONE',  ( 6.139770520408368348, 198.4640165459539674, 41.45113791807857240 ) ) ;
#25731 = DIRECTION ( 'NONE',  ( 1.000000000000000000, 0.000000000000000000, 0.000000000000000000 ) ) ;
#25732 = CARTESIAN_POINT ( 'NONE',  ( -6.139770520408369237, 215.5359834540460042, 30.95113791807857240 ) ) ;
#25733 = CARTESIAN_POINT ( 'NONE',  ( 9.984503880673420539, 210.2968891136705736, 99.84886208192142476 ) ) ;
#25734 = CARTESIAN_POINT ( 'NONE',  ( -6.500168698208244500, 211.6636982574061676, 80.79886208192144181 ) ) ;
#25735 = CARTESIAN_POINT ( 'NONE',  ( 33.22499999726881725, 160.0630714827496206, -15.58253175000000823 ) ) ;
#25736 = CARTESIAN_POINT ( 'NONE',  ( 0.000000000000000000, 0.000000000000000000, 0.000000000000000000 ) ) ;
#25737 = CARTESIAN_POINT ( 'NONE',  ( 77.30950000000004252, 0.000000000000000000, 0.000000000000000000 ) ) ;
#25738 = CARTESIAN_POINT ( 'NONE',  ( -9.680171189290831535, 214.0920067884431148, 9.801137918078564937 ) ) ;
#25739 = CARTESIAN_POINT ( 'NONE',  ( 64.78867513459482552, 155.0000000000000000, -15.00000000000002487 ) ) ;
#25740 = CARTESIAN_POINT ( 'NONE',  ( 47.77499999726881441, 169.8198683612136222, -4.815267126137197984 ) ) ;
#25741 = CARTESIAN_POINT ( 'NONE',  ( 8.118202686958039038, 212.8392687619912635, 52.70113791807857240 ) ) ;
#25742 = DIRECTION ( 'NONE',  ( -1.000000000000000000, 0.000000000000000000, -0.000000000000000000 ) ) ;
#25743 = FACE_OUTER_BOUND ( 'NONE', #726, .T. ) ;
#25744 = CARTESIAN_POINT ( 'NONE',  ( 6.139770520408223575, 215.5359834540460611, 3.548862081921434708 ) ) ;
#25745 = CARTESIAN_POINT ( 'NONE',  ( 51.49999999453763166, 139.7537977485451393, -4.138211985947621020E-15 ) ) ;
#25746 = ORIENTED_EDGE ( 'NONE', *, *, #27409, .T. ) ;
#25747 = CARTESIAN_POINT ( 'NONE',  ( -7.375838497908182134, 217.2372850707499765, 24.95113791807856884 ) ) ;
#25748 = CARTESIAN_POINT ( 'NONE',  ( -1.750000000000016209, -3.031088913245524985, 0.000000000000000000 ) ) ;
#25749 = CARTESIAN_POINT ( 'NONE',  ( 9.984503880673420539, 210.2968891136705167, 15.84886208192143719 ) ) ;
#25750 =( REPRESENTATION_RELATIONSHIP ('NONE','NONE', #25663, #22175 ) REPRESENTATION_RELATIONSHIP_WITH_TRANSFORMATION ( #9509 )SHAPE_REPRESENTATION_RELATIONSHIP( ) );
#25751 = DIRECTION ( 'NONE',  ( 0.000000000000000000, -1.000000000000000000, 0.000000000000000000 ) ) ;
#25752 = ORIENTED_EDGE ( 'NONE', *, *, #6049, .F. ) ;
#25753 = AXIS2_PLACEMENT_3D ( 'NONE', #32124, #31631, #10691 ) ;
#25754 = CARTESIAN_POINT ( 'NONE',  ( 6.139770520408368348, 198.4640165459539674, 8.451137918078565292 ) ) ;
#25755 = CARTESIAN_POINT ( 'NONE',  ( -8.118202686958039038, 201.1607312380087080, 69.20113791807858661 ) ) ;
#25756 = AXIS2_PLACEMENT_3D ( 'NONE', #8577, #32240, #14360 ) ;
#25757 = ORIENTED_EDGE ( 'NONE', *, *, #24726, .T. ) ;
#25758 = CARTESIAN_POINT ( 'NONE',  ( -6.444103211790928043, 202.2591342207265939, 29.19886208192143684 ) ) ;
#25759 = CONICAL_SURFACE ( 'NONE', #1265, 3.499999999999999556, 1.047197551196589638 ) ;
#25760 = CARTESIAN_POINT ( 'NONE',  ( 2.243702833038388356, -30.45886237079322356, -16.29170001372754228 ) ) ;
#25761 = CARTESIAN_POINT ( 'NONE',  ( 76.07499999726880446, 168.2552932293087906, 9.630534252274372875 ) ) ;
#25762 = VERTEX_POINT ( 'NONE', #6262 ) ;
#25763 = CARTESIAN_POINT ( 'NONE',  ( -8.000000000000008882, 207.0476921513413515, 6.501137918078566891 ) ) ;
#25764 = ADVANCED_FACE ( 'NONE', ( #14438 ), #11718, .F. ) ;
#25765 = CARTESIAN_POINT ( 'NONE',  ( -12.01549611932659722, 210.8513442034533227, 86.64886208192143613 ) ) ;
#25766 = CARTESIAN_POINT ( 'NONE',  ( 36.87499999726881583, 138.6155565068815747, -3.929120461958505118E-15 ) ) ;
#25767 = ORIENTED_EDGE ( 'NONE', *, *, #28341, .T. ) ;
#25768 = CARTESIAN_POINT ( 'NONE',  ( 46.62499999726880873, 138.6155565068815463, -3.929120461958505118E-15 ) ) ;
#25769 = CARTESIAN_POINT ( 'NONE',  ( 7.500000000000000888, 3.639598441879751345, -0.7155132341745285007 ) ) ;
#25770 = CARTESIAN_POINT ( 'NONE',  ( 8.118202686958039038, 212.8392687619912635, 7.701137918078566180 ) ) ;
#25771 = VECTOR ( 'NONE', #14459, 1000.000000000000000 ) ;
#25772 =( GEOMETRIC_REPRESENTATION_CONTEXT ( 3 ) GLOBAL_UNCERTAINTY_ASSIGNED_CONTEXT ( ( #3622 ) ) GLOBAL_UNIT_ASSIGNED_CONTEXT ( ( #9632, #23094, #25130 ) ) REPRESENTATION_CONTEXT ( 'NONE', 'WORKASPACE' ) );
#25773 = CARTESIAN_POINT ( 'NONE',  ( -6.139770520408224463, 198.4640165459539389, 71.04886208192139918 ) ) ;
#25774 = CARTESIAN_POINT ( 'NONE',  ( 44.17499999726881299, 164.1591823560292198, 12.60653300113718167 ) ) ;
#25775 = CARTESIAN_POINT ( 'NONE',  ( -67.50001199999998391, 143.7659452401275928, 12.80757580047018962 ) ) ;
#25776 = CARTESIAN_POINT ( 'NONE',  ( 3.044812012440130555, 197.4746971517856764, 8.601137918078565647 ) ) ;
#25777 = PRODUCT_DEFINITION_SHAPE ( 'NONE', 'NONE',  #33692 ) ;
#25778 = CARTESIAN_POINT ( 'NONE',  ( 5.000000000000000000, 4.685197434473814759, -5.637851296924623057E-15 ) ) ;
#25779 = ADVANCED_FACE ( 'NONE', ( #6776 ), #27547, .T. ) ;
#25780 = VECTOR ( 'NONE', #29499, 1000.000000000000000 ) ;
#25781 = CARTESIAN_POINT ( 'NONE',  ( 70.09999999999999432, 141.2096805137202580, -4.480746418436742040 ) ) ;
#25782 =( BOUNDED_CURVE ( )  B_SPLINE_CURVE ( 2, ( #29495, #11607, #5813, #3775, #11276, #21657, #21823, #16210, #32213, #32053, #8716 ),
 .UNSPECIFIED., .F., .T. ) 
 B_SPLINE_CURVE_WITH_KNOTS ( ( 3, 2, 2, 2, 2, 3 ),
 ( 0.2499999999999996947, 0.2535714285714282812, 0.2571428571428568399, 0.2607142857142853987, 0.2642857142857140129, 0.2678571428571425717 ),
 .UNSPECIFIED. ) 
 CURVE ( )  GEOMETRIC_REPRESENTATION_ITEM ( )  RATIONAL_B_SPLINE_CURVE ( ( 1.000000000000004219, 0.9510565162951492013, 1.000000000000000000, 0.9510565162951534202, 1.000000000000000000, 0.9510565162951534202, 1.000000000000000000, 0.9510565162951534202, 1.000000000000000000, 0.9510565162951564178, 0.9999999999999970024 ) ) 
 REPRESENTATION_ITEM ( '' )  );
#25783 = CARTESIAN_POINT ( 'NONE',  ( 9.984503880673470277, 203.7031108863295401, 98.15113791807858945 ) ) ;
#25784 = LINE ( 'NONE', #17954, #1169 ) ;
#25785 = CARTESIAN_POINT ( 'NONE',  ( 10.01549611932653860, 210.2015048109876716, 79.85113791807853545 ) ) ;
#25786 = CARTESIAN_POINT ( 'NONE',  ( 3.500000000000004885, 0.6879904500768362352, -0.03016324292412390917 ) ) ;
#25787 = CIRCLE ( 'NONE', #2421, 6.500000000000000888 ) ;
#25788 = FACE_OUTER_BOUND ( 'NONE', #17635, .T. ) ;
#25789 = CARTESIAN_POINT ( 'NONE',  ( 7.375838497908012492, 217.2372850707501186, 84.54886208192144181 ) ) ;
#25790 = AXIS2_PLACEMENT_3D ( 'NONE', #31045, #17574, #28644 ) ;
#25791 = CARTESIAN_POINT ( 'NONE',  ( 71.42499999726879878, 168.2552932293087906, -9.630534252274385310 ) ) ;
#25792 = VERTEX_POINT ( 'NONE', #14771 ) ;
#25793 = CARTESIAN_POINT ( 'NONE',  ( -59.60814253741918378, 194.9368883388851259, -2.246975524854183170 ) ) ;
#25794 = CARTESIAN_POINT ( 'NONE',  ( 86.97499999726882436, 140.1801316387863778, -4.815267126137194431 ) ) ;
#25795 = CARTESIAN_POINT ( 'NONE',  ( -3.662846001190052991, 218.4274158808045740, 100.1011379180785781 ) ) ;
#25796 = ADVANCED_FACE ( 'NONE', ( #3712 ), #19555, .F. ) ;
#25797 = DIRECTION ( 'NONE',  ( 0.000000000000000000, 0.000000000000000000, 1.000000000000000000 ) ) ;
#25798 = VERTEX_POINT ( 'NONE', #12051 ) ;
#25799 = AXIS2_PLACEMENT_3D ( 'NONE', #26971, #3633, #15913 ) ;
#25800 = CARTESIAN_POINT ( 'NONE',  ( 6.139770520408223575, 215.5359834540460611, 87.54886208192142760 ) ) ;
#25801 = CARTESIAN_POINT ( 'NONE',  ( 9.680171189290716072, 214.0920067884432854, 21.69886208192144039 ) ) ;
#25802 = CARTESIAN_POINT ( 'NONE',  ( 115.4999999999999858, 61.05130719884917312, -52.99999999999945999 ) ) ;
#25803 = CARTESIAN_POINT ( 'NONE',  ( -6.220909254589537696, 198.5229672870051161, 39.05113791807856671 ) ) ;
#25804 = EDGE_CURVE ( 'NONE', #23132, #8055, #4385, .T. ) ;
#25805 = EDGE_LOOP ( 'NONE', ( #19517, #14401, #11546, #9849 ) ) ;
#25806 = CARTESIAN_POINT ( 'NONE',  ( 0.05014649552828275708, 196.4853777576173002, 103.7488620819214589 ) ) ;
#25807 = PLANE ( 'NONE',  #2926 ) ;
#25808 = ORIENTED_EDGE ( 'NONE', *, *, #24018, .T. ) ;
#25809 = CARTESIAN_POINT ( 'NONE',  ( 8.015496119326595448, 204.4483345814782638, 85.14886208192143613 ) ) ;
#25810 = CIRCLE ( 'NONE', #30155, 19.99999999999998934 ) ;
#25811 = VERTEX_POINT ( 'NONE', #9325 ) ;
#25812 = FACE_OUTER_BOUND ( 'NONE', #21813, .T. ) ;
#25814 = VERTEX_POINT ( 'NONE', #29948 ) ;
#25813 = B_SPLINE_CURVE_WITH_KNOTS ( 'NONE', 3,
 ( #26451, #26779, #24405, #16387, #8403, #21335 ),
 .UNSPECIFIED., .F., .F.,
 ( 4, 2, 4 ),
 ( 0.003605240635278501252, 0.004627368318297491422, 0.005649496001316482025 ),
 .UNSPECIFIED. ) ;
#25815 = CARTESIAN_POINT ( 'NONE',  ( 81.21132485994280614, 139.2280666364260071, -4.041636747397287284E-15 ) ) ;
#25816 = CARTESIAN_POINT ( 'NONE',  ( 2.426778023690261410, 199.3768101843759837, 56.60113791807857808 ) ) ;
#25817 = CARTESIAN_POINT ( 'NONE',  ( 85.72499999726882436, 169.8198683612136222, 4.815267126137181997 ) ) ;
#25818 = CARTESIAN_POINT ( 'NONE',  ( 51.71132485994281325, 155.0000000000000000, -15.00000000000002487 ) ) ;
#25819 = CARTESIAN_POINT ( 'NONE',  ( -2.517493886308901807, 199.4062855549015012, 86.90113791807857524 ) ) ;
#25820 = CARTESIAN_POINT ( 'NONE',  ( 0.5974722283283632196, -8.315303285985693904, -0.7026937717022971874 ) ) ;
#25821 = CARTESIAN_POINT ( 'NONE',  ( 47.50000000000000000, 155.0000000000000000, 14.49999999999999467 ) ) ;
#25822 = CARTESIAN_POINT ( 'NONE',  ( -6.500168698208244500, 211.6636982574061676, 65.79886208192144181 ) ) ;
#25823 = EDGE_CURVE ( 'NONE', #16872, #16076, #31481, .T. ) ;
#25824 = ADVANCED_FACE ( 'NONE', ( #24831, #25163, #16824, #19717, #27381, #25005, #27219, #19883, #32830, #24667 ), #4047, .F. ) ;
#25825 = CARTESIAN_POINT ( 'NONE',  ( 48.32499999726881157, 145.8408176439707802, 12.60653300113718345 ) ) ;
#25826 = DIRECTION ( 'NONE',  ( 1.000000000000000000, 0.000000000000000000, 0.000000000000000000 ) ) ;
#25827 = FACE_OUTER_BOUND ( 'NONE', #3239, .T. ) ;
#25828 = CARTESIAN_POINT ( 'NONE',  ( 59.52499999726881441, 169.8198683612136222, -4.815267126137197984 ) ) ;
#25829 = CARTESIAN_POINT ( 'NONE',  ( 69.77499999726880731, 169.8198683612136222, -4.815267126137197984 ) ) ;
#25830 = CARTESIAN_POINT ( 'NONE',  ( -9.736236675707914401, 199.9851607334237542, 66.20113791807857240 ) ) ;
#25831 = CARTESIAN_POINT ( 'NONE',  ( 2.886521338340684917, 4.440929409521844457E-17, 0.000000000000000000 ) ) ;
#25832 = PRODUCT_RELATED_PRODUCT_CATEGORY ( 'part', '', ( #3690 ) ) ;
#25833 = CARTESIAN_POINT ( 'NONE',  ( -11.98450388067348804, 210.9467285061362247, 6.651137918078566358 ) ) ;
#25834 = ADVANCED_FACE ( 'NONE', ( #10527, #9844, #7796, #4560, #10022 ), #22953, .T. ) ;
#25835 = CARTESIAN_POINT ( 'NONE',  ( -3.135527875058821579, 197.5041725223112223, 89.90113791807857524 ) ) ;
#25836 = CARTESIAN_POINT ( 'NONE',  ( 11.98450388067341876, 210.9467285061363953, 51.84886208192144608 ) ) ;
#25837 = CARTESIAN_POINT ( 'NONE',  ( -8.118202686958138514, 212.8392687619910930, 56.79886208192143471 ) ) ;
#25838 = CARTESIAN_POINT ( 'NONE',  ( -1.282512619719133662, -8.391164935524759727, -7.795653906409117262 ) ) ;
#25839 = CARTESIAN_POINT ( 'NONE',  ( -12.00000000000000711, 207.0476921513413515, 99.50113791807856956 ) ) ;
#25840 = CARTESIAN_POINT ( 'NONE',  ( 68.21132485994280614, 170.7719333635740497, -7.904646289410545231E-15 ) ) ;
#25841 = CARTESIAN_POINT ( 'NONE',  ( -0.05014649552810635652, 196.4853777576173002, 17.75113791807856245 ) ) ;
#25842 = EDGE_CURVE ( 'NONE', #18876, #30423, #15113, .T. ) ;
#25843 = CARTESIAN_POINT ( 'NONE',  ( -6.220909254589682469, 215.4770327129946850, 71.94886208192144750 ) ) ;
#25844 = ORIENTED_EDGE ( 'NONE', *, *, #19789, .F. ) ;
#25845 = CARTESIAN_POINT ( 'NONE',  ( 3.662846001189864698, 218.4274158808046593, 81.39886208192143613 ) ) ;
#25846 = CARTESIAN_POINT ( 'NONE',  ( 10.01549611932653860, 210.2015048109876716, 94.85113791807857808 ) ) ;
#25847 = ORIENTED_EDGE ( 'NONE', *, *, #29775, .T. ) ;
#25848 = CARTESIAN_POINT ( 'NONE',  ( 75.47499999726881015, 160.0630714827496206, -15.58253175000000823 ) ) ;
#25849 = CARTESIAN_POINT ( 'NONE',  ( 8.015496119326595448, 204.4483345814782638, 49.14886208192145034 ) ) ;
#25850 = ORIENTED_EDGE ( 'NONE', *, *, #2230, .T. ) ;
#25851 = CARTESIAN_POINT ( 'NONE',  ( 74.42499999726881299, 141.7447067706911810, 9.630534252274376428 ) ) ;
#25852 = CARTESIAN_POINT ( 'NONE',  ( 6.500000000000000000, -1.417018949932591365, -5.722407714414702085 ) ) ;
#25853 = CARTESIAN_POINT ( 'NONE',  ( 72.99495483890930814, 155.0000000000000000, 15.50000000000000355 ) ) ;
#25854 = CARTESIAN_POINT ( 'NONE',  ( 64.52499999726882152, 140.1801316387863778, 4.815267126137185549 ) ) ;
#25855 = FACE_OUTER_BOUND ( 'NONE', #13891, .T. ) ;
#25856 = CARTESIAN_POINT ( 'NONE',  ( 3.044812012439969795, 216.5253028482143520, 51.39886208192143613 ) ) ;
#25857 = ORIENTED_EDGE ( 'NONE', *, *, #25342, .F. ) ;
#25858 = CARTESIAN_POINT ( 'NONE',  ( 0.000000000000000000, -0.8865213383406721492, -1.535499999999998977 ) ) ;
#25859 = DIRECTION ( 'NONE',  ( 1.000000000000000000, 0.000000000000000000, 0.000000000000000000 ) ) ;
#25860 = CARTESIAN_POINT ( 'NONE',  ( 6.500168698208244500, 202.3363017425938324, 31.29886208192143826 ) ) ;
#25861 = CARTESIAN_POINT ( 'NONE',  ( 10.00000000000000711, 206.9523078486586201, 74.00113791807858377 ) ) ;
#25862 = CYLINDRICAL_SURFACE ( 'NONE', #32685, 5.000000000000000888 ) ;
#25863 = CARTESIAN_POINT ( 'NONE',  ( -8.062137200540920645, 212.9164362838581894, 54.80113791807857382 ) ) ;
#25864 = ITEM_DEFINED_TRANSFORMATION ( 'NONE', 'NONE', #23537,  #2404 ) ;
#25865 = CARTESIAN_POINT ( 'NONE',  ( 3.135527875058820690, 216.4958274776887492, 25.40113791807856813 ) ) ;
#25866 = CARTESIAN_POINT ( 'NONE',  ( 2.426778023690261410, 199.3768101843759837, 11.60113791807856742 ) ) ;
#25867 = DIRECTION ( 'NONE',  ( -1.000000000000000000, 0.000000000000000000, 0.000000000000000000 ) ) ;
#25868 = FACE_OUTER_BOUND ( 'NONE', #8821, .T. ) ;
#25869 = CARTESIAN_POINT ( 'NONE',  ( 35.22499999726881015, 160.0630714827496206, -15.58253175000000823 ) ) ;
#25870 = CARTESIAN_POINT ( 'NONE',  ( 7.375838497908181246, 196.7627149292499666, 38.45113791807856529 ) ) ;
#25871 = FACE_BOUND ( 'NONE', #14063, .T. ) ;
#25872 = CARTESIAN_POINT ( 'NONE',  ( 6.220909254589536808, 215.4770327129947702, 88.55113791807853829 ) ) ;
#25873 = CARTESIAN_POINT ( 'NONE',  ( -6.139770520408368348, 215.5359834540460042, 54.95113791807856529 ) ) ;
#25874 = CARTESIAN_POINT ( 'NONE',  ( 104.9083388212530537, 155.0000000000000000, 32.00000000000000000 ) ) ;
#25875 = B_SPLINE_CURVE_WITH_KNOTS ( 'NONE', 3,
 ( #5154, #15542, #9935, #18440, #20490, #2101, #218, #10615, #12488, #53, #7720, #30722, #31226, #30893, #15377, #7382, #17944, #17761 ),
 .UNSPECIFIED., .F., .F.,
 ( 4, 2, 2, 2, 2, 2, 2, 2, 4 ),
 ( 0.000000000000000000, 0.06250000000000059674, 0.1250000000000012212, 0.1875000000000018874, 0.2500000000000024980, 0.3125000000000018874, 0.3750000000000012212, 0.4375000000000006106, 0.5000000000000000000 ),
 .UNSPECIFIED. ) ;
#25876 = CARTESIAN_POINT ( 'NONE',  ( 7.375838497908012492, 217.2372850707501186, 21.54886208192143471 ) ) ;
#25877 = CARTESIAN_POINT ( 'NONE',  ( -8.062137200540822946, 201.0835637161416400, 32.19886208192143329 ) ) ;
#25878 = CARTESIAN_POINT ( 'NONE',  ( 76.09999999453762598, 159.7113355953771077, -14.50000000000000888 ) ) ;
#25879 = CARTESIAN_POINT ( 'NONE',  ( -7.456977232089304408, 196.8216656703010301, 69.05113791807856671 ) ) ;
#25880 = CARTESIAN_POINT ( 'NONE',  ( -4.984841277089726574, 200.2242689037092305, 78.05113791807858092 ) ) ;
#25881 = CARTESIAN_POINT ( 'NONE',  ( -10.01549611932659722, 210.2015048109875011, 38.64886208192142192 ) ) ;
#25882 = CARTESIAN_POINT ( 'NONE',  ( 125.5000000000000000, 157.1500000000010573, 105.9999999999999858 ) ) ;
#25883 = EDGE_LOOP ( 'NONE', ( #33507, #17711, #24421, #30318 ) ) ;
#25884 = CARTESIAN_POINT ( 'NONE',  ( 3.662846001189864698, 218.4274158808046593, 54.39886208192143613 ) ) ;
#25885 = ORIENTED_EDGE ( 'NONE', *, *, #25391, .F. ) ;
#25886 = EDGE_LOOP ( 'NONE', ( #12937, #4934 ) ) ;
#25887 = CARTESIAN_POINT ( 'NONE',  ( 6.826399921716642005, 2.638123634694624631, -6.344399053232583796 ) ) ;
#25888 = DIRECTION ( 'NONE',  ( 1.000000000000000000, 0.000000000000000000, 0.000000000000000000 ) ) ;
#25889 = ORIENTED_EDGE ( 'NONE', *, *, #15102, .F. ) ;
#25890 = CARTESIAN_POINT ( 'NONE',  ( -2.517493886308901807, 199.4062855549015012, 44.90113791807856813 ) ) ;
#25891 = CARTESIAN_POINT ( 'NONE',  ( 108.0159016311981759, 155.0000000000000000, 0.000000000000000000 ) ) ;
#25892 = CARTESIAN_POINT ( 'NONE',  ( 3.135527875058981895, 197.5041725223112792, 22.59886208192143542 ) ) ;
#25893 = CARTESIAN_POINT ( 'NONE',  ( 60.67499999726881299, 141.7447067706911810, 9.630534252274376428 ) ) ;
#25894 = ORIENTED_EDGE ( 'NONE', *, *, #26852, .T. ) ;
#25895 = DIRECTION ( 'NONE',  ( 0.7071067811865475727, 0.7071067811865475727, 0.000000000000000000 ) ) ;
#25896 = FACE_OUTER_BOUND ( 'NONE', #29187, .T. ) ;
#25897 = CARTESIAN_POINT ( 'NONE',  ( -8.015496119326597224, 209.5516654185217362, 5.648862081921434353 ) ) ;
#25898 = CARTESIAN_POINT ( 'NONE',  ( -8.062137200540920645, 212.9164362838581894, 45.80113791807856671 ) ) ;
#25899 = LINE ( 'NONE', #15837, #7840 ) ;
#25900 = CARTESIAN_POINT ( 'NONE',  ( 10.01549611932653860, 210.2015048109876716, 28.85113791807855677 ) ) ;
#25901 = CARTESIAN_POINT ( 'NONE',  ( -3.135527875058982783, 216.4958274776886924, 102.0988620819214390 ) ) ;
#25902 = APPLICATION_PROTOCOL_DEFINITION ( 'draft international standard', 'automotive_design', 1998, #22914 ) ;
#25903 = CARTESIAN_POINT ( 'NONE',  ( -4.903702542908436435, 200.1653181626580249, 92.04886208192142760 ) ) ;
#25904 = CARTESIAN_POINT ( 'NONE',  ( 34.82499999726881157, 141.7447067706911810, -9.630534252274385310 ) ) ;
#25905 = CARTESIAN_POINT ( 'NONE',  ( 5.000000000000000000, 2.342598717236900718, -4.057500000000001883 ) ) ;
#25906 = CARTESIAN_POINT ( 'NONE',  ( -7.375838497908182134, 217.2372850707499765, 9.951137918078567068 ) ) ;
#25907 = CARTESIAN_POINT ( 'NONE',  ( -12.99999999999999112, -3.903127820947815962E-15, -8.000000000000000000 ) ) ;
#25908 = CARTESIAN_POINT ( 'NONE',  ( 48.17499999726881299, 164.1591823560292198, 12.60653300113718167 ) ) ;
#25909 = CARTESIAN_POINT ( 'NONE',  ( -0.05014649552810635652, 196.4853777576173002, 53.75113791807857666 ) ) ;
#25910 = CIRCLE ( 'NONE', #30333, 4.057500000000000107 ) ;
#25911 = CARTESIAN_POINT ( 'NONE',  ( 35.61132485994281183, 150.1262045565064511, -15.00000000000005329 ) ) ;
#25912 = DIRECTION ( 'NONE',  ( -1.000000000000000000, -0.000000000000000000, -0.000000000000000000 ) ) ;
#25913 = CARTESIAN_POINT ( 'NONE',  ( 65.51132485994280330, 146.1832212156128890, -12.13525491562423042 ) ) ;
#25914 = CARTESIAN_POINT ( 'NONE',  ( 55.59999999453763309, 141.2096805137202580, -4.480746418436742040 ) ) ;
#25915 = ORIENTED_EDGE ( 'NONE', *, *, #13542, .F. ) ;
#25916 = CARTESIAN_POINT ( 'NONE',  ( 11.98450388067348271, 203.0532714938637753, 41.15113791807857524 ) ) ;
#25917 = LINE ( 'NONE', #18255, #28965 ) ;
#25918 = ADVANCED_FACE ( 'NONE', ( #20734 ), #1533, .T. ) ;
#25919 = CARTESIAN_POINT ( 'NONE',  ( 3.044812012439969795, 216.5253028482143520, 9.398862081921436129 ) ) ;
#25920 = CARTESIAN_POINT ( 'NONE',  ( 59.71132485994280614, 155.0000000000000000, -15.00000000000002487 ) ) ;
#25921 = EDGE_LOOP ( 'NONE', ( #8987, #7537, #4974 ) ) ;
#25922 = CARTESIAN_POINT ( 'NONE',  ( -3.044812012440131443, 216.5253028482142952, 13.10113791807856742 ) ) ;
#25923 = CARTESIAN_POINT ( 'NONE',  ( 8.062137200540920645, 201.0835637161417822, 71.30113791807856671 ) ) ;
#25924 = VERTEX_POINT ( 'NONE', #30457 ) ;
#25925 = CARTESIAN_POINT ( 'NONE',  ( 4.903702542908435547, 213.8346818373419751, 33.54886208192144181 ) ) ;
#25926 = CARTESIAN_POINT ( 'NONE',  ( 80.68867513459484542, 150.1262045565065648, -15.00000000000015632 ) ) ;
#25927 = ORIENTED_EDGE ( 'NONE', *, *, #5641, .F. ) ;
#25928 = CARTESIAN_POINT ( 'NONE',  ( -7.984503880673488041, 209.6470497212046098, 9.651137918078566358 ) ) ;
#25929 = CIRCLE ( 'NONE', #24829, 12.99999999999998401 ) ;
#25930 = CARTESIAN_POINT ( 'NONE',  ( 3.753561863808876797, 195.6020594897209719, 94.59886208192145318 ) ) ;
#25931 = CARTESIAN_POINT ( 'NONE',  ( 42.67499999726880588, 141.7447067706911810, 9.630534252274376428 ) ) ;
#25932 = ORIENTED_EDGE ( 'NONE', *, *, #33085, .T. ) ;
#25933 = CARTESIAN_POINT ( 'NONE',  ( 52.22499999726881725, 149.9369285172503510, 15.58253174999999580 ) ) ;
#25934 = DIRECTION ( 'NONE',  ( -1.000000000000000000, -0.000000000000000000, -0.000000000000000000 ) ) ;
#25935 = CARTESIAN_POINT ( 'NONE',  ( -3.135527875058821579, 197.5041725223112223, 5.901137918078566358 ) ) ;
#25936 = CARTESIAN_POINT ( 'NONE',  ( 3.135527875058981895, 197.5041725223112792, 82.59886208192143897 ) ) ;
#25937 = CARTESIAN_POINT ( 'NONE',  ( 45.97499999726881015, 169.8198683612136222, 4.815267126137181997 ) ) ;
#25938 = LINE ( 'NONE', #13162, #909 ) ;
#25939 = CARTESIAN_POINT ( 'NONE',  ( -9.984503880673473830, 210.2968891136704315, 9.651137918078568134 ) ) ;
#25940 = DIRECTION ( 'NONE',  ( 0.000000000000000000, 0.000000000000000000, 1.000000000000000000 ) ) ;
#25941 = CIRCLE ( 'NONE', #3080, 12.10452846326762177 ) ;
#25942 = CARTESIAN_POINT ( 'NONE',  ( 70.50000000000000000, 155.0000000000000000, -14.50000000000000711 ) ) ;
#25943 = CARTESIAN_POINT ( 'NONE',  ( 0.05014649552810505201, 217.5146222423826714, 100.2511379180785838 ) ) ;
#25944 = CARTESIAN_POINT ( 'NONE',  ( 0.000000000000000000, 0.000000000000000000, -18.00000000000000000 ) ) ;
#25945 = CARTESIAN_POINT ( 'NONE',  ( -0.05014649552810635652, 196.4853777576173002, 86.75113791807858377 ) ) ;
#25946 = CARTESIAN_POINT ( 'NONE',  ( 85.98867513459482836, 146.1832212156128890, 12.13525491562421976 ) ) ;
#25947 = LINE ( 'NONE', #33622, #19998 ) ;
#25948 = CARTESIAN_POINT ( 'NONE',  ( 3.753561863808876797, 195.6020594897209719, 100.5988620819214532 ) ) ;
#25949 =( REPRESENTATION_RELATIONSHIP ('NONE','NONE', #25663, #2185 ) REPRESENTATION_RELATIONSHIP_WITH_TRANSFORMATION ( #24007 )SHAPE_REPRESENTATION_RELATIONSHIP( ) );
#25950 = CARTESIAN_POINT ( 'NONE',  ( 68.02499999726882152, 160.0630714827496206, 15.58253174999999402 ) ) ;
#25951 = VERTEX_POINT ( 'NONE', #7294 ) ;
#25952 = DIRECTION ( 'NONE',  ( -0.000000000000000000, -0.000000000000000000, 1.000000000000000000 ) ) ;
#25953 = CARTESIAN_POINT ( 'NONE',  ( 37.79999999453762882, 146.4771138417591203, -11.73074641843674470 ) ) ;
#25954 = CARTESIAN_POINT ( 'NONE',  ( -7.375838497908182134, 217.2372850707499765, 96.95113791807857240 ) ) ;
#25955 = AXIS2_PLACEMENT_3D ( 'NONE', #29052, #21374, #29716 ) ;
#25956 = CARTESIAN_POINT ( 'NONE',  ( -11.00000000000000355, 206.9999999999998863, 103.5000000000000142 ) ) ;
#25957 = ADVANCED_FACE ( 'NONE', ( #30973 ), #17858, .F. ) ;
#25958 = AXIS2_PLACEMENT_3D ( 'NONE', #488, #816, #10886 ) ;
#25959 = ORIENTED_EDGE ( 'NONE', *, *, #4798, .T. ) ;
#25960 = CARTESIAN_POINT ( 'NONE',  ( 9.984503880673420539, 210.2968891136705736, 90.84886208192143897 ) ) ;
#25961 = CARTESIAN_POINT ( 'NONE',  ( 12.01549611932659367, 203.1486557965466773, 19.14886208192143968 ) ) ;
#25962 = CARTESIAN_POINT ( 'NONE',  ( -4.336808689942017736E-14, -31.75426480542944319, -2.456200930618646971 ) ) ;
#25963 = ADVANCED_FACE ( 'NONE', ( #28579 ), #11873, .F. ) ;
#25964 = CARTESIAN_POINT ( 'NONE',  ( -6.220909254589537696, 198.5229672870051161, 45.05113791807855961 ) ) ;
#25965 = ORIENTED_EDGE ( 'NONE', *, *, #7089, .F. ) ;
#25966 = CARTESIAN_POINT ( 'NONE',  ( -6.500168698208244500, 211.6636982574061676, 5.798862081921435596 ) ) ;
#25967 = EDGE_CURVE ( 'NONE', #7879, #29153, #25489, .T. ) ;
#25968 = DIRECTION ( 'NONE',  ( -0.000000000000000000, -0.000000000000000000, 1.000000000000000000 ) ) ;
#25969 = EDGE_LOOP ( 'NONE', ( #4289, #13761 ) ) ;
#25970 = CARTESIAN_POINT ( 'NONE',  ( -6.500168698208244500, 211.6636982574061676, 89.79886208192142760 ) ) ;
#25971 = VERTEX_POINT ( 'NONE', #25507 ) ;
#25972 = CARTESIAN_POINT ( 'NONE',  ( -8.000000000000008882, 207.0476921513413515, 33.50113791807857666 ) ) ;
#25973 = DIRECTION ( 'NONE',  ( 1.000000000000000000, 0.000000000000000000, 0.000000000000000000 ) ) ;
#25974 = VERTEX_POINT ( 'NONE', #14948 ) ;
#25975 = CARTESIAN_POINT ( 'NONE',  ( 89.50000000000001421, 155.0000000000000000, -6.938893903907228378E-15 ) ) ;
#25976 =( BOUNDED_CURVE ( )  B_SPLINE_CURVE ( 2, ( #18397, #11, #28111, #23002, #7847, #30849, #6269, #13772, #24000, #29114, #8664 ),
 .UNSPECIFIED., .F., .T. ) 
 B_SPLINE_CURVE_WITH_KNOTS ( ( 3, 2, 2, 2, 2, 3 ),
 ( 0.3392857142857140795, 0.3428571428571427493, 0.3464285714285713080, 0.3499999999999998113, 0.3535714285714283700, 0.3571428571428569287 ),
 .UNSPECIFIED. ) 
 CURVE ( )  GEOMETRIC_REPRESENTATION_ITEM ( )  RATIONAL_B_SPLINE_CURVE ( ( 1.000000000000001554, 0.9510565162951518658, 1.000000000000000000, 0.9510565162951534202, 1.000000000000000000, 0.9510565162951534202, 1.000000000000000000, 0.9510565162951534202, 1.000000000000000000, 0.9510565162951557516, 0.9999999999999976685 ) ) 
 REPRESENTATION_ITEM ( '' )  );
#25977 = VECTOR ( 'NONE', #6782, 1000.000000000000000 ) ;
#25978 = CARTESIAN_POINT ( 'NONE',  ( 84.32499999726880446, 145.8408176439707802, 12.60653300113718345 ) ) ;
#25979 = EDGE_CURVE ( 'NONE', #32773, #23288, #10273, .T. ) ;
#25980 = DIRECTION ( 'NONE',  ( 0.000000000000000000, 0.000000000000000000, 1.000000000000000000 ) ) ;
#25981 = CARTESIAN_POINT ( 'NONE',  ( -2.426778023690262742, 214.6231898156240163, 85.10113791807857808 ) ) ;
#25982 = CARTESIAN_POINT ( 'NONE',  ( 125.5000000000000000, 48.99999999999998579, -1.387778780781445676E-14 ) ) ;
#25983 = AXIS2_PLACEMENT_3D ( 'NONE', #25167, #6607, #14612 ) ;
#25984 = AXIS2_PLACEMENT_3D ( 'NONE', #3640, #24433, #11821 ) ;
#25985 = CARTESIAN_POINT ( 'NONE',  ( 0.000000000000000000, 0.000000000000000000, 0.000000000000000000 ) ) ;
#25986 = CARTESIAN_POINT ( 'NONE',  ( 51.39999999999999858, 159.7113355953771077, 14.49999999999999289 ) ) ;
#25987 = CARTESIAN_POINT ( 'NONE',  ( -6.444103211790928043, 202.2591342207265939, 62.19886208192144750 ) ) ;
#25988 = DIRECTION ( 'NONE',  ( -1.000000000000000000, -0.000000000000000000, -0.000000000000000000 ) ) ;
#25989 = EDGE_CURVE ( 'NONE', #28893, #33143, #15155, .T. ) ;
#25990 = CIRCLE ( 'NONE', #20538, 32.00000000000005684 ) ;
#25991 = CARTESIAN_POINT ( 'NONE',  ( 52.92499999726881299, 145.8408176439707802, -12.60653300113719588 ) ) ;
#25992 = CARTESIAN_POINT ( 'NONE',  ( -1.750000000000014211, 3.031088913245526317, 0.000000000000000000 ) ) ;
#25993 = DIRECTION ( 'NONE',  ( -1.000000000000000000, 0.000000000000000000, 0.000000000000000000 ) ) ;
#25994 = CARTESIAN_POINT ( 'NONE',  ( 55.02499999726881441, 149.9369285172503510, -15.58253175000000823 ) ) ;
#25995 = CARTESIAN_POINT ( 'NONE',  ( 68.47499999726878173, 149.9369285172503510, 15.58253174999999580 ) ) ;
#25996 = CARTESIAN_POINT ( 'NONE',  ( 11.98450388067348271, 203.0532714938637753, 71.15113791807857524 ) ) ;
#25997 = DIRECTION ( 'NONE',  ( -0.000000000000000000, -0.000000000000000000, -1.000000000000000000 ) ) ;
#25998 = CARTESIAN_POINT ( 'NONE',  ( -12.00000000000000711, 207.0476921513413515, 9.501137918078566003 ) ) ;
#25999 = CARTESIAN_POINT ( 'NONE',  ( -10.00000000000000711, 207.0476921513413515, 90.50113791807858377 ) ) ;
#26000 = EDGE_CURVE ( 'NONE', #7925, #12782, #27886, .T. ) ;
#26001 = FACE_OUTER_BOUND ( 'NONE', #17421, .T. ) ;
#26002 = CARTESIAN_POINT ( 'NONE',  ( 12.01549611932659367, 203.1486557965466773, 55.14886208192143613 ) ) ;
#26003 = CARTESIAN_POINT ( 'NONE',  ( -0.05014649552828402690, 217.5146222423826714, 60.24886208192143044 ) ) ;
#26004 = CARTESIAN_POINT ( 'NONE',  ( -9.680171189290831535, 214.0920067884431148, 93.80113791807858092 ) ) ;
#26005 = DIRECTION ( 'NONE',  ( -0.000000000000000000, -0.000000000000000000, 1.000000000000000000 ) ) ;
#26006 = AXIS2_PLACEMENT_3D ( 'NONE', #21189, #26466, #18639 ) ;
#26007 = CARTESIAN_POINT ( 'NONE',  ( -3.044812012440131443, 216.5253028482142952, 16.10113791807856742 ) ) ;
#26008 = CARTESIAN_POINT ( 'NONE',  ( 3.135527875058981895, 197.5041725223112792, 76.59886208192142476 ) ) ;
#26009 = VERTEX_POINT ( 'NONE', #25335 ) ;
#26010 = CARTESIAN_POINT ( 'NONE',  ( 9.680171189290716072, 214.0920067884432854, 78.69886208192143329 ) ) ;
#26011 = AXIS2_PLACEMENT_3D ( 'NONE', #2147, #20371, #9984 ) ;
#26012 = CARTESIAN_POINT ( 'NONE',  ( -10.00000000000000711, 207.0476921513413515, 102.5011379180785838 ) ) ;
#26013 = ORIENTED_EDGE ( 'NONE', *, *, #27227, .T. ) ;
#26014 = FACE_OUTER_BOUND ( 'NONE', #14809, .T. ) ;
#26015 = CARTESIAN_POINT ( 'NONE',  ( -4.984841277089891776, 213.7757310962905990, 50.94886208192143329 ) ) ;
#26016 = EDGE_LOOP ( 'NONE', ( #31003, #21150, #2729, #14231 ) ) ;
#26017 = ADVANCED_FACE ( 'NONE', ( #2003 ), #28525, .F. ) ;
#26018 = AXIS2_PLACEMENT_3D ( 'NONE', #30137, #22124, #27744 ) ;
#26019 = CARTESIAN_POINT ( 'NONE',  ( 72.92499999726881299, 145.8408176439707802, -12.60653300113719588 ) ) ;
#26020 = DIRECTION ( 'NONE',  ( 0.000000000000000000, 0.000000000000000000, -1.000000000000000000 ) ) ;
#26021 = CARTESIAN_POINT ( 'NONE',  ( 0.000000000000000000, 0.000000000000000000, -18.00000000000000000 ) ) ;
#26022 = CARTESIAN_POINT ( 'NONE',  ( 61.62499999726881583, 171.3844434931184253, -7.942151717890132712E-15 ) ) ;
#26023 = ADVANCED_FACE ( 'NONE', ( #16444 ), #30954, .T. ) ;
#26024 = FILL_AREA_STYLE_COLOUR ( '', #30364 ) ;
#26025 = CARTESIAN_POINT ( 'NONE',  ( -6.139770520408224463, 198.4640165459539389, 53.04886208192142050 ) ) ;
#26026 = VERTEX_POINT ( 'NONE', #5557 ) ;
#26027 = DIRECTION ( 'NONE',  ( 0.000000000000000000, -9.859324684083082301E-16, -1.000000000000000000 ) ) ;
#26028 = CARTESIAN_POINT ( 'NONE',  ( 15.79999999999999538, 0.000000000000000000, -1.540456584061364431 ) ) ;
#26029 = CARTESIAN_POINT ( 'NONE',  ( 4.903702542908435547, 213.8346818373419751, 36.54886208192144892 ) ) ;
#26030 = CONICAL_SURFACE ( 'NONE', #14587, 27.50000000000000355, 1.047197551196595411 ) ;
#26031 = EDGE_CURVE ( 'NONE', #11207, #7326, #27676, .T. ) ;
#26032 = CARTESIAN_POINT ( 'NONE',  ( 9.984503880673470277, 203.7031108863295401, 71.15113791807857524 ) ) ;
#26033 = DIRECTION ( 'NONE',  ( 0.000000000000000000, 0.000000000000000000, -1.000000000000000000 ) ) ;
#26034 = CARTESIAN_POINT ( 'NONE',  ( -0.05014649552810635652, 196.4853777576173002, 59.75113791807857666 ) ) ;
#26035 = AXIS2_PLACEMENT_3D ( 'NONE', #32660, #24495, #3874 ) ;
#26036 = CARTESIAN_POINT ( 'NONE',  ( 3.044812012440130555, 197.4746971517856764, 29.60113791807856742 ) ) ;
#26037 = CARTESIAN_POINT ( 'NONE',  ( 2.426778023690261410, 199.3768101843759837, 17.60113791807856742 ) ) ;
#26038 = CARTESIAN_POINT ( 'NONE',  ( 127.5000000000000000, 155.0000000000000000, 112.0000000000000711 ) ) ;
#26039 = CARTESIAN_POINT ( 'NONE',  ( 92.60208470531341618, 155.0000000000000000, 0.000000000000000000 ) ) ;
#26040 = CARTESIAN_POINT ( 'NONE',  ( 36.42499999726879878, 141.7447067706911810, 9.630534252274376428 ) ) ;
#26041 = CARTESIAN_POINT ( 'NONE',  ( -12.01549611932652972, 203.1486557965464499, 36.35113791807856387 ) ) ;
#26042 = FACE_OUTER_BOUND ( 'NONE', #9533, .T. ) ;
#26043 = CARTESIAN_POINT ( 'NONE',  ( 10.01549611932653860, 210.2015048109876716, 85.85113791807857808 ) ) ;
#26044 = CARTESIAN_POINT ( 'NONE',  ( 9.984503880673473830, 203.7031108863295401, 59.15113791807857524 ) ) ;
#26045 = AXIS2_PLACEMENT_3D ( 'NONE', #19031, #5739, #32137 ) ;
#26046 = CARTESIAN_POINT ( 'NONE',  ( 11.98450388067341876, 210.9467285061363953, 27.84886208192143897 ) ) ;
#26047 = CARTESIAN_POINT ( 'NONE',  ( 6.139770520408223575, 215.5359834540460611, 27.54886208192143471 ) ) ;
#26048 = CARTESIAN_POINT ( 'NONE',  ( 77.29999999453764303, 142.6655632788954620, 8.961492836873471646 ) ) ;
#26049 = CARTESIAN_POINT ( 'NONE',  ( 12.00000000000000711, 206.9523078486586485, 68.00113791807856956 ) ) ;
#26050 = CARTESIAN_POINT ( 'NONE',  ( -8.015496119326531499, 204.4483345814780364, 90.35113791807857808 ) ) ;
#26051 = CARTESIAN_POINT ( 'NONE',  ( -8.118202686958138514, 212.8392687619910930, 50.79886208192143471 ) ) ;
#26052 = DIRECTION ( 'NONE',  ( 0.9945218953682747332, 0.000000000000000000, -0.1045284632676402453 ) ) ;
#26053 = VERTEX_POINT ( 'NONE', #616 ) ;
#26054 = CARTESIAN_POINT ( 'NONE',  ( -12.00000000000000711, 206.9523078486584780, 50.49886208192143044 ) ) ;
#26055 = EDGE_LOOP ( 'NONE', ( #32031, #5519, #5186, #5785 ) ) ;
#26056 = AXIS2_PLACEMENT_3D ( 'NONE', #5079, #15300, #26194 ) ;
#26057 = EDGE_LOOP ( 'NONE', ( #13962, #26669, #5397, #31016 ) ) ;
#26058 = EDGE_CURVE ( 'NONE', #866, #19336, #13826, .T. ) ;
#26059 = DIRECTION ( 'NONE',  ( 1.000000000000000000, 0.000000000000000000, 0.000000000000000000 ) ) ;
#26060 = AXIS2_PLACEMENT_3D ( 'NONE', #27109, #16366, #3927 ) ;
#26061 = CARTESIAN_POINT ( 'NONE',  ( 6.139770520408368348, 198.4640165459539674, 68.45113791807858661 ) ) ;
#26062 = DIRECTION ( 'NONE',  ( 1.000000000000000000, 0.000000000000000000, 0.000000000000000000 ) ) ;
#26063 = ORIENTED_EDGE ( 'NONE', *, *, #19558, .T. ) ;
#26064 = CARTESIAN_POINT ( 'NONE',  ( -7.984503880673488041, 209.6470497212046098, 42.65113791807857524 ) ) ;
#26065 = EDGE_CURVE ( 'NONE', #16785, #3951, #22228, .T. ) ;
#26066 = DIRECTION ( 'NONE',  ( 0.000000000000000000, 0.000000000000000000, -1.000000000000000000 ) ) ;
#26067 = CARTESIAN_POINT ( 'NONE',  ( -3.135527875058982783, 216.4958274776886924, 24.09886208192143542 ) ) ;
#26068 = CARTESIAN_POINT ( 'NONE',  ( 61.97499999726881015, 169.8198683612136222, 4.815267126137181997 ) ) ;
#26070 = ORIENTED_EDGE ( 'NONE', *, *, #24941, .T. ) ;
#26069 = CIRCLE ( 'NONE', #29317, 15.00000000000001776 ) ;
#26071 = DIRECTION ( 'NONE',  ( 0.000000000000000000, 0.000000000000000000, -1.000000000000000000 ) ) ;
#26072 = CARTESIAN_POINT ( 'NONE',  ( -63.49999999999884892, 217.5000000000001990, 0.000000000000000000 ) ) ;
#26073 = CARTESIAN_POINT ( 'NONE',  ( -8.000000000000008882, 206.9523078486584780, 8.498862081921435774 ) ) ;
#26074 = CARTESIAN_POINT ( 'NONE',  ( 8.118202686958039038, 212.8392687619912635, 37.70113791807857240 ) ) ;
#26075 = SURFACE_STYLE_FILL_AREA ( #33569 ) ;
#26076 = CARTESIAN_POINT ( 'NONE',  ( -3.044812012440131443, 216.5253028482142952, 31.10113791807856742 ) ) ;
#26077 = CARTESIAN_POINT ( 'NONE',  ( 3.044812012439969795, 216.5253028482143520, 99.39886208192145034 ) ) ;
#26078 = SHAPE_DEFINITION_REPRESENTATION ( #9999, #30243 ) ;
#26079 = CARTESIAN_POINT ( 'NONE',  ( -6.444103211790928043, 202.2591342207265939, 89.19886208192144750 ) ) ;
#26080 = CARTESIAN_POINT ( 'NONE',  ( 84.70000000000000284, 163.5228861582408797, -11.73074641843674470 ) ) ;
#26081 = DIRECTION ( 'NONE',  ( -0.000000000000000000, -0.000000000000000000, 1.000000000000000000 ) ) ;
#26082 = DIRECTION ( 'NONE',  ( -1.000000000000000000, 0.000000000000000000, 0.000000000000000000 ) ) ;
#26083 = CARTESIAN_POINT ( 'NONE',  ( -0.05014649552807705357, 194.3824533091408000, 14.75113791807856600 ) ) ;
#26084 = CIRCLE ( 'NONE', #3746, 5.000000000000000888 ) ;
#26085 = DIRECTION ( 'NONE',  ( -1.000000000000000000, -0.000000000000000000, -0.000000000000000000 ) ) ;
#26086 = CARTESIAN_POINT ( 'NONE',  ( 58.37499999726881583, 155.0000000000000000, 15.58253174999999402 ) ) ;
#26087 = CARTESIAN_POINT ( 'NONE',  ( -9.984503880673473830, 210.2968891136704315, 54.65113791807858235 ) ) ;
#26088 = CARTESIAN_POINT ( 'NONE',  ( 0.000000000000000000, 0.000000000000000000, 3.100000000000000533 ) ) ;
#26089 = CARTESIAN_POINT ( 'NONE',  ( -64.50000000000000000, -2.605762844159085212, 20.00000000000000000 ) ) ;
#26090 = CARTESIAN_POINT ( 'NONE',  ( 32.50000000000000000, 155.0000000000000000, -6.938893903907228378E-15 ) ) ;
#26091 = CARTESIAN_POINT ( 'NONE',  ( 59.69999999453762030, 142.6655632788954620, -8.961492836873480528 ) ) ;
#26092 = ORIENTED_EDGE ( 'NONE', *, *, #8640, .F. ) ;
#26093 = CARTESIAN_POINT ( 'NONE',  ( -3.662846001190052991, 218.4274158808045740, 37.10113791807855677 ) ) ;
#26094 = DIRECTION ( 'NONE',  ( 0.000000000000000000, -1.000000000000000000, 1.222984857324291014E-15 ) ) ;
#26095 = UNCERTAINTY_MEASURE_WITH_UNIT (LENGTH_MEASURE( 1.000000000000000082E-05 ), #20578, 'distance_accuracy_value', 'NONE');
#26096 = CARTESIAN_POINT ( 'NONE',  ( 3.044812012439969795, 216.5253028482143520, 12.39886208192143435 ) ) ;
#26097 = DIRECTION ( 'NONE',  ( -1.000000000000000000, 0.000000000000000000, 0.000000000000000000 ) ) ;
#26098 = ORIENTED_EDGE ( 'NONE', *, *, #11870, .T. ) ;
#26099 = CARTESIAN_POINT ( 'NONE',  ( -6.220909254589537696, 198.5229672870051161, 75.05113791807858092 ) ) ;
#26100 = ORIENTED_EDGE ( 'NONE', *, *, #21789, .F. ) ;
#26101 = CARTESIAN_POINT ( 'NONE',  ( -8.015496119326597224, 209.5516654185217362, 32.64886208192144323 ) ) ;
#26102 = CARTESIAN_POINT ( 'NONE',  ( 117.5000000000000000, 182.4348187808683690, 102.3881375866409513 ) ) ;
#26103 = ORIENTED_EDGE ( 'NONE', *, *, #18695, .F. ) ;
#26104 = CARTESIAN_POINT ( 'NONE',  ( 2.426778023690261410, 199.3768101843759837, 11.60113791807856742 ) ) ;
#26105 = AXIS2_PLACEMENT_3D ( 'NONE', #5132, #7362, #9911 ) ;
#26106 = CARTESIAN_POINT ( 'NONE',  ( 3.662846001189864698, 218.4274158808046593, 96.39886208192146455 ) ) ;
#26107 = CARTESIAN_POINT ( 'NONE',  ( 43.77499999726881441, 169.8198683612136222, -4.815267126137197984 ) ) ;
#26108 = ORIENTED_EDGE ( 'NONE', *, *, #22802, .T. ) ;
#26109 = CARTESIAN_POINT ( 'NONE',  ( 48.22499999726880304, 149.9369285172503510, 15.58253174999999580 ) ) ;
#26110 = CARTESIAN_POINT ( 'NONE',  ( 7.499999999999999112, 0.3744244963005059490, 1.526918059583750369E-15 ) ) ;
#26111 = CARTESIAN_POINT ( 'NONE',  ( -8.118202686958039038, 201.1607312380087080, 12.20113791807856707 ) ) ;
#26112 = CARTESIAN_POINT ( 'NONE',  ( -9.984503880673420539, 203.7031108863293980, 77.34886208192142476 ) ) ;
#26113 = CARTESIAN_POINT ( 'NONE',  ( 53.67499999726879878, 168.2552932293087906, -9.630534252274385310 ) ) ;
#26114 = CARTESIAN_POINT ( 'NONE',  ( 79.41132485994285162, 142.2402378747194405, -9.270509831248439525 ) ) ;
#26115 = CARTESIAN_POINT ( 'NONE',  ( 9.984503880673470277, 203.7031108863295401, 17.15113791807856103 ) ) ;
#26116 = CARTESIAN_POINT ( 'NONE',  ( 44.08867513459483689, 142.2402378747194405, 9.270509831248432420 ) ) ;
#26117 = CARTESIAN_POINT ( 'NONE',  ( 65.70000000000000284, 146.4771138417591203, 11.73074641843673227 ) ) ;
#26118 = FACE_OUTER_BOUND ( 'NONE', #7869, .T. ) ;
#26119 = DIRECTION ( 'NONE',  ( 0.9945218953682747332, 1.280104479605073142E-17, 0.1045284632676402453 ) ) ;
#26120 = CARTESIAN_POINT ( 'NONE',  ( 8.062137200540920645, 201.0835637161417822, 83.30113791807858092 ) ) ;
#26121 = CARTESIAN_POINT ( 'NONE',  ( -125.0000000000000000, -25.00000000000000000, 35.00000000000000000 ) ) ;
#26122 = CARTESIAN_POINT ( 'NONE',  ( 38.97499999726881015, 140.1801316387863778, -4.815267126137194431 ) ) ;
#26123 = CARTESIAN_POINT ( 'NONE',  ( 11.98450388067341876, 210.9467285061363953, 93.84886208192143897 ) ) ;
#26124 = CARTESIAN_POINT ( 'NONE',  ( 71.22499999726879594, 160.0630714827496206, -15.58253175000000823 ) ) ;
#26125 = ORIENTED_EDGE ( 'NONE', *, *, #11256, .F. ) ;
#26126 = CARTESIAN_POINT ( 'NONE',  ( 43.51132485994280330, 146.1832212156128890, -12.13525491562423042 ) ) ;
#26127 = CARTESIAN_POINT ( 'NONE',  ( 36.09999999453761887, 159.7113355953771077, -14.50000000000000888 ) ) ;
#26128 = CARTESIAN_POINT ( 'NONE',  ( -12.00000000000000711, 207.0476921513413515, 96.50113791807856956 ) ) ;
#26129 =( BOUNDED_CURVE ( )  B_SPLINE_CURVE ( 2, ( #8040, #19085, #533, #28817, #21302, #359, #21636, #15861, #8206, #11093, #31696 ),
 .UNSPECIFIED., .F., .F. ) 
 B_SPLINE_CURVE_WITH_KNOTS ( ( 3, 2, 2, 2, 2, 3 ),
 ( 0.2857142857142854209, 0.2892857142857139796, 0.2928571428571425939, 0.2964285714285711526, 0.2999999999999997669, 0.3035714285714283256 ),
 .UNSPECIFIED. ) 
 CURVE ( )  GEOMETRIC_REPRESENTATION_ITEM ( )  RATIONAL_B_SPLINE_CURVE ( ( 1.000000000000003775, 0.9510565162951496454, 1.000000000000000000, 0.9510565162951534202, 1.000000000000000000, 0.9510565162951534202, 1.000000000000000000, 0.9510565162951534202, 1.000000000000000000, 0.9510565162951557516, 0.9999999999999976685 ) ) 
 REPRESENTATION_ITEM ( '' )  );
#26130 = CARTESIAN_POINT ( 'NONE',  ( 115.4999999999999858, 207.9999999999998010, -89.64869280115067340 ) ) ;
#26131 = VERTEX_POINT ( 'NONE', #8134 ) ;
#26132 = CARTESIAN_POINT ( 'NONE',  ( 10.00000000000000711, 207.0476921513415220, 81.99886208192143044 ) ) ;
#26133 = CARTESIAN_POINT ( 'NONE',  ( 12.01549611932659367, 203.1486557965466773, 25.14886208192143258 ) ) ;
#26134 = CARTESIAN_POINT ( 'NONE',  ( -7.922281120364393914, -4.573931137438277617, -8.047472243342932430 ) ) ;
#26135 = CARTESIAN_POINT ( 'NONE',  ( -9.984503880673473830, 210.2968891136704315, 39.65113791807857524 ) ) ;
#26136 = ORIENTED_EDGE ( 'NONE', *, *, #15621, .T. ) ;
#26137 = CARTESIAN_POINT ( 'NONE',  ( 0.05014649552828262524, 198.5883022060938572, 7.748862081921434886 ) ) ;
#26138 = CARTESIAN_POINT ( 'NONE',  ( 74.31132485994281467, 169.2658477444273331, 4.635254915624208216 ) ) ;
#26139 = ORIENTED_EDGE ( 'NONE', *, *, #12320, .T. ) ;
#26140 = CARTESIAN_POINT ( 'NONE',  ( -2.426778023690076225, 199.3768101843759553, 91.89886208192143613 ) ) ;
#26141 = CARTESIAN_POINT ( 'NONE',  ( -6.500168698208129925, 202.3363017425936050, 30.20113791807856529 ) ) ;
#26142 = CARTESIAN_POINT ( 'NONE',  ( 58.50000000000001421, -88.00000000000000000, -30.00000000000000000 ) ) ;
#26143 = ORIENTED_EDGE ( 'NONE', *, *, #7663, .T. ) ;
#26144 = CARTESIAN_POINT ( 'NONE',  ( 3.295171437449806451, 7.213553046161976567, -7.590212325761626744 ) ) ;
#26145 = CARTESIAN_POINT ( 'NONE',  ( 37.47499999726880304, 160.0630714827496206, -15.58253175000000823 ) ) ;
#26146 = CARTESIAN_POINT ( 'NONE',  ( 125.5000000000000000, 48.99999999999998579, -1.387778780781445676E-14 ) ) ;
#26147 = CARTESIAN_POINT ( 'NONE',  ( 8.015496119326531499, 209.5516654185219636, 91.85113791807857808 ) ) ;
#26148 = EDGE_CURVE ( 'NONE', #17290, #22749, #26842, .T. ) ;
#26149 = DIRECTION ( 'NONE',  ( 0.000000000000000000, 0.000000000000000000, -1.000000000000000000 ) ) ;
#26150 = CARTESIAN_POINT ( 'NONE',  ( 47.60000000000000853, 150.2886644046228639, 14.49999999999999645 ) ) ;
#26151 = CARTESIAN_POINT ( 'NONE',  ( 4.903702542908435547, 213.8346818373419751, 66.54886208192144181 ) ) ;
#26152 = CARTESIAN_POINT ( 'NONE',  ( 27.50000000000000000, -9.324699302609159801, -0.8718021930569386235 ) ) ;
#26153 = CIRCLE ( 'NONE', #642, 2.500000000000000000 ) ;
#26154 = CARTESIAN_POINT ( 'NONE',  ( 48.42499999726881299, 141.7447067706911810, 9.630534252274376428 ) ) ;
#26155 = CARTESIAN_POINT ( 'NONE',  ( 6.139770520408367460, 198.4640165459539389, 5.451137918078566180 ) ) ;
#26156 = CARTESIAN_POINT ( 'NONE',  ( 102.4138169258850581, 155.0000000000000000, 0.000000000000000000 ) ) ;
#26157 = CARTESIAN_POINT ( 'NONE',  ( 65.02499999726882152, 149.9369285172503510, -15.58253175000000823 ) ) ;
#26158 = CARTESIAN_POINT ( 'NONE',  ( 69.67499999726878457, 168.2552932293087906, -9.630534252274385310 ) ) ;
#26159 = CARTESIAN_POINT ( 'NONE',  ( -9.736236675707914401, 199.9851607334237542, 69.20113791807857240 ) ) ;
#26160 = DIRECTION ( 'NONE',  ( 0.000000000000000000, 1.000000000000000000, 0.000000000000000000 ) ) ;
#26161 = CARTESIAN_POINT ( 'NONE',  ( -8.118202686958039038, 201.1607312380087080, 87.20113791807858661 ) ) ;
#26162 = CARTESIAN_POINT ( 'NONE',  ( 7.456977232089471386, 196.8216656703012006, 52.44886208192144039 ) ) ;
#26163 = CARTESIAN_POINT ( 'NONE',  ( 9.984503880673420539, 210.2968891136705736, 57.84886208192143897 ) ) ;
#26164 = CARTESIAN_POINT ( 'NONE',  ( 3.662846001190051659, 195.5725841191953691, 98.60113791807857808 ) ) ;
#26165 = CARTESIAN_POINT ( 'NONE',  ( 68.61132485994279762, 159.8737954434937478, 14.99999999999991651 ) ) ;
#26166 = CARTESIAN_POINT ( 'NONE',  ( 10.00000000000000711, 206.9523078486586201, 17.00113791807856600 ) ) ;
#26167 = CARTESIAN_POINT ( 'NONE',  ( 9.984503880673420539, 210.2968891136705167, 75.84886208192143897 ) ) ;
#26168 = VERTEX_POINT ( 'NONE', #19015 ) ;
#26169 = CARTESIAN_POINT ( 'NONE',  ( 7.456977232089471386, 196.8216656703012006, 76.44886208192143329 ) ) ;
#26170 = CARTESIAN_POINT ( 'NONE',  ( -6.220909254589537696, 198.5229672870051161, 99.05113791807858092 ) ) ;
#26171 = EDGE_LOOP ( 'NONE', ( #31249, #20949, #17966, #4421 ) ) ;
#26172 = CARTESIAN_POINT ( 'NONE',  ( -2.517493886309087880, 214.5937144450984135, 66.09886208192142476 ) ) ;
#26173 = EDGE_CURVE ( 'NONE', #6985, #28362, #26346, .T. ) ;
#26174 = ORIENTED_EDGE ( 'NONE', *, *, #12482, .F. ) ;
#26175 = CARTESIAN_POINT ( 'NONE',  ( 77.92499999726881299, 164.1591823560292198, 12.60653300113718167 ) ) ;
#26176 = DIRECTION ( 'NONE',  ( 0.000000000000000000, -0.5000000000000009992, -0.8660254037844380415 ) ) ;
#26177 = CARTESIAN_POINT ( 'NONE',  ( -57.85233474027615586, 194.9267265987278961, -2.420233332361308332 ) ) ;
#26178 = CIRCLE ( 'NONE', #11493, 2.149999999999974598 ) ;
#26179 = CARTESIAN_POINT ( 'NONE',  ( 63.22499999726881725, 160.0630714827496206, -15.58253175000000823 ) ) ;
#26180 = CARTESIAN_POINT ( 'NONE',  ( 7.984503880673485376, 204.3529502787953902, 59.15113791807857524 ) ) ;
#26181 = LINE ( 'NONE', #26352, #2057 ) ;
#26182 = ADVANCED_FACE ( 'NONE', ( #24120 ), #21397, .T. ) ;
#26183 = CARTESIAN_POINT ( 'NONE',  ( -10.01549611932659722, 210.2015048109875011, 47.64886208192142192 ) ) ;
#26184 = PLANE ( 'NONE',  #15099 ) ;
#26185 = DIRECTION ( 'NONE',  ( -0.000000000000000000, -0.000000000000000000, 1.000000000000000000 ) ) ;
#26186 = CARTESIAN_POINT ( 'NONE',  ( -6.444103211790928043, 202.2591342207265939, 38.19886208192144750 ) ) ;
#26187 = CARTESIAN_POINT ( 'NONE',  ( 6.220909254589536808, 215.4770327129947702, 79.55113791807855250 ) ) ;
#26188 = FACE_BOUND ( 'NONE', #17715, .T. ) ;
#26189 = CARTESIAN_POINT ( 'NONE',  ( 0.05014649552810505201, 217.5146222423826714, 55.25113791807858377 ) ) ;
#26190 =( REPRESENTATION_RELATIONSHIP ('NONE','NONE', #25663, #18505 ) REPRESENTATION_RELATIONSHIP_WITH_TRANSFORMATION ( #25177 )SHAPE_REPRESENTATION_RELATIONSHIP( ) );
#26191 = EDGE_CURVE ( 'NONE', #15536, #9440, #24960, .T. ) ;
#26192 = CARTESIAN_POINT ( 'NONE',  ( -10.01549611932653860, 203.7984951890123284, 27.35113791807856742 ) ) ;
#26193 = CARTESIAN_POINT ( 'NONE',  ( 6.444103211791042618, 202.2591342207267644, 14.30113791807856849 ) ) ;
#26194 = DIRECTION ( 'NONE',  ( 0.000000000000000000, 0.000000000000000000, -1.000000000000000000 ) ) ;
#26195 = DIRECTION ( 'NONE',  ( -1.000000000000000000, -0.000000000000000000, -0.000000000000000000 ) ) ;
#26196 = CARTESIAN_POINT ( 'NONE',  ( 35.12499999726881583, 155.0000000000000000, -15.58253175000000823 ) ) ;
#26197 = CARTESIAN_POINT ( 'NONE',  ( 7.456977232089302632, 217.1783343296989131, 43.55113791807857382 ) ) ;
#26198 = CARTESIAN_POINT ( 'NONE',  ( 2.263183130831067924, -6.566419505188284766, -6.208110906918261840 ) ) ;
#26199 = CARTESIAN_POINT ( 'NONE',  ( -3.135527875058821579, 197.5041725223112223, 83.90113791807857524 ) ) ;
#26200 = CARTESIAN_POINT ( 'NONE',  ( 3.044812012440130555, 197.4746971517856764, 56.60113791807857098 ) ) ;
#26201 = CARTESIAN_POINT ( 'NONE',  ( 11.98450388067341876, 210.9467285061363953, 24.84886208192143897 ) ) ;
#26202 = CARTESIAN_POINT ( 'NONE',  ( 0.05014649552828275014, 196.4853777576173002, 28.74886208192144110 ) ) ;
#26203 = CONICAL_SURFACE ( 'NONE', #12044, 27.50000000000000355, 1.047197551196595411 ) ;
#26204 = CARTESIAN_POINT ( 'NONE',  ( 76.69999999453764872, 167.3344367211045096, 8.961492836873468093 ) ) ;
#26205 = CARTESIAN_POINT ( 'NONE',  ( -7.456977232089304408, 196.8216656703010301, 66.05113791807858092 ) ) ;
#26206 = CARTESIAN_POINT ( 'NONE',  ( -8.000000000000008882, 207.0476921513413515, 84.50113791807856956 ) ) ;
#26207 = EDGE_CURVE ( 'NONE', #17836, #30105, #1560, .T. ) ;
#26208 = CARTESIAN_POINT ( 'NONE',  ( 8.062137200540822946, 212.9164362838583315, 51.69886208192143329 ) ) ;
#26209 = DIRECTION ( 'NONE',  ( 1.000000000000000000, 0.000000000000000000, -0.000000000000000000 ) ) ;
#26210 = ORIENTED_EDGE ( 'NONE', *, *, #3735, .F. ) ;
#26211 = CARTESIAN_POINT ( 'NONE',  ( -3.662846001189865142, 195.5725841191952838, 49.89886208192143613 ) ) ;
#26212 = AXIS2_PLACEMENT_3D ( 'NONE', #22032, #15708, #28660 ) ;
#26213 = ORIENTED_EDGE ( 'NONE', *, *, #11870, .F. ) ;
#26214 = ORIENTED_EDGE ( 'NONE', *, *, #10168, .T. ) ;
#26215 = DIRECTION ( 'NONE',  ( 0.000000000000000000, -0.5000000000000013323, -0.8660254037844379305 ) ) ;
#26216 = CARTESIAN_POINT ( 'NONE',  ( 56.58867513459482979, 146.1832212156128890, -12.13525491562423042 ) ) ;
#26217 = CARTESIAN_POINT ( 'NONE',  ( 2.426778023690261410, 199.3768101843759837, 38.60113791807857098 ) ) ;
#26218 = SURFACE_SIDE_STYLE ('',( #25719 ) ) ;
#26219 = CARTESIAN_POINT ( 'NONE',  ( -6.139770520408224463, 198.4640165459539389, 26.04886208192143471 ) ) ;
#26220 = CARTESIAN_POINT ( 'NONE',  ( 62.07499999726881157, 168.2552932293087906, 9.630534252274372875 ) ) ;
#26221 = ORIENTED_EDGE ( 'NONE', *, *, #6663, .T. ) ;
#26222 = PLANE ( 'NONE',  #7507 ) ;
#26223 = CARTESIAN_POINT ( 'NONE',  ( -6.602753909532903975, -5.319290460493544259, -7.792447862505333056 ) ) ;
#26224 = CARTESIAN_POINT ( 'NONE',  ( 8.000000000000008882, 207.0476921513415220, 9.998862081921435774 ) ) ;
#26225 = CARTESIAN_POINT ( 'NONE',  ( 6.220909254589536808, 215.4770327129947702, 55.55113791807855961 ) ) ;
#26226 = DIRECTION ( 'NONE',  ( 0.000000000000000000, 0.000000000000000000, 1.000000000000000000 ) ) ;
#26227 = CARTESIAN_POINT ( 'NONE',  ( 10.00000000000000711, 206.9523078486586201, 32.00113791807856956 ) ) ;
#26228 = DIRECTION ( 'NONE',  ( 0.000000000000000000, -0.9988620819214357738, -0.04769215134144155765 ) ) ;
#26229 = SHAPE_DEFINITION_REPRESENTATION ( #6421, #30038 ) ;
#26230 = CARTESIAN_POINT ( 'NONE',  ( 4.984841277089891776, 200.2242689037093726, 88.44886208192144750 ) ) ;
#26231 = VECTOR ( 'NONE', #11269, 1000.000000000000000 ) ;
#26232 = CARTESIAN_POINT ( 'NONE',  ( 39.32499999726881157, 164.1591823560292198, -12.60653300113719766 ) ) ;
#26233 = DIRECTION ( 'NONE',  ( -1.000000000000000000, -0.000000000000000000, -0.000000000000000000 ) ) ;
#26234 = CARTESIAN_POINT ( 'NONE',  ( -18.40606158072672116, 21.12752019707600937, -17.76591125084755873 ) ) ;
#26235 = CARTESIAN_POINT ( 'NONE',  ( 3.753561863808689836, 218.3979405102790565, 7.401137918078566358 ) ) ;
#26236 = CARTESIAN_POINT ( 'NONE',  ( 78.00000000000001421, 3.309499999999999886, 0.000000000000000000 ) ) ;
#26237 = CARTESIAN_POINT ( 'NONE',  ( 54.17499999726881299, 164.1591823560292198, 12.60653300113718167 ) ) ;
#26238 = ADVANCED_FACE ( 'NONE', ( #787 ), #23336, .T. ) ;
#26239 = CARTESIAN_POINT ( 'NONE',  ( -8.118202686958039038, 201.1607312380087080, 57.20113791807857950 ) ) ;
#26240 = EDGE_CURVE ( 'NONE', #5848, #2476, #28901, .T. ) ;
#26241 = CARTESIAN_POINT ( 'NONE',  ( 10.01549611932653860, 210.2015048109876716, 31.85113791807857453 ) ) ;
#26242 = CARTESIAN_POINT ( 'NONE',  ( 35.21132485994281325, 139.2280666364260071, -4.041636747397287284E-15 ) ) ;
#26243 = CARTESIAN_POINT ( 'NONE',  ( 55.58867513459482268, 163.8167787843871110, 12.13525491562421621 ) ) ;
#26244 = CARTESIAN_POINT ( 'NONE',  ( 0.000000000000000000, 0.000000000000000000, 6.099999999999999645 ) ) ;
#26245 = CARTESIAN_POINT ( 'NONE',  ( 60.79999999453762882, 163.5228861582408797, 11.73074641843673049 ) ) ;
#26246 = EDGE_LOOP ( 'NONE', ( #5833, #10775 ) ) ;
#26247 = CARTESIAN_POINT ( 'NONE',  ( -3.662846001190052991, 218.4274158808045740, 43.10113791807857098 ) ) ;
#26248 = PRODUCT_RELATED_PRODUCT_CATEGORY ( 'part', '', ( #28508 ) ) ;
#26249 = ADVANCED_FACE ( 'NONE', ( #31624 ), #8291, .T. ) ;
#26250 = CARTESIAN_POINT ( 'NONE',  ( 77.61132485994281183, 150.1262045565064227, -15.00000000000002665 ) ) ;
#26251 = CARTESIAN_POINT ( 'NONE',  ( -9.984503880673420539, 203.7031108863293980, 17.34886208192143542 ) ) ;
#26252 = CARTESIAN_POINT ( 'NONE',  ( 59.41132485994281609, 142.2402378747194405, -9.270509831248439525 ) ) ;
#26253 = EDGE_LOOP ( 'NONE', ( #17586, #31910, #454, #20621 ) ) ;
#26254 = PRODUCT_DEFINITION_FORMATION_WITH_SPECIFIED_SOURCE ( 'ANY', '', #9707, .NOT_KNOWN. ) ;
#26255 = ADVANCED_BREP_SHAPE_REPRESENTATION ( '', ( #12730, #2404 ), #11614 ) ;
#26256 = CARTESIAN_POINT ( 'NONE',  ( 6.220909254589536808, 215.4770327129947702, 70.55113791807856671 ) ) ;
#26257 = EDGE_CURVE ( 'NONE', #10430, #25798, #11180, .T. ) ;
#26258 = EDGE_LOOP ( 'NONE', ( #16382, #15748 ) ) ;
#26259 = CARTESIAN_POINT ( 'NONE',  ( -9.093938419273312590, -26.50387701106812344, -17.76591125084755163 ) ) ;
#26260 = CARTESIAN_POINT ( 'NONE',  ( -4.336808689942017736E-14, -31.75426480542944319, -15.54379906938135214 ) ) ;
#26261 = ORIENTED_EDGE ( 'NONE', *, *, #19384, .T. ) ;
#26262 = VECTOR ( 'NONE', #33120, 1000.000000000000000 ) ;
#26263 = CARTESIAN_POINT ( 'NONE',  ( -2.426778023690262742, 214.6231898156240163, 13.10113791807856742 ) ) ;
#26264 = CIRCLE ( 'NONE', #8295, 32.00000000000002842 ) ;
#26265 = CARTESIAN_POINT ( 'NONE',  ( -0.05014649552828442242, 219.6175466908591716, 96.24886208192144466 ) ) ;
#26266 = CARTESIAN_POINT ( 'NONE',  ( 45.17499999726881299, 145.8408176439707802, -12.60653300113719588 ) ) ;
#26267 = ORIENTED_EDGE ( 'NONE', *, *, #12476, .F. ) ;
#26268 = CARTESIAN_POINT ( 'NONE',  ( 49.72499999726881725, 169.8198683612136222, 4.815267126137181997 ) ) ;
#26269 = PLANE ( 'NONE',  #8293 ) ;
#26270 = CARTESIAN_POINT ( 'NONE',  ( 8.062137200540920645, 201.0835637161417822, 8.301137918078566713 ) ) ;
#26271 = CARTESIAN_POINT ( 'NONE',  ( 8.118202686958138514, 201.1607312380088501, 79.29886208192144181 ) ) ;
#26272 = CARTESIAN_POINT ( 'NONE',  ( 50.57499999726881157, 145.8408176439707802, 12.60653300113718345 ) ) ;
#26273 = CARTESIAN_POINT ( 'NONE',  ( 52.28867513459482552, 139.2280666364260071, -4.041636747397287284E-15 ) ) ;
#26274 = CARTESIAN_POINT ( 'NONE',  ( 9.984503880673470277, 203.7031108863295401, 14.15113791807856458 ) ) ;
#26275 = CARTESIAN_POINT ( 'NONE',  ( 125.5000000000000000, 78.52640161467446944, -73.43303922622258995 ) ) ;
#26276 = CIRCLE ( 'NONE', #18113, 1.000000000000000000 ) ;
#26277 = CARTESIAN_POINT ( 'NONE',  ( 68.50000000000000000, 155.0000000000000000, -14.50000000000000711 ) ) ;
#26278 = CARTESIAN_POINT ( 'NONE',  ( -6.220909254589537696, 198.5229672870051161, 96.05113791807858092 ) ) ;
#26279 = CARTESIAN_POINT ( 'NONE',  ( -6.139770520408369237, 215.5359834540460042, 87.95113791807858661 ) ) ;
#26280 = LINE ( 'NONE', #18283, #22705 ) ;
#26281 = CARTESIAN_POINT ( 'NONE',  ( 40.07499999726879736, 168.2552932293087906, 9.630534252274372875 ) ) ;
#26282 = CARTESIAN_POINT ( 'NONE',  ( -3.753561863808878130, 218.3979405102790281, 99.09886208192145318 ) ) ;
#26283 = CARTESIAN_POINT ( 'NONE',  ( 68.52499999726880731, 140.1801316387863778, 4.815267126137185549 ) ) ;
#26284 = ORIENTED_EDGE ( 'NONE', *, *, #3748, .F. ) ;
#26285 = CARTESIAN_POINT ( 'NONE',  ( 0.000000000000000000, 0.000000000000000000, 0.000000000000000000 ) ) ;
#26286 = VECTOR ( 'NONE', #10783, 1000.000000000000000 ) ;
#26287 = CARTESIAN_POINT ( 'NONE',  ( 43.69999999453763451, 142.6655632788954620, -8.961492836873480528 ) ) ;
#26288 = CARTESIAN_POINT ( 'NONE',  ( 9.680171189290831535, 199.9079932115568852, 101.3011379180785951 ) ) ;
#26289 = AXIS2_PLACEMENT_3D ( 'NONE', #10678, #18671, #29063 ) ;
#26290 = LINE ( 'NONE', #29014, #1209 ) ;
#26291 = AXIS2_PLACEMENT_3D ( 'NONE', #1831, #22611, #32998 ) ;
#26292 = ORIENTED_EDGE ( 'NONE', *, *, #4756, .F. ) ;
#26293 = CARTESIAN_POINT ( 'NONE',  ( 6.220909254589680693, 198.5229672870052582, 97.44886208192143329 ) ) ;
#26294 = CARTESIAN_POINT ( 'NONE',  ( -12.00000000000000711, 206.9523078486584780, 29.49886208192143400 ) ) ;
#26295 = CARTESIAN_POINT ( 'NONE',  ( -58.50000000000002132, 194.9217985566782829, 2.500000000000000000 ) ) ;
#26296 = CARTESIAN_POINT ( 'NONE',  ( 6.139770520408368348, 198.4640165459539674, 44.45113791807855819 ) ) ;
#26297 = EDGE_LOOP ( 'NONE', ( #6781, #14853, #33455, #28099, #7196 ) ) ;
#26298 = CARTESIAN_POINT ( 'NONE',  ( -9.984503880673420539, 203.7031108863293980, 104.3488620819214105 ) ) ;
#26299 = AXIS2_PLACEMENT_3D ( 'NONE', #22754, #17639, #20190 ) ;
#26300 = DIRECTION ( 'NONE',  ( 0.5000000000000003331, -0.8660254037844384856, 0.000000000000000000 ) ) ;
#26301 = ORIENTED_EDGE ( 'NONE', *, *, #29585, .T. ) ;
#26303 = CARTESIAN_POINT ( 'NONE',  ( 6.500168698208244500, 202.3363017425938324, 94.29886208192142760 ) ) ;
#26302 = MECHANICAL_DESIGN_GEOMETRIC_PRESENTATION_REPRESENTATION (  '', ( #663 ), #24128 ) ;
#26304 = CARTESIAN_POINT ( 'NONE',  ( 7.984503880673485376, 204.3529502787953902, 26.15113791807857169 ) ) ;
#26305 = DIRECTION ( 'NONE',  ( -0.000000000000000000, -0.000000000000000000, -1.000000000000000000 ) ) ;
#26306 = EDGE_LOOP ( 'NONE', ( #19374, #15780, #12437, #24368 ) ) ;
#26307 = CARTESIAN_POINT ( 'NONE',  ( 33.42499999726881299, 168.2552932293087906, -9.630534252274385310 ) ) ;
#26308 = STYLED_ITEM ( 'NONE', ( #12612 ), #11883 ) ;
#26309 = VECTOR ( 'NONE', #2432, 1000.000000000000000 ) ;
#26310 = CARTESIAN_POINT ( 'NONE',  ( 86.02499999726880731, 160.0630714827496206, 15.58253174999999402 ) ) ;
#26311 = CARTESIAN_POINT ( 'NONE',  ( -63.50000000000004263, 215.0000000000000000, 0.000000000000000000 ) ) ;
#26312 = CARTESIAN_POINT ( 'NONE',  ( -8.000000000000008882, 207.0476921513413515, 87.50113791807856956 ) ) ;
#26313 = VECTOR ( 'NONE', #14007, 1000.000000000000000 ) ;
#26314 = DIRECTION ( 'NONE',  ( -1.000000000000000000, 0.000000000000000000, 0.000000000000000000 ) ) ;
#26315 = CARTESIAN_POINT ( 'NONE',  ( 45.99999999999999289, 139.7537977485451393, -4.138211985947621020E-15 ) ) ;
#26316 = CARTESIAN_POINT ( 'NONE',  ( 2.517493886309087436, 199.4062855549015865, 61.59886208192145318 ) ) ;
#26317 = LINE ( 'NONE', #2659, #11833 ) ;
#26318 =( BOUNDED_CURVE ( )  B_SPLINE_CURVE ( 2, ( #20606, #17536, #12591, #10058, #5096, #27923, #4597, #17880, #5260, #14982, #7664 ),
 .UNSPECIFIED., .F., .T. ) 
 B_SPLINE_CURVE_WITH_KNOTS ( ( 3, 2, 2, 2, 2, 3 ),
 ( 0.7321428571428570953, 0.7357142857142857650, 0.7392857142857143238, 0.7428571428571428825, 0.7464285714285714413, 0.7500000000000000000 ),
 .UNSPECIFIED. ) 
 CURVE ( )  GEOMETRIC_REPRESENTATION_ITEM ( )  RATIONAL_B_SPLINE_CURVE ( ( 1.000000000000000000, 0.9510565162951534202, 1.000000000000000000, 0.9510565162951534202, 1.000000000000000000, 0.9510565162951534202, 1.000000000000000000, 0.9510565162951534202, 1.000000000000000000, 0.9510565162951534202, 1.000000000000000000 ) ) 
 REPRESENTATION_ITEM ( '' )  );
#26319 = CARTESIAN_POINT ( 'NONE',  ( 49.02499999726880731, 149.9369285172503510, -15.58253175000000823 ) ) ;
#26321 = ORIENTED_EDGE ( 'NONE', *, *, #19981, .F. ) ;
#26320 = CARTESIAN_POINT ( 'NONE',  ( -8.118202686958039038, 201.1607312380087080, 15.20113791807856884 ) ) ;
#26322 = LINE ( 'NONE', #26981, #28242 ) ;
#26323 = CARTESIAN_POINT ( 'NONE',  ( 62.62499999726880873, 138.6155565068815747, -3.929120461958505118E-15 ) ) ;
#26324 = CARTESIAN_POINT ( 'NONE',  ( 79.37499999726881583, 155.0000000000000000, -15.58253175000000823 ) ) ;
#26325 = CARTESIAN_POINT ( 'NONE',  ( 9.736236675707914401, 214.0148392665762458, 73.70113791807857240 ) ) ;
#26326 = CARTESIAN_POINT ( 'NONE',  ( 16.00000000000000000, 0.000000000000000000, 0.000000000000000000 ) ) ;
#26327 = CARTESIAN_POINT ( 'NONE',  ( 6.220909254589536808, 215.4770327129947987, 88.55113791807855250 ) ) ;
#26328 = DIRECTION ( 'NONE',  ( -0.1461455375466716444, 0.9854922318508084755, -0.08629335326029916042 ) ) ;
#26329 = VERTEX_POINT ( 'NONE', #16109 ) ;
#26330 = CARTESIAN_POINT ( 'NONE',  ( 3.753561863808876797, 195.6020594897209719, 55.59886208192143897 ) ) ;
#26331 = CARTESIAN_POINT ( 'NONE',  ( 3.135527875058981895, 197.5041725223112792, 70.59886208192143897 ) ) ;
#26332 = CARTESIAN_POINT ( 'NONE',  ( 11.98450388067348271, 203.0532714938637753, 92.15113791807856103 ) ) ;
#26333 = CARTESIAN_POINT ( 'NONE',  ( 34.78867513459482552, 155.0000000000000000, -15.00000000000002487 ) ) ;
#26334 = CARTESIAN_POINT ( 'NONE',  ( -8.062137200540920645, 212.9164362838581894, 15.80113791807856849 ) ) ;
#26335 = CIRCLE ( 'NONE', #31240, 3.399999999999999911 ) ;
#26336 = CARTESIAN_POINT ( 'NONE',  ( -3.135527875058982783, 216.4958274776886924, 81.09886208192143897 ) ) ;
#26337 = EDGE_CURVE ( 'NONE', #28846, #27342, #26505, .T. ) ;
#26338 = EDGE_LOOP ( 'NONE', ( #29192, #2505 ) ) ;
#26339 = CARTESIAN_POINT ( 'NONE',  ( -3.044812012440131443, 216.5253028482142952, 100.1011379180785781 ) ) ;
#26340 = ORIENTED_EDGE ( 'NONE', *, *, #13929, .T. ) ;
#26341 = DIRECTION ( 'NONE',  ( 1.000000000000000000, 0.000000000000000000, 0.000000000000000000 ) ) ;
#26342 = PRODUCT_DEFINITION_CONTEXT ( 'detailed design', #21167, 'design' ) ;
#26343 = CARTESIAN_POINT ( 'NONE',  ( 2.517493886309087436, 199.4062855549015865, 64.59886208192142476 ) ) ;
#26344 = VERTEX_POINT ( 'NONE', #18840 ) ;
#26345 = CARTESIAN_POINT ( 'NONE',  ( 78.52499999726880731, 140.1801316387863778, 4.815267126137185549 ) ) ;
#26346 = LINE ( 'NONE', #31467, #14613 ) ;
#26347 = STYLED_ITEM ( 'NONE', ( #25726 ), #32336 ) ;
#26348 = CARTESIAN_POINT ( 'NONE',  ( 77.50000000000000000, 155.0000000000000000, -6.938893903907228378E-15 ) ) ;
#26349 = UNCERTAINTY_MEASURE_WITH_UNIT (LENGTH_MEASURE( 1.000000000000000082E-05 ), #32551, 'distance_accuracy_value', 'NONE');
#26350 = CARTESIAN_POINT ( 'NONE',  ( 67.62499999726881583, 171.3844434931184253, -7.942151717890132712E-15 ) ) ;
#26351 = CARTESIAN_POINT ( 'NONE',  ( 6.500168698208129925, 211.6636982574063381, 61.70113791807857240 ) ) ;
#26352 = CARTESIAN_POINT ( 'NONE',  ( 32.50000000000000000, 155.0000000000000000, 15.00000000000001243 ) ) ;
#26353 = CARTESIAN_POINT ( 'NONE',  ( -52.50000000000002132, -95.00000000000000000, 270.4495957273638282 ) ) ;
#26354 = CIRCLE ( 'NONE', #2443, 1.000000000000000222 ) ;
#26355 = CARTESIAN_POINT ( 'NONE',  ( 7.894787914004607998, 1.243647571710251278E-13, -7.591390474663425536 ) ) ;
#26356 = B_SPLINE_CURVE_WITH_KNOTS ( 'NONE', 3,
 ( #9666, #20058, #30797, #26177, #7634, #25508, #10362, #4898, #23126, #15784, #125, #2178, #2692, #33514, #12737, #25678, #28580, #2845, #7459, #30627, #12900, #20907, #12562, #2347, #13070, #23460, #10528, #31303, #17841, #31132 ),
 .UNSPECIFIED., .F., .F.,
 ( 4, 2, 2, 2, 2, 2, 2, 2, 2, 2, 2, 2, 2, 2, 4 ),
 ( 0.007818044621537994371, 0.008306560441632113850, 0.008795076261726231595, 0.009772107901914449737, 0.01026062372200855187, 0.01074913954210265227, 0.01123765536219675440, 0.01172617118229085653, 0.01221468700238495693, 0.01270320282247905906, 0.01319171864257315946, 0.01368023446266726159, 0.01416875028276136372, 0.01465726610285546412, 0.01563429774304366665 ),
 .UNSPECIFIED. ) ;
#26357 = CARTESIAN_POINT ( 'NONE',  ( 6.444103211790928043, 211.7408657792734061, 36.69886208192144039 ) ) ;
#26358 = CARTESIAN_POINT ( 'NONE',  ( -9.984503880673473830, 210.2968891136704315, 75.65113791807858945 ) ) ;
#26359 = DIRECTION ( 'NONE',  ( -1.000000000000000000, 0.000000000000000000, 0.000000000000000000 ) ) ;
#26360 = CARTESIAN_POINT ( 'NONE',  ( 0.05014649552810505201, 217.5146222423826714, 61.25113791807856245 ) ) ;
#26361 = CARTESIAN_POINT ( 'NONE',  ( -8.062137200540920645, 212.9164362838581894, 24.80113791807857027 ) ) ;
#26362 = CARTESIAN_POINT ( 'NONE',  ( 7.984503880673485376, 204.3529502787953902, 17.15113791807856458 ) ) ;
#26363 = CARTESIAN_POINT ( 'NONE',  ( 87.50000000000001421, 160.9457742543943652, -14.40357817542362540 ) ) ;
#26364 = CARTESIAN_POINT ( 'NONE',  ( 60.78867513459481842, 155.0000000000000000, -15.00000000000002487 ) ) ;
#26365 = CARTESIAN_POINT ( 'NONE',  ( 46.82499999726881157, 141.7447067706911810, -9.630534252274387086 ) ) ;
#26366 = CARTESIAN_POINT ( 'NONE',  ( 9.736236675707914401, 214.0148392665762458, 34.70113791807856529 ) ) ;
#26367 = DIRECTION ( 'NONE',  ( 1.000000000000000000, 0.000000000000000000, 0.000000000000000000 ) ) ;
#26368 = CARTESIAN_POINT ( 'NONE',  ( 8.118202686958039038, 212.8392687619912635, 85.70113791807858661 ) ) ;
#26369 = CARTESIAN_POINT ( 'NONE',  ( 3.135527875058820690, 216.4958274776887492, 61.40113791807857524 ) ) ;
#26370 = CARTESIAN_POINT ( 'NONE',  ( -9.736236675708031640, 214.0148392665760753, 20.79886208192143826 ) ) ;
#26371 = CARTESIAN_POINT ( 'NONE',  ( -8.118202686958138514, 212.8392687619910930, 38.79886208192143471 ) ) ;
#26372 = CARTESIAN_POINT ( 'NONE',  ( 78.49999999453764588, 170.2462022514548323, -7.872454543227099337E-15 ) ) ;
#26373 = CARTESIAN_POINT ( 'NONE',  ( 12.01549611932652972, 210.8513442034534933, 67.85113791807857808 ) ) ;
#26374 = CARTESIAN_POINT ( 'NONE',  ( -4.984841277089726574, 200.2242689037092305, 90.05113791807858092 ) ) ;
#26375 = CARTESIAN_POINT ( 'NONE',  ( 9.984503880673420539, 210.2968891136705167, 54.84886208192141765 ) ) ;
#26376 = ADVANCED_FACE ( 'NONE', ( #5887 ), #3334, .T. ) ;
#26377 = ORIENTED_EDGE ( 'NONE', *, *, #20440, .T. ) ;
#26378 = CARTESIAN_POINT ( 'NONE',  ( -3.753561863808878130, 218.3979405102790281, 54.09886208192143897 ) ) ;
#26379 = ORIENTED_EDGE ( 'NONE', *, *, #20375, .F. ) ;
#26380 = EDGE_CURVE ( 'NONE', #26053, #29866, #1947, .T. ) ;
#26381 = ORIENTED_EDGE ( 'NONE', *, *, #12703, .F. ) ;
#26382 = CARTESIAN_POINT ( 'NONE',  ( 74.67499999726879878, 141.7447067706911810, 9.630534252274376428 ) ) ;
#26383 = DIRECTION ( 'NONE',  ( 1.000000000000000000, 0.000000000000000000, 0.000000000000000000 ) ) ;
#26384 = ADVANCED_FACE ( 'NONE', ( #9463 ), #19850, .T. ) ;
#26385 = CARTESIAN_POINT ( 'NONE',  ( 58.98867513459482836, 163.8167787843871110, -12.13525491562423397 ) ) ;
#26386 = CARTESIAN_POINT ( 'NONE',  ( -4.984841277089726574, 200.2242689037092305, 42.05113791807857382 ) ) ;
#26387 =( LENGTH_UNIT ( ) NAMED_UNIT ( * ) SI_UNIT ( .MILLI., .METRE. ) );
#26388 = CARTESIAN_POINT ( 'NONE',  ( -9.984503880673420539, 203.7031108863293980, 23.34886208192142831 ) ) ;
#26389 = CARTESIAN_POINT ( 'NONE',  ( 65.67499999726881299, 168.2552932293087906, -9.630534252274387086 ) ) ;
#26390 = EDGE_LOOP ( 'NONE', ( #27977, #5432, #2044, #28658 ) ) ;
#26391 = CARTESIAN_POINT ( 'NONE',  ( 36.51132485994280330, 163.8167787843871110, 12.13525491562421621 ) ) ;
#26392 = PRESENTATION_STYLE_ASSIGNMENT (( #16000 ) ) ;
#26393 = DIRECTION ( 'NONE',  ( -0.000000000000000000, -0.000000000000000000, 1.000000000000000000 ) ) ;
#26394 = CARTESIAN_POINT ( 'NONE',  ( -8.000000000000008882, 206.9523078486584780, 5.498862081921434886 ) ) ;
#26395 = CARTESIAN_POINT ( 'NONE',  ( 10.01549611932653860, 210.2015048109876716, 46.85113791807856387 ) ) ;
#26397 = ADVANCED_FACE ( 'NONE', ( #11515 ), #19177, .F. ) ;
#26396 = PRODUCT_DEFINITION_SHAPE ( 'NONE', 'NONE',  #33710 ) ;
#26398 = CARTESIAN_POINT ( 'NONE',  ( -10.01549611932653860, 203.7984951890123284, 24.35113791807855677 ) ) ;
#26399 = CARTESIAN_POINT ( 'NONE',  ( 86.77499999726882152, 140.1801316387863778, 4.815267126137185549 ) ) ;
#26400 = CARTESIAN_POINT ( 'NONE',  ( 4.984841277089891776, 200.2242689037093726, 94.44886208192143329 ) ) ;
#26401 = CARTESIAN_POINT ( 'NONE',  ( 37.32499999726881157, 164.1591823560292198, -12.60653300113719766 ) ) ;
#26402 = PRESENTATION_STYLE_ASSIGNMENT (( #13951 ) ) ;
#26403 = CARTESIAN_POINT ( 'NONE',  ( 10.00000000000000711, 207.0000000000000853, 0.000000000000000000 ) ) ;
#26404 = CARTESIAN_POINT ( 'NONE',  ( 7.375838497908181246, 196.7627149292499666, 11.45113791807856529 ) ) ;
#26405 = CARTESIAN_POINT ( 'NONE',  ( 82.48867513459482836, 142.2402378747194405, -9.270509831248439525 ) ) ;
#26406 = CARTESIAN_POINT ( 'NONE',  ( 54.27499999726880020, 160.0630714827496206, 15.58253174999999402 ) ) ;
#26407 = EDGE_CURVE ( 'NONE', #24271, #5394, #30317, .T. ) ;
#26408 = CARTESIAN_POINT ( 'NONE',  ( -3.044812012440131443, 216.5253028482142952, 58.10113791807857808 ) ) ;
#26409 = CARTESIAN_POINT ( 'NONE',  ( 3.135527875058820690, 216.4958274776887492, 25.40113791807856813 ) ) ;
#26410 = CARTESIAN_POINT ( 'NONE',  ( -58.50000000000001421, -88.00000000000000000, -20.00000000000000000 ) ) ;
#26411 = CARTESIAN_POINT ( 'NONE',  ( 55.68867513459483831, 159.8737954434936057, 15.00000000000001421 ) ) ;
#26412 = FACE_OUTER_BOUND ( 'NONE', #905, .T. ) ;
#26413 = CARTESIAN_POINT ( 'NONE',  ( 58.19999999453763451, 163.5228861582408797, -11.73074641843674470 ) ) ;
#26414 = ORIENTED_EDGE ( 'NONE', *, *, #2071, .F. ) ;
#26415 = CARTESIAN_POINT ( 'NONE',  ( 12.01549611932652972, 210.8513442034534933, 37.85113791807856387 ) ) ;
#26416 = CARTESIAN_POINT ( 'NONE',  ( -4.336808689942017736E-14, -31.75426480542944319, -15.54379906938135214 ) ) ;
#26417 = CARTESIAN_POINT ( 'NONE',  ( 8.118202686958138514, 201.1607312380088501, 25.29886208192143826 ) ) ;
#26418 = PLANE ( 'NONE',  #16115 ) ;
#26419 = ORIENTED_EDGE ( 'NONE', *, *, #16463, .T. ) ;
#26420 = CARTESIAN_POINT ( 'NONE',  ( -8.118202686958039038, 201.1607312380087080, 78.20113791807857240 ) ) ;
#26421 = ORIENTED_EDGE ( 'NONE', *, *, #23088, .T. ) ;
#26422 = CARTESIAN_POINT ( 'NONE',  ( 87.50000000000004263, 168.9939550398769086, -6.930048056949515534 ) ) ;
#26423 = LINE ( 'NONE', #18433, #26309 ) ;
#26424 = ORIENTED_EDGE ( 'NONE', *, *, #26625, .T. ) ;
#26425 = CARTESIAN_POINT ( 'NONE',  ( -8.000000000000008882, 207.0476921513413515, 9.501137918078566003 ) ) ;
#26426 = ADVANCED_FACE ( 'NONE', ( #14064 ), #21049, .F. ) ;
#26427 = CARTESIAN_POINT ( 'NONE',  ( 12.01549611932659367, 203.1486557965466773, 94.14886208192145034 ) ) ;
#26428 = CARTESIAN_POINT ( 'NONE',  ( 46.47499999726880304, 149.9369285172503510, 15.58253174999999580 ) ) ;
#26429 = ORIENTED_EDGE ( 'NONE', *, *, #19594, .T. ) ;
#26430 = CARTESIAN_POINT ( 'NONE',  ( 50.22499999726880304, 149.9369285172503510, 15.58253174999999580 ) ) ;
#26431 = DIRECTION ( 'NONE',  ( 1.000000000000000000, 0.000000000000000000, 0.000000000000000000 ) ) ;
#26432 = CARTESIAN_POINT ( 'NONE',  ( 2.000000000000000000, 1.773042676681340968, -2.276824562219559311E-15 ) ) ;
#26433 = CARTESIAN_POINT ( 'NONE',  ( -0.05014649552828403384, 217.5146222423826714, 81.24886208192140202 ) ) ;
#26434 = CARTESIAN_POINT ( 'NONE',  ( 52.57499999726881157, 145.8408176439707802, 12.60653300113718345 ) ) ;
#26435 = CARTESIAN_POINT ( 'NONE',  ( 6.139770520408368348, 198.4640165459539674, 20.45113791807855819 ) ) ;
#26436 = CARTESIAN_POINT ( 'NONE',  ( 32.50000000000000000, 155.0000000000000000, -6.938893903907228378E-15 ) ) ;
#26437 = EDGE_CURVE ( 'NONE', #14059, #4327, #27687, .T. ) ;
#26438 = CARTESIAN_POINT ( 'NONE',  ( 74.89999999999999147, 168.7903194862797420, -4.480746418436745593 ) ) ;
#26439 = CARTESIAN_POINT ( 'NONE',  ( -9.984503880673473830, 210.2968891136704315, 99.65113791807853261 ) ) ;
#26440 = DIRECTION ( 'NONE',  ( -1.000000000000000000, -0.000000000000000000, -0.000000000000000000 ) ) ;
#26441 = CARTESIAN_POINT ( 'NONE',  ( 3.044812012440130555, 197.4746971517856764, 83.60113791807857808 ) ) ;
#26442 = CARTESIAN_POINT ( 'NONE',  ( 56.78867513459481842, 155.0000000000000000, -15.00000000000002487 ) ) ;
#26443 = CARTESIAN_POINT ( 'NONE',  ( 37.57499999726881157, 164.1591823560292198, -12.60653300113719766 ) ) ;
#26444 = ADVANCED_FACE ( 'NONE', ( #8955 ), #3102, .T. ) ;
#26445 = CARTESIAN_POINT ( 'NONE',  ( 7.375838497908012492, 217.2372850707501186, 96.54886208192142760 ) ) ;
#26446 = CARTESIAN_POINT ( 'NONE',  ( 79.72499999726881015, 169.8198683612136222, 4.815267126137181997 ) ) ;
#26447 = ORIENTED_EDGE ( 'NONE', *, *, #26407, .T. ) ;
#26448 = CARTESIAN_POINT ( 'NONE',  ( 54.30000000000001137, -88.00000000000000000, 30.00000000000000000 ) ) ;
#26449 = CARTESIAN_POINT ( 'NONE',  ( 42.39999999453762314, 168.7903194862797420, -4.480746418436745593 ) ) ;
#26450 = B_SPLINE_CURVE_WITH_KNOTS ( 'NONE', 3,
 ( #17562, #22334, #11952, #7009 ),
 .UNSPECIFIED., .F., .F.,
 ( 4, 4 ),
 ( 2.380739282308591161E-07, 0.002044882221487502854 ),
 .UNSPECIFIED. ) ;
#26451 = CARTESIAN_POINT ( 'NONE',  ( -3.499999999999997780, -2.020725942163714262, -2.587392608830344720 ) ) ;
#26452 = CARTESIAN_POINT ( 'NONE',  ( 6.874999999999997335, -4.690970937165716670, -7.298562697733105509 ) ) ;
#26453 = VERTEX_POINT ( 'NONE', #6906 ) ;
#26454 = CARTESIAN_POINT ( 'NONE',  ( -3.135527875058982783, 216.4958274776886924, 93.09886208192145318 ) ) ;
#26455 = CARTESIAN_POINT ( 'NONE',  ( -9.736236675708031640, 214.0148392665760753, 29.79886208192143826 ) ) ;
#26456 = CARTESIAN_POINT ( 'NONE',  ( 95.70416941062676131, 155.0000000000000000, 32.00000000000005684 ) ) ;
#26457 = CARTESIAN_POINT ( 'NONE',  ( 10.00000000000000711, 206.9523078486586201, 41.00113791807856956 ) ) ;
#26458 = ORIENTED_EDGE ( 'NONE', *, *, #2027, .F. ) ;
#26459 = CARTESIAN_POINT ( 'NONE',  ( 2.426778023690075337, 214.6231898156240447, 6.398862081921435241 ) ) ;
#26460 = CLOSED_SHELL ( 'NONE', ( #33066, #26426, #2190, #4109, #26444, #10877, #1909, #28327, #10424, #25764, #1017, #18755, #17033, #30183, #28541, #10654, #12460, #5572, #33424, #10456, #22239, #1474, #13867, #19779, #31417, #7099, #26017, #13403, #18676, #14060, #32016, #22523 ) ) ;
#26461 = FACE_OUTER_BOUND ( 'NONE', #10975, .T. ) ;
#26462 = EDGE_LOOP ( 'NONE', ( #12504, #27926, #14694, #33476 ) ) ;
#26463 = CARTESIAN_POINT ( 'NONE',  ( 4.903702542908435547, 213.8346818373419751, 90.54886208192144181 ) ) ;
#26464 = EDGE_CURVE ( 'NONE', #14208, #5796, #22399, .T. ) ;
#26465 = CARTESIAN_POINT ( 'NONE',  ( -2.517493886308901807, 199.4062855549015012, 32.90113791807857524 ) ) ;
#26466 = DIRECTION ( 'NONE',  ( 1.000000000000000000, -0.000000000000000000, -0.000000000000000000 ) ) ;
#26468 = EDGE_LOOP ( 'NONE', ( #16555, #1536, #6768, #16817, #21760 ) ) ;
#26467 = CONICAL_SURFACE ( 'NONE', #32443, 32.10452846326764131, 1.466076571675242413 ) ;
#26469 = DIRECTION ( 'NONE',  ( 0.000000000000000000, -0.8660254037844389297, -0.4999999999999995004 ) ) ;
#26470 = CARTESIAN_POINT ( 'NONE',  ( 35.27499999726881441, 149.9369285172503510, -15.58253175000000823 ) ) ;
#26471 = FACE_OUTER_BOUND ( 'NONE', #17129, .T. ) ;
#26472 = CARTESIAN_POINT ( 'NONE',  ( -0.05014649552807731031, 198.5883022060938572, 98.75113791807856956 ) ) ;
#26473 = EDGE_CURVE ( 'NONE', #3669, #6381, #27581, .T. ) ;
#26474 = CARTESIAN_POINT ( 'NONE',  ( 57.70000000000000284, 146.4771138417591203, 11.73074641843673227 ) ) ;
#26475 = CARTESIAN_POINT ( 'NONE',  ( 6.444103211790928043, 211.7408657792734061, 69.69886208192143329 ) ) ;
#26476 = CYLINDRICAL_SURFACE ( 'NONE', #21625, 31.00000000000000000 ) ;
#26477 = AXIS2_PLACEMENT_3D ( 'NONE', #27039, #24486, #4201 ) ;
#26478 = CARTESIAN_POINT ( 'NONE',  ( 49.42499999726879878, 168.2552932293087906, -9.630534252274385310 ) ) ;
#26480 = ORIENTED_EDGE ( 'NONE', *, *, #7424, .T. ) ;
#26479 = CARTESIAN_POINT ( 'NONE',  ( 9.984503880673473830, 203.7031108863295401, 11.15113791807856458 ) ) ;
#26481 = CARTESIAN_POINT ( 'NONE',  ( -6.500000000000001776, -2.692912473542373952, -6.218066308278946686 ) ) ;
#26482 = CARTESIAN_POINT ( 'NONE',  ( 64.22499999726881015, 149.9369285172503510, 15.58253174999999580 ) ) ;
#26483 = CARTESIAN_POINT ( 'NONE',  ( 75.27499999726879309, 149.9369285172503510, -15.58253175000000823 ) ) ;
#26484 = CARTESIAN_POINT ( 'NONE',  ( -12.00000000000000711, 207.0476921513413515, 72.50113791807856956 ) ) ;
#26485 = DIRECTION ( 'NONE',  ( 0.000000000000000000, 0.000000000000000000, -1.000000000000000000 ) ) ;
#26486 = CARTESIAN_POINT ( 'NONE',  ( -0.05014649552810635652, 196.4853777576173002, 98.75113791807855534 ) ) ;
#26487 = CARTESIAN_POINT ( 'NONE',  ( 84.18867513459483121, 140.7341522555726669, 4.635254915624211769 ) ) ;
#26488 = CIRCLE ( 'NONE', #13993, 37.00000000000000711 ) ;
#26489 = ORIENTED_EDGE ( 'NONE', *, *, #27856, .F. ) ;
#26490 = CARTESIAN_POINT ( 'NONE',  ( -12.01549611932659722, 210.8513442034533227, 65.64886208192142192 ) ) ;
#26491 = CARTESIAN_POINT ( 'NONE',  ( -6.139770520408224463, 198.4640165459539105, 68.04886208192144181 ) ) ;
#26492 = CARTESIAN_POINT ( 'NONE',  ( -3.753561863808878130, 218.3979405102790281, 3.098862081921434530 ) ) ;
#26493 = CARTESIAN_POINT ( 'NONE',  ( 0.000000000000000000, 0.000000000000000000, 2.066666666667000385 ) ) ;
#26494 = CARTESIAN_POINT ( 'NONE',  ( 10.01549611932653860, 210.2015048109876716, 13.85113791807856742 ) ) ;
#26495 = CARTESIAN_POINT ( 'NONE',  ( -8.118202686958138514, 212.8392687619910930, 80.79886208192144181 ) ) ;
#26496 = ORIENTED_EDGE ( 'NONE', *, *, #29362, .F. ) ;
#26497 = CARTESIAN_POINT ( 'NONE',  ( 9.984503880673470277, 203.7031108863295401, 101.1511379180785752 ) ) ;
#26498 = VERTEX_POINT ( 'NONE', #29574 ) ;
#26499 = PRESENTATION_STYLE_ASSIGNMENT (( #5717 ) ) ;
#26500 = CARTESIAN_POINT ( 'NONE',  ( 7.984503880673422316, 209.6470497212048372, 63.84886208192143187 ) ) ;
#26501 = AXIS2_PLACEMENT_3D ( 'NONE', #22497, #9543, #7000 ) ;
#26502 = ORIENTED_EDGE ( 'NONE', *, *, #33319, .T. ) ;
#26503 = CIRCLE ( 'NONE', #15103, 3.999999999999996003 ) ;
#26504 = CARTESIAN_POINT ( 'NONE',  ( 77.72499999726881015, 169.8198683612136222, 4.815267126137181997 ) ) ;
#26505 = LINE ( 'NONE', #3174, #13002 ) ;
#26506 = FACE_OUTER_BOUND ( 'NONE', #22786, .T. ) ;
#26507 = CARTESIAN_POINT ( 'NONE',  ( 68.42499999726881299, 141.7447067706911810, 9.630534252274376428 ) ) ;
#26508 = CARTESIAN_POINT ( 'NONE',  ( 6.444103211791042618, 202.2591342207267644, 62.30113791807858092 ) ) ;
#26509 = CIRCLE ( 'NONE', #22733, 0.9999999999999968914 ) ;
#26510 = FACE_OUTER_BOUND ( 'NONE', #20802, .T. ) ;
#26511 = CARTESIAN_POINT ( 'NONE',  ( 38.50000000000000000, 155.0000000000000000, -14.50000000000000711 ) ) ;
#26512 = CARTESIAN_POINT ( 'NONE',  ( -8.015496119326597224, 209.5516654185217362, 47.64886208192145034 ) ) ;
#26513 = CARTESIAN_POINT ( 'NONE',  ( 10.00000000000000711, 206.9523078486586201, 80.00113791807856956 ) ) ;
#26514 = DIRECTION ( 'NONE',  ( 0.000000000000000000, 0.000000000000000000, -1.000000000000000000 ) ) ;
#26515 = EDGE_CURVE ( 'NONE', #3092, #5650, #29603, .T. ) ;
#26516 = CARTESIAN_POINT ( 'NONE',  ( 9.984503880673470277, 203.7031108863295401, 68.15113791807857524 ) ) ;
#26517 = DIRECTION ( 'NONE',  ( 1.000000000000000000, -0.000000000000000000, -0.000000000000000000 ) ) ;
#26518 = CARTESIAN_POINT ( 'NONE',  ( -6.444103211791042618, 211.7408657792732356, 12.80113791807856849 ) ) ;
#26519 = CARTESIAN_POINT ( 'NONE',  ( 1.250000000000000222, 7.938566201357357244, -7.198902722707428481 ) ) ;
#26520 = CARTESIAN_POINT ( 'NONE',  ( 42.72499999726881015, 140.1801316387863778, -4.815267126137194431 ) ) ;
#26521 = CARTESIAN_POINT ( 'NONE',  ( 7.456977232089302632, 217.1783343296989131, 52.55113791807856671 ) ) ;
#26522 = CARTESIAN_POINT ( 'NONE',  ( 7.894705354777835637, 0.7527931906242791849, -7.590204373988219011 ) ) ;
#26523 = CONICAL_SURFACE ( 'NONE', #2620, 3.499999999999999556, 1.047197551196589638 ) ;
#26524 = CARTESIAN_POINT ( 'NONE',  ( -10.00000000000000711, 207.0476921513413515, 99.50113791807856956 ) ) ;
#26525 = CARTESIAN_POINT ( 'NONE',  ( 10.01549611932653860, 210.2015048109876716, 70.85113791807856387 ) ) ;
#26526 = PRESENTATION_LAYER_ASSIGNMENT (  '', '', ( #19460 ) ) ;
#26527 = CARTESIAN_POINT ( 'NONE',  ( -3.753561863808878130, 218.3979405102790281, 27.09886208192143897 ) ) ;
#26528 = CARTESIAN_POINT ( 'NONE',  ( 3.135527875058981895, 197.5041725223112792, 37.59886208192143187 ) ) ;
#26529 = CARTESIAN_POINT ( 'NONE',  ( 80.49999999453763166, 170.2462022514548323, -7.872454543227099337E-15 ) ) ;
#26530 = CARTESIAN_POINT ( 'NONE',  ( 7.456977232089302632, 217.1783343296989131, 73.55113791807856671 ) ) ;
#26531 = CARTESIAN_POINT ( 'NONE',  ( 0.05014649552807626948, 215.4116977939061144, 85.25113791807856956 ) ) ;
#26532 = CARTESIAN_POINT ( 'NONE',  ( -10.00000000000000711, 206.9523078486584495, 47.49886208192143755 ) ) ;
#26533 = CARTESIAN_POINT ( 'NONE',  ( 100.3117322205716420, 155.0000000000000000, -12.10452846326767684 ) ) ;
#26534 = CIRCLE ( 'NONE', #9127, 6.500000000000000888 ) ;
#26535 = ORIENTED_EDGE ( 'NONE', *, *, #21820, .T. ) ;
#26536 = CARTESIAN_POINT ( 'NONE',  ( -9.736236675708031640, 214.0148392665760753, 47.79886208192143471 ) ) ;
#26537 = EDGE_LOOP ( 'NONE', ( #21849, #6010, #28621, #20698 ) ) ;
#26538 = ORIENTED_EDGE ( 'NONE', *, *, #11249, .F. ) ;
#26539 = CARTESIAN_POINT ( 'NONE',  ( 74.57499999726881867, 145.8408176439707802, 12.60653300113718345 ) ) ;
#26540 = DIRECTION ( 'NONE',  ( 0.000000000000000000, 0.000000000000000000, 1.000000000000000000 ) ) ;
#26541 = CARTESIAN_POINT ( 'NONE',  ( 59.28867513459483263, 170.7719333635740497, -7.904646289410545231E-15 ) ) ;
#26542 = CARTESIAN_POINT ( 'NONE',  ( -0.05014649552807731031, 198.5883022060938572, 47.75113791807856245 ) ) ;
#26543 = AXIS2_PLACEMENT_3D ( 'NONE', #18803, #29195, #5847 ) ;
#26544 = CARTESIAN_POINT ( 'NONE',  ( 0.05014649552828275708, 196.4853777576173002, 34.74886208192143044 ) ) ;
#26545 = CARTESIAN_POINT ( 'NONE',  ( 59.87499999726881583, 171.3844434931184253, -7.942151717890134290E-15 ) ) ;
#26546 = EDGE_LOOP ( 'NONE', ( #21894, #6171, #31820, #3609, #24963 ) ) ;
#26547 = CARTESIAN_POINT ( 'NONE',  ( 36.61132485994281893, 159.8737954434935489, 15.00000000000005151 ) ) ;
#26548 = CARTESIAN_POINT ( 'NONE',  ( 0.000000000000000000, 0.000000000000000000, 3.469446951953614189E-15 ) ) ;
#26549 = CARTESIAN_POINT ( 'NONE',  ( 2.517493886309087436, 199.4062855549015865, 10.59886208192143542 ) ) ;
#26550 = CARTESIAN_POINT ( 'NONE',  ( 0.05014649552810505201, 217.5146222423826714, 52.25113791807856245 ) ) ;
#26551 = DIRECTION ( 'NONE',  ( -1.000000000000000000, 0.000000000000000000, 0.000000000000000000 ) ) ;
#26552 = EDGE_CURVE ( 'NONE', #33143, #1032, #8548, .T. ) ;
#26553 = CARTESIAN_POINT ( 'NONE',  ( 10.00000000000000711, 206.9523078486586201, 38.00113791807857666 ) ) ;
#26554 = CARTESIAN_POINT ( 'NONE',  ( 87.47499999726883857, 160.0630714827496206, -15.58253175000000823 ) ) ;
#26555 = CIRCLE ( 'NONE', #28206, 2.149999999999985256 ) ;
#26556 = CARTESIAN_POINT ( 'NONE',  ( 6.500168698208244500, 202.3363017425938324, 91.29886208192142760 ) ) ;
#26557 = CARTESIAN_POINT ( 'NONE',  ( 40.52499999726881441, 140.1801316387863778, 4.815267126137185549 ) ) ;
#26558 =( NAMED_UNIT ( * ) PLANE_ANGLE_UNIT ( ) SI_UNIT ( $, .RADIAN. ) );
#26559 = DIRECTION ( 'NONE',  ( -1.000000000000000000, -8.584654849926598947E-16, 0.000000000000000000 ) ) ;
#26560 = CARTESIAN_POINT ( 'NONE',  ( 12.00000000000000711, 206.9523078486586485, 17.00113791807856956 ) ) ;
#26561 = CARTESIAN_POINT ( 'NONE',  ( 6.625705691649528717, -5.306270977113132226, -7.795653906408932521 ) ) ;
#26562 = CARTESIAN_POINT ( 'NONE',  ( 59.17499999726881299, 145.8408176439707802, -12.60653300113719588 ) ) ;
#26563 = CARTESIAN_POINT ( 'NONE',  ( -10.00000000000000711, 207.0476921513413515, 66.50113791807856956 ) ) ;
#26564 = CARTESIAN_POINT ( 'NONE',  ( -8.118202686958039038, 201.1607312380087080, 33.20113791807857240 ) ) ;
#26565 = CARTESIAN_POINT ( 'NONE',  ( 5.000000000000000000, -2.342598717236912265, -4.057499999999995666 ) ) ;
#26566 = ADVANCED_FACE ( 'NONE', ( #19518 ), #22137, .T. ) ;
#26567 = CARTESIAN_POINT ( 'NONE',  ( -7.500000000000000000, -4.330127018922198090, -7.422398894150034288 ) ) ;
#26568 = CARTESIAN_POINT ( 'NONE',  ( 8.062137200540822946, 212.9164362838583315, 9.698862081921435063 ) ) ;
#26569 = CARTESIAN_POINT ( 'NONE',  ( 59.49999999453761745, 139.7537977485451393, -4.138211985947621020E-15 ) ) ;
#26570 = ORIENTED_EDGE ( 'NONE', *, *, #5485, .T. ) ;
#26571 = CARTESIAN_POINT ( 'NONE',  ( 7.456977232089302632, 217.1783343296989131, 37.55113791807855961 ) ) ;
#26572 = CONICAL_SURFACE ( 'NONE', #20038, 4.171999999999999709, 0.7853981633974687071 ) ;
#26573 = DIRECTION ( 'NONE',  ( 0.000000000000000000, 0.000000000000000000, -1.000000000000000000 ) ) ;
#26574 = CARTESIAN_POINT ( 'NONE',  ( -6.220909254589682469, 215.4770327129946850, 23.94886208192142618 ) ) ;
#26575 = VECTOR ( 'NONE', #12561, 1000.000000000000000 ) ;
#26576 = CARTESIAN_POINT ( 'NONE',  ( 71.91132485994280898, 163.8167787843871110, -12.13525491562423397 ) ) ;
#26577 = ORIENTED_EDGE ( 'NONE', *, *, #4594, .T. ) ;
#26578 = AXIS2_PLACEMENT_3D ( 'NONE', #7763, #17808, #25305 ) ;
#26579 = EDGE_CURVE ( 'NONE', #13101, #20988, #15624, .T. ) ;
#26580 = CARTESIAN_POINT ( 'NONE',  ( -10.00000000000000711, 207.0476921513413515, 78.50113791807856956 ) ) ;
#26581 = ORIENTED_EDGE ( 'NONE', *, *, #15399, .T. ) ;
#26582 = CIRCLE ( 'NONE', #17351, 12.10452846326765020 ) ;
#26583 = CARTESIAN_POINT ( 'NONE',  ( 50.11132485994281183, 169.2658477444273331, -4.635254915624224203 ) ) ;
#26584 = ORIENTED_EDGE ( 'NONE', *, *, #9825, .T. ) ;
#26585 = CARTESIAN_POINT ( 'NONE',  ( -0.05014649552807731031, 198.5883022060938572, 14.75113791807856600 ) ) ;
#26586 = EDGE_CURVE ( 'NONE', #17155, #22495, #25401, .T. ) ;
#26587 = CARTESIAN_POINT ( 'NONE',  ( -60.48684543773389066, 194.9711049089068808, 1.526260319620769579 ) ) ;
#26588 = CARTESIAN_POINT ( 'NONE',  ( 6.220909254589681581, 198.5229672870052582, 4.448862081921432399 ) ) ;
#26589 = CARTESIAN_POINT ( 'NONE',  ( 43.27499999726880731, 149.9369285172503510, -15.58253175000000823 ) ) ;
#26590 = ORIENTED_EDGE ( 'NONE', *, *, #1334, .F. ) ;
#26591 = CARTESIAN_POINT ( 'NONE',  ( 50.92499999726880588, 145.8408176439707802, -12.60653300113719588 ) ) ;
#26592 = CARTESIAN_POINT ( 'NONE',  ( -2.428571428571428381, 2.974142226500714333E-16, 3.100000000000000533 ) ) ;
#26593 = CARTESIAN_POINT ( 'NONE',  ( 0.000000000000000000, 0.000000000000000000, -25.03750572909317285 ) ) ;
#26594 = FACE_OUTER_BOUND ( 'NONE', #6128, .T. ) ;
#26595 = VECTOR ( 'NONE', #12166, 1000.000000000000000 ) ;
#26596 = CARTESIAN_POINT ( 'NONE',  ( 10.01549611932659545, 203.7984951890123853, 82.14886208192140771 ) ) ;
#26597 = CARTESIAN_POINT ( 'NONE',  ( 51.27499999726880731, 149.9369285172503510, -15.58253175000000823 ) ) ;
#26598 = CARTESIAN_POINT ( 'NONE',  ( 8.062137200540920645, 201.0835637161417822, 20.30113791807856671 ) ) ;
#26599 = DIRECTION ( 'NONE',  ( 1.000000000000000000, 0.000000000000000000, 0.000000000000000000 ) ) ;
#26600 = EDGE_CURVE ( 'NONE', #11107, #250, #5028, .T. ) ;
#26601 = CARTESIAN_POINT ( 'NONE',  ( 12.00000000000000711, 207.0476921513415220, 81.99886208192144466 ) ) ;
#26602 = CARTESIAN_POINT ( 'NONE',  ( -4.903702542908436435, 200.1653181626580249, 35.04886208192144181 ) ) ;
#26603 = CARTESIAN_POINT ( 'NONE',  ( 72.09999999999999432, 141.2096805137202580, -4.480746418436742040 ) ) ;
#26604 = CARTESIAN_POINT ( 'NONE',  ( -150.0000000000000000, 0.000000000000000000, 35.00000000000000000 ) ) ;
#26605 = DIRECTION ( 'NONE',  ( 1.000000000000000000, 0.000000000000000000, 0.000000000000000000 ) ) ;
#26606 = CARTESIAN_POINT ( 'NONE',  ( -8.118202686958039038, 201.1607312380087080, 84.20113791807858661 ) ) ;
#26607 = CARTESIAN_POINT ( 'NONE',  ( -52.50000000000002132, 120.3589838486224437, 20.00000000000000000 ) ) ;
#26608 = CARTESIAN_POINT ( 'NONE',  ( 36.37499999726881583, 155.0000000000000000, 15.58253174999999402 ) ) ;
#26609 = CARTESIAN_POINT ( 'NONE',  ( 3.135527875058820690, 216.4958274776887492, 34.40113791807856813 ) ) ;
#26610 = CARTESIAN_POINT ( 'NONE',  ( 76.92499999726881299, 145.8408176439707802, -12.60653300113719588 ) ) ;
#26611 = EDGE_CURVE ( 'NONE', #5848, #5152, #33309, .T. ) ;
#26612 = ORIENTED_EDGE ( 'NONE', *, *, #10960, .F. ) ;
#26613 = DIRECTION ( 'NONE',  ( 0.000000000000000000, 0.000000000000000000, 1.000000000000000000 ) ) ;
#26614 = CARTESIAN_POINT ( 'NONE',  ( 38.09999999453761887, 159.7113355953771077, -14.50000000000000888 ) ) ;
#26615 = CARTESIAN_POINT ( 'NONE',  ( 9.736236675707914401, 214.0148392665762458, 10.70113791807856529 ) ) ;
#26616 = DIRECTION ( 'NONE',  ( 0.000000000000000000, 0.000000000000000000, 1.000000000000000000 ) ) ;
#26617 = CARTESIAN_POINT ( 'NONE',  ( 1.649999999999999911, 0.000000000000000000, 2.066666666667000385 ) ) ;
#26618 = ORIENTED_EDGE ( 'NONE', *, *, #23365, .T. ) ;
#26619 = CARTESIAN_POINT ( 'NONE',  ( 3.135527875058981895, 197.5041725223112792, 91.59886208192143897 ) ) ;
#26620 = CARTESIAN_POINT ( 'NONE',  ( -12.00000000000000711, 206.9523078486584780, 35.49886208192143044 ) ) ;
#26621 = CARTESIAN_POINT ( 'NONE',  ( -7.894787914004607998, -0.7661396099416333261, -7.591390474663429089 ) ) ;
#26622 = VECTOR ( 'NONE', #31530, 999.9999999999998863 ) ;
#26623 = CARTESIAN_POINT ( 'NONE',  ( -6.139770520408369237, 215.5359834540460042, 48.95113791807855108 ) ) ;
#26624 = ORIENTED_EDGE ( 'NONE', *, *, #19475, .F. ) ;
#26625 = EDGE_CURVE ( 'NONE', #4155, #19887, #15417, .T. ) ;
#26626 = CARTESIAN_POINT ( 'NONE',  ( -4.984841277089891776, 213.7757310962905990, 17.94886208192143684 ) ) ;
#26627 = CARTESIAN_POINT ( 'NONE',  ( -14.91983402814538451, -23.14029461301517543, -17.98559444045775280 ) ) ;
#26628 = ORIENTED_EDGE ( 'NONE', *, *, #12848, .F. ) ;
#26629 = CARTESIAN_POINT ( 'NONE',  ( 6.444103211790928043, 211.7408657792734061, 87.69886208192144750 ) ) ;
#26630 = ADVANCED_FACE ( 'NONE', ( #32962, #17636 ), #15247, .T. ) ;
#26631 = CONICAL_SURFACE ( 'NONE', #23426, 32.10452846326764131, 1.466076571675242413 ) ;
#26632 = CARTESIAN_POINT ( 'NONE',  ( 2.517493886308900919, 214.5937144450984420, 34.40113791807856813 ) ) ;
#26633 = CARTESIAN_POINT ( 'NONE',  ( 7.500000000000000888, -0.7512838658081439913, 1.423015351387224570E-15 ) ) ;
#26634 = ORIENTED_EDGE ( 'NONE', *, *, #25296, .T. ) ;
#26635 = LINE ( 'NONE', #3137, #16690 ) ;
#26636 = CARTESIAN_POINT ( 'NONE',  ( 36.17499999726880588, 164.1591823560292198, 12.60653300113718167 ) ) ;
#26637 = DIRECTION ( 'NONE',  ( 0.000000000000000000, 0.000000000000000000, 1.000000000000000000 ) ) ;
#26638 = CARTESIAN_POINT ( 'NONE',  ( 8.000000000000008882, 206.9523078486586485, 95.00113791807856956 ) ) ;
#26639 = SHAPE_REPRESENTATION_RELATIONSHIP ( 'NONE' , 'NONE' ,  #16098, #26255 ) ;
#26640 = CARTESIAN_POINT ( 'NONE',  ( 55.40000000000000568, 159.7113355953771077, 14.49999999999999289 ) ) ;
#26641 = CARTESIAN_POINT ( 'NONE',  ( 2.426778023690075337, 214.6231898156240447, 75.39886208192143613 ) ) ;
#26642 = CARTESIAN_POINT ( 'NONE',  ( -6.837824896291514243, 3.947820044545427454, -6.564402953523716278 ) ) ;
#26643 = CARTESIAN_POINT ( 'NONE',  ( 58.22499999726881015, 149.9369285172503510, 15.58253174999999580 ) ) ;
#26644 = CARTESIAN_POINT ( 'NONE',  ( -9.984503880673475606, 210.2968891136704315, 12.65113791807856458 ) ) ;
#26645 = CARTESIAN_POINT ( 'NONE',  ( -6.500000000000000000, 1.392044006191029304, -6.058542048163745086 ) ) ;
#26646 = CARTESIAN_POINT ( 'NONE',  ( 65.22499999726881015, 160.0630714827496206, -15.58253175000000823 ) ) ;
#26647 = CARTESIAN_POINT ( 'NONE',  ( 76.57499999726881867, 145.8408176439707802, 12.60653300113718345 ) ) ;
#26648 = CARTESIAN_POINT ( 'NONE',  ( -12.00000000000000711, 207.0476921513413515, 78.50113791807856956 ) ) ;
#26649 = LINE ( 'NONE', #24741, #16805 ) ;
#26650 = EDGE_CURVE ( 'NONE', #22495, #17155, #28693, .T. ) ;
#26651 = EDGE_CURVE ( 'NONE', #31059, #6774, #9624, .T. ) ;
#26652 = CARTESIAN_POINT ( 'NONE',  ( 6.139770520408367460, 198.4640165459539389, 98.45113791807857240 ) ) ;
#26653 = DIRECTION ( 'NONE',  ( -0.5000000000000061062, 0.000000000000000000, 0.8660254037844351549 ) ) ;
#26654 = ORIENTED_EDGE ( 'NONE', *, *, #31667, .F. ) ;
#26655 = CARTESIAN_POINT ( 'NONE',  ( -11.98450388067341876, 203.0532714938636047, 104.3488620819214532 ) ) ;
#26656 = CARTESIAN_POINT ( 'NONE',  ( -3.662846001189865142, 195.5725841191952838, 58.89886208192143613 ) ) ;
#26657 = CARTESIAN_POINT ( 'NONE',  ( -9.984503880673420539, 203.7031108863293980, 68.34886208192143897 ) ) ;
#26658 = CARTESIAN_POINT ( 'NONE',  ( -3.662846001189865142, 195.5725841191952838, 1.898862081921434131 ) ) ;
#26659 = DIRECTION ( 'NONE',  ( -0.000000000000000000, 0.8660254037844391517, 0.4999999999999990563 ) ) ;
#26660 = CARTESIAN_POINT ( 'NONE',  ( 8.118202686958039038, 212.8392687619912635, 25.70113791807856529 ) ) ;
#26661 = EDGE_CURVE ( 'NONE', #16104, #11212, #7631, .T. ) ;
#26662 = EDGE_CURVE ( 'NONE', #32153, #14133, #26488, .T. ) ;
#26663 = CARTESIAN_POINT ( 'NONE',  ( -6.220909254589682469, 215.4770327129946850, 74.94886208192143329 ) ) ;
#26664 = VERTEX_POINT ( 'NONE', #23087 ) ;
#26665 = CARTESIAN_POINT ( 'NONE',  ( -8.118202686958039038, 201.1607312380087080, 96.20113791807857240 ) ) ;
#26666 = VERTEX_POINT ( 'NONE', #1786 ) ;
#26667 =( NAMED_UNIT ( * ) PLANE_ANGLE_UNIT ( ) SI_UNIT ( $, .RADIAN. ) );
#26668 = CARTESIAN_POINT ( 'NONE',  ( -8.000000000000008882, 206.9523078486584780, 59.49886208192144466 ) ) ;
#26669 = ORIENTED_EDGE ( 'NONE', *, *, #12723, .T. ) ;
#26670 = PRODUCT_DEFINITION_SHAPE ( 'NONE', 'NONE',  #33714 ) ;
#26671 = CARTESIAN_POINT ( 'NONE',  ( 79.22499999726879594, 160.0630714827496206, -15.58253175000000823 ) ) ;
#26672 = ORIENTED_EDGE ( 'NONE', *, *, #22049, .T. ) ;
#26673 = DIRECTION ( 'NONE',  ( -1.000000000000000000, 0.000000000000000000, 0.000000000000000000 ) ) ;
#26674 = UNCERTAINTY_MEASURE_WITH_UNIT (LENGTH_MEASURE( 1.000000000000000082E-05 ), #27550, 'distance_accuracy_value', 'NONE');
#26675 = CARTESIAN_POINT ( 'NONE',  ( 72.52499999726882152, 140.1801316387863778, 4.815267126137185549 ) ) ;
#26676 = CARTESIAN_POINT ( 'NONE',  ( 4.984841277089725686, 213.7757310962907411, 73.55113791807856671 ) ) ;
#26677 = AXIS2_PLACEMENT_3D ( 'NONE', #10085, #5774, #24343 ) ;
#26678 = CARTESIAN_POINT ( 'NONE',  ( 2.249320974685011798, 30.45561873520116691, -1.706427272390174776 ) ) ;
#26679 =( LENGTH_UNIT ( ) NAMED_UNIT ( * ) SI_UNIT ( .MILLI., .METRE. ) );
#26680 = CARTESIAN_POINT ( 'NONE',  ( 37.00000000000000000, 170.2462022514548323, -7.872454543227099337E-15 ) ) ;
#26681 = CARTESIAN_POINT ( 'NONE',  ( -7.984503880673422316, 204.3529502787951628, 41.34886208192143897 ) ) ;
#26682 = CARTESIAN_POINT ( 'NONE',  ( -3.135527875058821579, 197.5041725223112223, 80.90113791807858945 ) ) ;
#26683 = CIRCLE ( 'NONE', #9676, 40.00000000000000711 ) ;
#26684 = CARTESIAN_POINT ( 'NONE',  ( 9.984503880673470277, 203.7031108863295401, 62.15113791807856813 ) ) ;
#26685 = CARTESIAN_POINT ( 'NONE',  ( 72.99495483890930814, 155.0000000000000000, -6.938893903907228378E-15 ) ) ;
#26686 = CARTESIAN_POINT ( 'NONE',  ( -0.05014649552807731031, 198.5883022060938572, 20.75113791807856600 ) ) ;
#26687 = CARTESIAN_POINT ( 'NONE',  ( -27.50000000000000355, 5.390523180938865622, -17.71625836475402238 ) ) ;
#26688 = CARTESIAN_POINT ( 'NONE',  ( -0.9108756637653833144, 6.979659189792688956, -6.219623095965475024 ) ) ;
#26689 = CARTESIAN_POINT ( 'NONE',  ( 42.82499999726880446, 141.7447067706911810, -9.630534252274387086 ) ) ;
#26690 = CARTESIAN_POINT ( 'NONE',  ( 9.736236675707914401, 214.0148392665762458, 46.70113791807857240 ) ) ;
#26691 = CARTESIAN_POINT ( 'NONE',  ( 7.922281120364393914, 4.573931137438269623, -8.047472243342930653 ) ) ;
#26692 = CARTESIAN_POINT ( 'NONE',  ( 3.135527875058820690, 216.4958274776887492, 91.40113791807857524 ) ) ;
#26693 = CARTESIAN_POINT ( 'NONE',  ( -8.118202686958039038, 201.1607312380087080, 69.20113791807858661 ) ) ;
#26694 = CARTESIAN_POINT ( 'NONE',  ( 11.98450388067341876, 210.9467285061363953, 33.84886208192142476 ) ) ;
#26695 = CARTESIAN_POINT ( 'NONE',  ( -3.135527875058982783, 216.4958274776886924, 39.09886208192143187 ) ) ;
#26696 = CARTESIAN_POINT ( 'NONE',  ( 81.89999999453763735, 150.2886644046228639, -14.50000000000000888 ) ) ;
#26697 = CARTESIAN_POINT ( 'NONE',  ( -0.05014649552807705357, 194.3824533091408000, 77.75113791807856956 ) ) ;
#26698 = CARTESIAN_POINT ( 'NONE',  ( -4.903702542908602524, 213.8346818373418898, 84.95113791807858661 ) ) ;
#26699 = CARTESIAN_POINT ( 'NONE',  ( -3.135527875058982783, 216.4958274776886924, 51.09886208192143897 ) ) ;
#26700 = DIRECTION ( 'NONE',  ( 0.000000000000000000, 0.000000000000000000, -1.000000000000000000 ) ) ;
#26702 = VERTEX_POINT ( 'NONE', #20527 ) ;
#26701 = B_SPLINE_CURVE_WITH_KNOTS ( 'NONE', 3,
 ( #4784, #33577, #10256, #23518 ),
 .UNSPECIFIED., .F., .F.,
 ( 4, 4 ),
 ( 0.000000000000000000, 0.004600009204204574646 ),
 .UNSPECIFIED. ) ;
#26703 = CARTESIAN_POINT ( 'NONE',  ( 7.375838497908012492, 217.2372850707501186, 57.54886208192142760 ) ) ;
#26704 = CIRCLE ( 'NONE', #12019, 2.149999999999994138 ) ;
#26705 = VERTEX_POINT ( 'NONE', #12188 ) ;
#26706 = CARTESIAN_POINT ( 'NONE',  ( 8.015496119326595448, 204.4483345814782638, 37.14886208192143613 ) ) ;
#26707 = ORIENTED_EDGE ( 'NONE', *, *, #6858, .F. ) ;
#26708 = CARTESIAN_POINT ( 'NONE',  ( 75.37499999726881583, 155.0000000000000000, -15.58253175000000823 ) ) ;
#26709 = DIRECTION ( 'NONE',  ( 0.000000000000000000, 0.000000000000000000, -1.000000000000000000 ) ) ;
#26710 = CARTESIAN_POINT ( 'NONE',  ( 59.48867513459483547, 167.7597621252805880, 9.270509831248428867 ) ) ;
#26711 = CARTESIAN_POINT ( 'NONE',  ( -6.444103211791042618, 211.7408657792732356, 48.80113791807858092 ) ) ;
#26712 = CARTESIAN_POINT ( 'NONE',  ( -63.49999999999884892, 217.5000000000001990, 0.000000000000000000 ) ) ;
#26713 = CARTESIAN_POINT ( 'NONE',  ( -3.135527875058982783, 216.4958274776886924, 33.09886208192143187 ) ) ;
#26714 = CARTESIAN_POINT ( 'NONE',  ( 72.57499999726880446, 145.8408176439707802, 12.60653300113718345 ) ) ;
#26715 = ORIENTED_EDGE ( 'NONE', *, *, #29583, .F. ) ;
#26716 = CARTESIAN_POINT ( 'NONE',  ( 62.78867513459482552, 155.0000000000000000, -15.00000000000002487 ) ) ;
#26717 = FILL_AREA_STYLE_COLOUR ( '', #4586 ) ;
#26718 = CARTESIAN_POINT ( 'NONE',  ( 107.5000000000000000, 155.0000000000000000, -6.938893903907228378E-15 ) ) ;
#26719 = CARTESIAN_POINT ( 'NONE',  ( -7.984503880673422316, 204.3529502787951628, 14.34886208192143364 ) ) ;
#26720 = CARTESIAN_POINT ( 'NONE',  ( 0.05014649552810505201, 217.5146222423826714, 49.25113791807857666 ) ) ;
#26721 = CARTESIAN_POINT ( 'NONE',  ( 7.922281120364393914, -4.573931137438282057, -8.047472243342932430 ) ) ;
#26722 = CARTESIAN_POINT ( 'NONE',  ( -6.220909254589537696, 198.5229672870051161, 36.05113791807857382 ) ) ;
#26723 = CARTESIAN_POINT ( 'NONE',  ( 84.17499999726882720, 164.1591823560292198, 12.60653300113718167 ) ) ;
#26724 = B_SPLINE_CURVE_WITH_KNOTS ( 'NONE', 3,
 ( #5821, #16718, #16885, #21666, #13658, #16216, #1218, #26945 ),
 .UNSPECIFIED., .F., .F.,
 ( 4, 2, 2, 4 ),
 ( 0.02832689070575900372, 0.03234239231761928957, 0.03635789392947956500, 0.04438889715320012974 ),
 .UNSPECIFIED. ) ;
#26725 = APPLICATION_PROTOCOL_DEFINITION ( 'draft international standard', 'automotive_design', 1998, #30526 ) ;
#26726 = VECTOR ( 'NONE', #22886, 1000.000000000000000 ) ;
#26727 = CARTESIAN_POINT ( 'NONE',  ( 4.984841277089891776, 200.2242689037093726, 100.4488620819214475 ) ) ;
#26728 = CARTESIAN_POINT ( 'NONE',  ( 38.22499999726881015, 149.9369285172503510, 15.58253174999999580 ) ) ;
#26729 = CARTESIAN_POINT ( 'NONE',  ( 36.08867513459483689, 142.2402378747194405, 9.270509831248432420 ) ) ;
#26730 = DIRECTION ( 'NONE',  ( -0.1461455375466716444, 0.9854922318508084755, -0.08629335326029916042 ) ) ;
#26731 = CARTESIAN_POINT ( 'NONE',  ( 7.375838497908181246, 196.7627149292499666, 20.45113791807856529 ) ) ;
#26732 = CARTESIAN_POINT ( 'NONE',  ( -9.996365641501871124, 207.8097375604742467, 102.5363179372327096 ) ) ;
#26733 = CARTESIAN_POINT ( 'NONE',  ( 56.07499999726881157, 168.2552932293087906, 9.630534252274372875 ) ) ;
#26734 = CARTESIAN_POINT ( 'NONE',  ( -3.044812012440131443, 216.5253028482142952, 64.10113791807857808 ) ) ;
#26735 = CARTESIAN_POINT ( 'NONE',  ( -8.062137200540920645, 212.9164362838581894, 36.80113791807856671 ) ) ;
#26736 = CARTESIAN_POINT ( 'NONE',  ( -7.500000000000000888, -0.7512838658081441023, 1.307818870560639724E-15 ) ) ;
#26737 = CARTESIAN_POINT ( 'NONE',  ( 13.75000000000000888, -23.81569860407206463, -18.00000000000000000 ) ) ;
#26738 = CARTESIAN_POINT ( 'NONE',  ( -8.118202686958138514, 212.8392687619910930, 8.798862081921434708 ) ) ;
#26739 = CARTESIAN_POINT ( 'NONE',  ( 60.49999999453763166, 170.2462022514548323, -7.872454543227099337E-15 ) ) ;
#26740 = ORIENTED_EDGE ( 'NONE', *, *, #11608, .T. ) ;
#26741 = CARTESIAN_POINT ( 'NONE',  ( 12.00000000000000711, 206.9523078486586485, 50.00113791807856956 ) ) ;
#26742 = DIRECTION ( 'NONE',  ( 1.000000000000000000, 0.000000000000000000, 0.000000000000000000 ) ) ;
#26743 = CARTESIAN_POINT ( 'NONE',  ( -10.01549611932659722, 210.2015048109875011, 17.64886208192143613 ) ) ;
#26744 = CARTESIAN_POINT ( 'NONE',  ( 72.41132485994282320, 167.7597621252805880, 9.270509831248428867 ) ) ;
#26745 = ORIENTED_EDGE ( 'NONE', *, *, #22871, .T. ) ;
#26746 = CARTESIAN_POINT ( 'NONE',  ( -8.118202686958039038, 201.1607312380087080, 84.20113791807858661 ) ) ;
#26747 = ORIENTED_EDGE ( 'NONE', *, *, #7049, .F. ) ;
#26748 = EDGE_CURVE ( 'NONE', #8055, #30882, #33033, .T. ) ;
#26749 = CARTESIAN_POINT ( 'NONE',  ( 83.78867513459482552, 155.0000000000000000, 15.00000000000001243 ) ) ;
#26750 = CARTESIAN_POINT ( 'NONE',  ( 66.71132485994280614, 155.0000000000000000, 15.00000000000001243 ) ) ;
#26751 = ORIENTED_EDGE ( 'NONE', *, *, #29729, .T. ) ;
#26752 = CARTESIAN_POINT ( 'NONE',  ( 2.517493886308900919, 214.5937144450984420, 25.40113791807857169 ) ) ;
#26753 = CARTESIAN_POINT ( 'NONE',  ( -60.98379214578430663, 194.9989775857802385, -0.3278793750673599239 ) ) ;
#26754 = CARTESIAN_POINT ( 'NONE',  ( -0.05014649552828403384, 217.5146222423826714, 3.248862081921433997 ) ) ;
#26755 = CARTESIAN_POINT ( 'NONE',  ( 51.07499999726880446, 141.7447067706911810, -9.630534252274387086 ) ) ;
#26756 = ORIENTED_EDGE ( 'NONE', *, *, #8750, .T. ) ;
#26757 = CARTESIAN_POINT ( 'NONE',  ( 56.72499999726881015, 140.1801316387863778, -4.815267126137194431 ) ) ;
#26758 = CARTESIAN_POINT ( 'NONE',  ( 7.500000000000000000, -4.330127018922199866, -7.422398894150035176 ) ) ;
#26759 = DIRECTION ( 'NONE',  ( 1.000000000000000000, -4.625929269271484928E-16, 0.000000000000000000 ) ) ;
#26760 = CIRCLE ( 'NONE', #24040, 6.500000000000000000 ) ;
#26761 = CARTESIAN_POINT ( 'NONE',  ( 32.50000000000000000, 155.0000000000000000, -6.938893903907228378E-15 ) ) ;
#26762 = CARTESIAN_POINT ( 'NONE',  ( -3.135527875058982783, 216.4958274776886924, 87.09886208192143897 ) ) ;
#26763 = CARTESIAN_POINT ( 'NONE',  ( 56.17499999726881299, 164.1591823560292198, 12.60653300113718167 ) ) ;
#26764 = CARTESIAN_POINT ( 'NONE',  ( -8.062137200540920645, 212.9164362838581894, 18.80113791807856671 ) ) ;
#26765 = CARTESIAN_POINT ( 'NONE',  ( -0.05014649552828442242, 219.6175466908591716, 81.24886208192143044 ) ) ;
#26766 = CARTESIAN_POINT ( 'NONE',  ( 77.00000000000001421, 170.2462022514548323, -7.872454543227099337E-15 ) ) ;
#26767 = DIRECTION ( 'NONE',  ( -1.000000000000000000, -0.000000000000000000, -0.000000000000000000 ) ) ;
#26768 = CARTESIAN_POINT ( 'NONE',  ( 61.71132485994280614, 155.0000000000000000, -15.00000000000002487 ) ) ;
#26769 = CARTESIAN_POINT ( 'NONE',  ( -0.05014649552810635652, 196.4853777576173002, 98.75113791807854113 ) ) ;
#26770 = DIRECTION ( 'NONE',  ( 0.000000000000000000, 0.000000000000000000, -1.000000000000000000 ) ) ;
#26771 = CARTESIAN_POINT ( 'NONE',  ( 39.47499999726881015, 160.0630714827496206, -15.58253175000000823 ) ) ;
#26772 = CARTESIAN_POINT ( 'NONE',  ( 8.118202686958039038, 212.8392687619912635, 40.70113791807857240 ) ) ;
#26773 = CARTESIAN_POINT ( 'NONE',  ( 78.22499999726881015, 149.9369285172503510, 15.58253174999999580 ) ) ;
#26774 = ORIENTED_EDGE ( 'NONE', *, *, #4798, .F. ) ;
#26775 =( GEOMETRIC_REPRESENTATION_CONTEXT ( 3 ) GLOBAL_UNCERTAINTY_ASSIGNED_CONTEXT ( ( #27137 ) ) GLOBAL_UNIT_ASSIGNED_CONTEXT ( ( #15341, #13121, #8020 ) ) REPRESENTATION_CONTEXT ( 'NONE', 'WORKASPACE' ) );
#26776 = DIRECTION ( 'NONE',  ( 1.000000000000000000, -0.000000000000000000, -0.000000000000000000 ) ) ;
#26777 = CARTESIAN_POINT ( 'NONE',  ( 43.09999999453763309, 150.2886644046228639, 14.49999999999999645 ) ) ;
#26778 = CARTESIAN_POINT ( 'NONE',  ( 3.662846001190051659, 195.5725841191953691, 20.60113791807856742 ) ) ;
#26779 = CARTESIAN_POINT ( 'NONE',  ( -3.499999999999996891, -1.692071238847158821, -2.682267049545485893 ) ) ;
#26780 = DIRECTION ( 'NONE',  ( 0.000000000000000000, 0.000000000000000000, 1.000000000000000000 ) ) ;
#26781 = ORIENTED_EDGE ( 'NONE', *, *, #33042, .T. ) ;
#26782 = CARTESIAN_POINT ( 'NONE',  ( -6.139770520408224463, 198.4640165459539105, 92.04886208192142760 ) ) ;
#26783 = AXIS2_PLACEMENT_3D ( 'NONE', #8384, #13321, #3257 ) ;
#26784 = CARTESIAN_POINT ( 'NONE',  ( 3.753561863808876797, 195.6020594897209719, 37.59886208192143187 ) ) ;
#26785 = DIRECTION ( 'NONE',  ( 0.000000000000000000, -0.7071067811865330288, 0.7071067811865621167 ) ) ;
#26786 = CARTESIAN_POINT ( 'NONE',  ( 0.05014649552810505201, 217.5146222423826714, 52.25113791807856245 ) ) ;
#26787 = EDGE_LOOP ( 'NONE', ( #30886, #10484 ) ) ;
#26788 = VECTOR ( 'NONE', #8606, 1000.000000000000000 ) ;
#26789 = CARTESIAN_POINT ( 'NONE',  ( -2.517493886309087880, 214.5937144450984135, 15.09886208192143719 ) ) ;
#26790 = EDGE_CURVE ( 'NONE', #6298, #5337, #9077, .T. ) ;
#26791 = B_SPLINE_CURVE_WITH_KNOTS ( 'NONE', 3,
 ( #5266, #5104, #25887, #23337, #31167, #20615 ),
 .UNSPECIFIED., .F., .F.,
 ( 4, 2, 4 ),
 ( 0.000000000000000000, 0.001990940508721409253, 0.003981881017442818506 ),
 .UNSPECIFIED. ) ;
#26792 = CARTESIAN_POINT ( 'NONE',  ( 50.18867513459482410, 140.7341522555726669, 4.635254915624211769 ) ) ;
#26793 = ORIENTED_EDGE ( 'NONE', *, *, #7429, .F. ) ;
#26794 = CARTESIAN_POINT ( 'NONE',  ( -0.05014649552828365914, 215.4116977939061144, 99.24886208192143044 ) ) ;
#26795 = B_SPLINE_CURVE_WITH_KNOTS ( 'NONE', 3,
 ( #21842, #8899, #21179, #16067, #1234, #32233 ),
 .UNSPECIFIED., .F., .F.,
 ( 4, 2, 4 ),
 ( 0.005511122051665403969, 0.007432374760074392586, 0.009353627468483380336 ),
 .UNSPECIFIED. ) ;
#26796 = CARTESIAN_POINT ( 'NONE',  ( 8.000000000000008882, 206.9523078486586485, 41.00113791807857666 ) ) ;
#26797 = EDGE_LOOP ( 'NONE', ( #2634, #28738, #17924, #31901 ) ) ;
#26798 = CARTESIAN_POINT ( 'NONE',  ( 39.32499999726881157, 164.1591823560292198, -12.60653300113719766 ) ) ;
#26799 = EDGE_CURVE ( 'NONE', #27213, #10143, #33646, .T. ) ;
#26800 = VECTOR ( 'NONE', #10917, 1000.000000000000000 ) ;
#26801 = CARTESIAN_POINT ( 'NONE',  ( -8.062137200540822946, 201.0835637161416400, 56.19886208192144039 ) ) ;
#26802 = CARTESIAN_POINT ( 'NONE',  ( 86.32499999726880446, 145.8408176439707802, 12.60653300113718345 ) ) ;
#26803 = CARTESIAN_POINT ( 'NONE',  ( -6.500000000000000000, -3.752776749732572803, -6.064240316920399998 ) ) ;
#26804 = CARTESIAN_POINT ( 'NONE',  ( -6.444103211791042618, 211.7408657792732356, 93.80113791807858092 ) ) ;
#26806 = AXIS2_PLACEMENT_3D ( 'NONE', #28850, #7402, #9959 ) ;
#26805 = DIRECTION ( 'NONE',  ( 1.000000000000000000, 0.000000000000000000, 0.000000000000000000 ) ) ;
#26807 = CARTESIAN_POINT ( 'NONE',  ( 54.69999999999999574, 163.5228861582408797, -11.73074641843674470 ) ) ;
#26808 = CARTESIAN_POINT ( 'NONE',  ( -0.05014649552828365914, 215.4116977939061144, 69.24886208192143044 ) ) ;
#26809 = LINE ( 'NONE', #3813, #18383 ) ;
#26810 = CIRCLE ( 'NONE', #31706, 0.4000000000000001887 ) ;
#26811 = ADVANCED_FACE ( 'NONE', ( #17802 ), #2841, .F. ) ;
#26812 = CIRCLE ( 'NONE', #26291, 2.149999999999985256 ) ;
#26813 = CARTESIAN_POINT ( 'NONE',  ( 55.42499999726879878, 168.2552932293087906, -9.630534252274385310 ) ) ;
#26814 = CARTESIAN_POINT ( 'NONE',  ( -6.139770520408368348, 215.5359834540460042, 9.951137918078567068 ) ) ;
#26815 = LINE ( 'NONE', #3479, #7034 ) ;
#26816 = CARTESIAN_POINT ( 'NONE',  ( 64.32499999726881867, 145.8408176439707802, 12.60653300113718345 ) ) ;
#26817 = CARTESIAN_POINT ( 'NONE',  ( 76.47499999726881015, 149.9369285172503510, 15.58253174999999580 ) ) ;
#26818 = CARTESIAN_POINT ( 'NONE',  ( -0.05014649552807705357, 194.3824533091408000, 80.75113791807856956 ) ) ;
#26819 = EDGE_CURVE ( 'NONE', #13342, #8327, #24079, .T. ) ;
#26820 = CARTESIAN_POINT ( 'NONE',  ( 8.118202686958039038, 212.8392687619912635, 100.7011379180785866 ) ) ;
#26821 = CARTESIAN_POINT ( 'NONE',  ( 84.28867513459483973, 139.2280666364260071, -4.041636747397287284E-15 ) ) ;
#26822 = ORIENTED_EDGE ( 'NONE', *, *, #10342, .T. ) ;
#26823 = CARTESIAN_POINT ( 'NONE',  ( -12.10169002831357510, 232.5389149829038331, 105.4832055762867782 ) ) ;
#26824 = CARTESIAN_POINT ( 'NONE',  ( -7.375838497908014268, 196.7627149292498530, 65.04886208192144181 ) ) ;
#26825 = AXIS2_PLACEMENT_3D ( 'NONE', #33147, #6570, #22240 ) ;
#26826 = CARTESIAN_POINT ( 'NONE',  ( 10.00000000000000711, 207.0476921513415220, 63.99886208192143044 ) ) ;
#26827 = CARTESIAN_POINT ( 'NONE',  ( -7.375838497908014268, 196.7627149292498530, 5.048862081921433820 ) ) ;
#26828 = CARTESIAN_POINT ( 'NONE',  ( 93.60208470531338776, 155.0000000000000000, -12.00000000000001066 ) ) ;
#26829 = CARTESIAN_POINT ( 'NONE',  ( -0.05014649552810635652, 196.4853777576173002, 26.75113791807856956 ) ) ;
#26830 = CARTESIAN_POINT ( 'NONE',  ( 0.05014649552828275708, 196.4853777576173002, 91.74886208192144466 ) ) ;
#26831 = ORIENTED_EDGE ( 'NONE', *, *, #15906, .F. ) ;
#26832 = CARTESIAN_POINT ( 'NONE',  ( 63.51132485994280330, 146.1832212156128890, -12.13525491562423042 ) ) ;
#26833 = CIRCLE ( 'NONE', #14312, 2.000000000000000888 ) ;
#26834 = EDGE_LOOP ( 'NONE', ( #5100, #21396 ) ) ;
#26835 = CARTESIAN_POINT ( 'NONE',  ( -63.49999999999884892, 215.0000000000003979, 0.000000000000000000 ) ) ;
#26836 = CARTESIAN_POINT ( 'NONE',  ( 6.444103211790928043, 211.7408657792734061, 66.69886208192143329 ) ) ;
#26837 = VECTOR ( 'NONE', #12137, 1000.000000000000000 ) ;
#26838 = ORIENTED_EDGE ( 'NONE', *, *, #24518, .T. ) ;
#26839 = AXIS2_PLACEMENT_3D ( 'NONE', #8236, #11459, #31570 ) ;
#26840 = CARTESIAN_POINT ( 'NONE',  ( 79.52499999726880731, 169.8198683612136222, -4.815267126137197984 ) ) ;
#26841 = VERTEX_POINT ( 'NONE', #23592 ) ;
#26842 = LINE ( 'NONE', #7964, #4283 ) ;
#26843 = CARTESIAN_POINT ( 'NONE',  ( 68.92499999726881299, 145.8408176439707802, -12.60653300113719588 ) ) ;
#26844 = CARTESIAN_POINT ( 'NONE',  ( 4.903702542908601636, 200.1653181626581102, 68.45113791807857240 ) ) ;
#26845 = EDGE_CURVE ( 'NONE', #4510, #250, #22680, .T. ) ;
#26846 = CARTESIAN_POINT ( 'NONE',  ( 67.71132485994280614, 155.0000000000000000, -15.00000000000002487 ) ) ;
#26847 = ADVANCED_FACE ( 'NONE', ( #29370 ), #31267, .T. ) ;
#26848 = CARTESIAN_POINT ( 'NONE',  ( 32.50000000000000000, 155.0000000000000000, -6.938893903907228378E-15 ) ) ;
#26849 = CARTESIAN_POINT ( 'NONE',  ( 35.40000000000000568, 159.7113355953771077, 14.49999999999999289 ) ) ;
#26850 = CARTESIAN_POINT ( 'NONE',  ( 2.517493886309087436, 199.4062855549015865, 46.59886208192143897 ) ) ;
#26851 = CARTESIAN_POINT ( 'NONE',  ( 10.01549611932653860, 210.2015048109876716, 82.85113791807854966 ) ) ;
#26852 = EDGE_CURVE ( 'NONE', #7110, #27265, #30868, .T. ) ;
#26853 = CARTESIAN_POINT ( 'NONE',  ( 3.044812012440130555, 197.4746971517856764, 62.60113791807857098 ) ) ;
#26854 = CARTESIAN_POINT ( 'NONE',  ( 0.000000000000000000, 0.000000000000000000, 3.469446951953614189E-15 ) ) ;
#26855 = CARTESIAN_POINT ( 'NONE',  ( 2.426778023690261410, 199.3768101843759837, 23.60113791807857098 ) ) ;
#26856 = CARTESIAN_POINT ( 'NONE',  ( 4.999999999999999112, 5.773502691896256422, -7.063244554129997965 ) ) ;
#26857 = PRESENTATION_LAYER_ASSIGNMENT (  '', '', ( #26308 ) ) ;
#26858 = LINE ( 'NONE', #8308, #23101 ) ;
#26859 = CARTESIAN_POINT ( 'NONE',  ( 43.62499999726880873, 171.3844434931184253, -7.942151717890134290E-15 ) ) ;
#26860 =( BOUNDED_CURVE ( )  B_SPLINE_CURVE ( 2, ( #30124, #19728, #14780, #22798, #22286, #25173, #15122, #33189, #17170, #22114, #11900 ),
 .UNSPECIFIED., .F., .T. ) 
 B_SPLINE_CURVE_WITH_KNOTS ( ( 3, 2, 2, 2, 2, 3 ),
 ( 0.9285714285714286031, 0.9321428571428571619, 0.9357142857142858317, 0.9392857142857143904, 0.9428571428571430602, 0.9464285714285716189 ),
 .UNSPECIFIED. ) 
 CURVE ( )  GEOMETRIC_REPRESENTATION_ITEM ( )  RATIONAL_B_SPLINE_CURVE ( ( 1.000000000000000000, 0.9510565162951534202, 1.000000000000000000, 0.9510565162951534202, 1.000000000000000000, 0.9510565162951534202, 1.000000000000000000, 0.9510565162951534202, 1.000000000000000000, 0.9510565162951504226, 1.000000000000003109 ) ) 
 REPRESENTATION_ITEM ( '' )  );
#26861 = CARTESIAN_POINT ( 'NONE',  ( 9.680171189290831535, 199.9079932115568852, 50.30113791807857382 ) ) ;
#26862 = CARTESIAN_POINT ( 'NONE',  ( 7.500000000000000888, -4.651016565836964212, -7.928861822685564498 ) ) ;
#26863 = CIRCLE ( 'NONE', #12747, 8.542937654374687995 ) ;
#26864 = EDGE_CURVE ( 'NONE', #6991, #9110, #8004, .T. ) ;
#26865 = CARTESIAN_POINT ( 'NONE',  ( 3.135527875058820690, 216.4958274776887492, 97.40113791807858945 ) ) ;
#26866 = CARTESIAN_POINT ( 'NONE',  ( -6.139770520408368348, 215.5359834540460042, 66.95113791807857240 ) ) ;
#26867 = CARTESIAN_POINT ( 'NONE',  ( -7.456977232089471386, 217.1783343296987709, 35.94886208192142618 ) ) ;
#26868 = CARTESIAN_POINT ( 'NONE',  ( -6.139770520408224463, 198.4640165459539105, 35.04886208192143471 ) ) ;
#26869 = CARTESIAN_POINT ( 'NONE',  ( 83.39999999453762314, 141.2096805137202580, 4.480746418436733158 ) ) ;
#26870 = CARTESIAN_POINT ( 'NONE',  ( -12.00000000000000711, 207.0476921513413515, 81.50113791807856956 ) ) ;
#26871 = CARTESIAN_POINT ( 'NONE',  ( -4.903702542908602524, 213.8346818373418898, 99.95113791807860082 ) ) ;
#26872 = CARTESIAN_POINT ( 'NONE',  ( 8.118202686958138514, 201.1607312380088501, 58.29886208192143471 ) ) ;
#26873 = SURFACE_STYLE_USAGE ( .BOTH. , #17152 ) ;
#26874 = ORIENTED_EDGE ( 'NONE', *, *, #31076, .T. ) ;
#26875 = CARTESIAN_POINT ( 'NONE',  ( -12.01549611932659722, 210.8513442034533227, 59.64886208192143613 ) ) ;
#26876 = VERTEX_POINT ( 'NONE', #8097 ) ;
#26877 = CARTESIAN_POINT ( 'NONE',  ( -2.426778023690076225, 199.3768101843759553, 31.89886208192144323 ) ) ;
#26878 = ORIENTED_EDGE ( 'NONE', *, *, #590, .F. ) ;
#26879 = EDGE_CURVE ( 'NONE', #82, #23779, #5816, .T. ) ;
#26880 = CARTESIAN_POINT ( 'NONE',  ( 79.47499999726881015, 160.0630714827496206, -15.58253175000000823 ) ) ;
#26881 = LINE ( 'NONE', #24159, #8610 ) ;
#26882 = DIRECTION ( 'NONE',  ( 1.000000000000000000, 0.000000000000000000, 0.000000000000000000 ) ) ;
#26883 = AXIS2_PLACEMENT_3D ( 'NONE', #10084, #25570, #2234 ) ;
#26884 = CARTESIAN_POINT ( 'NONE',  ( 6.500168698208129925, 211.6636982574063381, 49.70113791807857240 ) ) ;
#26885 = VECTOR ( 'NONE', #3212, 1000.000000000000000 ) ;
#26886 = CARTESIAN_POINT ( 'NONE',  ( 94.70964751525852421, 155.0000000000000000, 0.000000000000000000 ) ) ;
#26887 = CARTESIAN_POINT ( 'NONE',  ( 9.984503880673420539, 210.2968891136705167, 36.84886208192143187 ) ) ;
#26888 = CARTESIAN_POINT ( 'NONE',  ( 68.37499999726881583, 155.0000000000000000, 15.58253174999999402 ) ) ;
#26889 = ORIENTED_EDGE ( 'NONE', *, *, #24122, .F. ) ;
#26890 = LINE ( 'NONE', #3050, #3138 ) ;
#26891 = FILL_AREA_STYLE_COLOUR ( '', #12194 ) ;
#26892 = CARTESIAN_POINT ( 'NONE',  ( 52.78867513459482552, 155.0000000000000000, -15.00000000000002487 ) ) ;
#26893 = DIRECTION ( 'NONE',  ( -1.000000000000000000, 0.000000000000000000, 0.000000000000000000 ) ) ;
#26894 = CARTESIAN_POINT ( 'NONE',  ( 8.015496119326595448, 204.4483345814782638, 19.14886208192143968 ) ) ;
#26895 = CARTESIAN_POINT ( 'NONE',  ( 6.139770520408368348, 198.4640165459539674, 53.45113791807855108 ) ) ;
#26896 = CARTESIAN_POINT ( 'NONE',  ( 80.71132485994280614, 155.0000000000000000, 15.00000000000001243 ) ) ;
#26897 = CARTESIAN_POINT ( 'NONE',  ( 6.220909254589536808, 215.4770327129947702, 34.55113791807855250 ) ) ;
#26898 = CARTESIAN_POINT ( 'NONE',  ( 83.87499999726878741, 171.3844434931184253, -7.942151717890132712E-15 ) ) ;
#26899 = PRODUCT_CONTEXT ( 'NONE', #8976, 'mechanical' ) ;
#26900 =( GEOMETRIC_REPRESENTATION_CONTEXT ( 3 ) GLOBAL_UNCERTAINTY_ASSIGNED_CONTEXT ( ( #21139 ) ) GLOBAL_UNIT_ASSIGNED_CONTEXT ( ( #12744, #23134, #9672 ) ) REPRESENTATION_CONTEXT ( 'NONE', 'WORKASPACE' ) );
#26901 = CARTESIAN_POINT ( 'NONE',  ( 2.426778023690075337, 214.6231898156240447, 99.39886208192146455 ) ) ;
#26902 = CARTESIAN_POINT ( 'NONE',  ( 35.82499999726880446, 168.2552932293087906, 9.630534252274372875 ) ) ;
#26903 = CARTESIAN_POINT ( 'NONE',  ( 127.5000000000000000, 229.9533188057749555, 74.95331880577313655 ) ) ;
#26904 = DIRECTION ( 'NONE',  ( 0.000000000000000000, 0.000000000000000000, -1.000000000000000000 ) ) ;
#26905 = CARTESIAN_POINT ( 'NONE',  ( -3.662846001190052991, 218.4274158808045740, 16.10113791807856742 ) ) ;
#26906 = DIRECTION ( 'NONE',  ( 1.000000000000000000, 0.000000000000000000, 0.000000000000000000 ) ) ;
#26907 = CARTESIAN_POINT ( 'NONE',  ( 64.97499999726881015, 140.1801316387863778, -4.815267126137194431 ) ) ;
#26908 = CARTESIAN_POINT ( 'NONE',  ( -10.01549611932653860, 203.7984951890123284, 66.35113791807853545 ) ) ;
#26909 = CARTESIAN_POINT ( 'NONE',  ( 8.118202686958039038, 212.8392687619912635, 40.70113791807857240 ) ) ;
#26910 = LINE ( 'NONE', #26565, #7780 ) ;
#26911 = DIRECTION ( 'NONE',  ( -1.000000000000000000, 0.000000000000000000, 0.000000000000000000 ) ) ;
#26912 = CARTESIAN_POINT ( 'NONE',  ( -12.01549611932652972, 203.1486557965464499, 102.3511379180785639 ) ) ;
#26913 = CARTESIAN_POINT ( 'NONE',  ( 3.135527875058981895, 197.5041725223112792, 10.59886208192143542 ) ) ;
#26914 = CARTESIAN_POINT ( 'NONE',  ( 65.09999999453764019, 150.2886644046228639, 14.49999999999999645 ) ) ;
#26915 = ORIENTED_EDGE ( 'NONE', *, *, #6806, .T. ) ;
#26916 = CARTESIAN_POINT ( 'NONE',  ( 7.375838497908181246, 196.7627149292499666, 44.45113791807857240 ) ) ;
#26917 = CARTESIAN_POINT ( 'NONE',  ( 8.015496119326531499, 209.5516654185219636, 64.85113791807857808 ) ) ;
#26918 = CARTESIAN_POINT ( 'NONE',  ( 37.08867513459482268, 167.7597621252805880, -9.270509831248443078 ) ) ;
#26919 = CARTESIAN_POINT ( 'NONE',  ( 6.139770520408223575, 215.5359834540460611, 21.54886208192143826 ) ) ;
#26920 = CARTESIAN_POINT ( 'NONE',  ( 59.51132485994281041, 146.1832212156128890, -12.13525491562423042 ) ) ;
#26921 = EDGE_LOOP ( 'NONE', ( #16604, #33678 ) ) ;
#26922 = CARTESIAN_POINT ( 'NONE',  ( 3.135527875058820690, 216.4958274776887492, 76.40113791807857524 ) ) ;
#26923 = ORIENTED_EDGE ( 'NONE', *, *, #19325, .F. ) ;
#26924 = CARTESIAN_POINT ( 'NONE',  ( 33.24999999726880873, 155.0000000000000000, -15.58253175000000823 ) ) ;
#26925 = CARTESIAN_POINT ( 'NONE',  ( -4.444974277458378253, -4.939246403833585042, -5.720331885005373707 ) ) ;
#26926 = VERTEX_POINT ( 'NONE', #18805 ) ;
#26927 = CARTESIAN_POINT ( 'NONE',  ( -7.984503880673488041, 209.6470497212046098, 21.65113791807856813 ) ) ;
#26928 = CARTESIAN_POINT ( 'NONE',  ( -60.74744875717816939, 194.9849611312037041, -1.107162489773501513 ) ) ;
#26929 = CARTESIAN_POINT ( 'NONE',  ( 8.118202686958138514, 201.1607312380088501, 7.298862081921435596 ) ) ;
#26930 = CARTESIAN_POINT ( 'NONE',  ( 48.87499999726880873, 138.6155565068815747, -3.929120461958505118E-15 ) ) ;
#26931 = ORIENTED_EDGE ( 'NONE', *, *, #23649, .F. ) ;
#26932 = CARTESIAN_POINT ( 'NONE',  ( 59.52499999726881441, 169.8198683612136222, -4.815267126137197984 ) ) ;
#26933 = CARTESIAN_POINT ( 'NONE',  ( 64.50000000000000000, -103.0000000000000000, 30.00000000000000000 ) ) ;
#26934 = CARTESIAN_POINT ( 'NONE',  ( 7.922281120364393914, 4.573931137438269623, -8.047472243342930653 ) ) ;
#26935 = FACE_OUTER_BOUND ( 'NONE', #9490, .T. ) ;
#26936 = CARTESIAN_POINT ( 'NONE',  ( -6.220909254589682469, 215.4770327129946850, 89.94886208192140487 ) ) ;
#26937 = CARTESIAN_POINT ( 'NONE',  ( 57.87499999726880873, 171.3844434931184253, -7.942151717890132712E-15 ) ) ;
#26938 = CARTESIAN_POINT ( 'NONE',  ( -8.118202686958039038, 201.1607312380087080, 21.20113791807856529 ) ) ;
#26939 = DIRECTION ( 'NONE',  ( 0.000000000000000000, 0.000000000000000000, 1.000000000000000000 ) ) ;
#26940 = CARTESIAN_POINT ( 'NONE',  ( -3.753561863808878130, 218.3979405102790281, 78.09886208192142476 ) ) ;
#26941 = CARTESIAN_POINT ( 'NONE',  ( 73.09999999999999432, 168.7903194862797420, 4.480746418436729606 ) ) ;
#26942 = CARTESIAN_POINT ( 'NONE',  ( 61.91132485994280898, 163.8167787843871110, -12.13525491562423397 ) ) ;
#26943 = CYLINDRICAL_SURFACE ( 'NONE', #22946, 15.00000000000001776 ) ;
#26944 = CARTESIAN_POINT ( 'NONE',  ( 6.139770520408368348, 198.4640165459539674, 95.45113791807855819 ) ) ;
#26945 = CARTESIAN_POINT ( 'NONE',  ( 27.50000000000000355, 0.000000000000000000, -18.00000000000000000 ) ) ;
#26946 = CARTESIAN_POINT ( 'NONE',  ( 46.77499999726881441, 140.1801316387863778, 4.815267126137185549 ) ) ;
#26947 = CARTESIAN_POINT ( 'NONE',  ( 10.00000000000000711, 206.9523078486586201, 38.00113791807857666 ) ) ;
#26948 = EDGE_CURVE ( 'NONE', #33071, #18396, #26635, .T. ) ;
#26949 = CARTESIAN_POINT ( 'NONE',  ( 78.92499999726881299, 145.8408176439707802, -12.60653300113719588 ) ) ;
#26950 = ORIENTED_EDGE ( 'NONE', *, *, #14769, .T. ) ;
#26951 = DIRECTION ( 'NONE',  ( 1.000000000000000000, 0.000000000000000000, 0.000000000000000000 ) ) ;
#26952 = CARTESIAN_POINT ( 'NONE',  ( 38.99999999453762456, 155.0000000000000000, 14.49999999999999467 ) ) ;
#26953 = CARTESIAN_POINT ( 'NONE',  ( 3.753561863808689836, 218.3979405102790565, 19.40113791807856813 ) ) ;
#26954 = CARTESIAN_POINT ( 'NONE',  ( 89.50000000000002842, 155.0000000000000000, -32.00000000000002842 ) ) ;
#26955 = CARTESIAN_POINT ( 'NONE',  ( -2.621328321948020346, -7.606199919102354379, -7.633618187056584681 ) ) ;
#26956 = ORIENTED_EDGE ( 'NONE', *, *, #33465, .F. ) ;
#26957 = CARTESIAN_POINT ( 'NONE',  ( -11.98450388067341876, 203.0532714938636047, 32.34886208192142476 ) ) ;
#26958 = DIRECTION ( 'NONE',  ( 0.000000000000000000, 0.000000000000000000, -1.000000000000000000 ) ) ;
#26959 = CARTESIAN_POINT ( 'NONE',  ( -6.220909254589537696, 198.5229672870051161, 54.05113791807856671 ) ) ;
#26960 = ORIENTED_EDGE ( 'NONE', *, *, #22078, .F. ) ;
#26961 = CARTESIAN_POINT ( 'NONE',  ( -0.05014649552828365914, 215.4116977939061144, 15.24886208192143577 ) ) ;
#26962 = DIRECTION ( 'NONE',  ( -1.000000000000000000, 0.000000000000000000, 0.000000000000000000 ) ) ;
#26963 = ORIENTED_EDGE ( 'NONE', *, *, #26191, .F. ) ;
#26964 = CARTESIAN_POINT ( 'NONE',  ( 8.015496119326595448, 204.4483345814782638, 100.1488620819214646 ) ) ;
#26965 = CARTESIAN_POINT ( 'NONE',  ( -2.517493886308901807, 199.4062855549015012, 35.90113791807856813 ) ) ;
#26966 = DIRECTION ( 'NONE',  ( -1.000000000000000000, -0.000000000000000000, -0.000000000000000000 ) ) ;
#26967 = ORIENTED_EDGE ( 'NONE', *, *, #7308, .F. ) ;
#26968 = CARTESIAN_POINT ( 'NONE',  ( 39.92499999726881299, 164.1591823560292198, 12.60653300113718167 ) ) ;
#26969 = CARTESIAN_POINT ( 'NONE',  ( 3.044812012439969795, 216.5253028482143520, 60.39886208192143613 ) ) ;
#26970 = CARTESIAN_POINT ( 'NONE',  ( 41.67499999726881299, 168.2552932293087906, -9.630534252274385310 ) ) ;
#26971 = CARTESIAN_POINT ( 'NONE',  ( 0.000000000000000000, 0.000000000000000000, 3.469446951953614189E-15 ) ) ;
#26972 = CARTESIAN_POINT ( 'NONE',  ( -0.05014649552807731031, 198.5883022060938572, 101.7511379180785696 ) ) ;
#26973 = CARTESIAN_POINT ( 'NONE',  ( 52.10000000000000142, 141.2096805137202580, -4.480746418436742040 ) ) ;
#26974 = CARTESIAN_POINT ( 'NONE',  ( 4.903702542908435547, 213.8346818373419751, 75.54886208192142760 ) ) ;
#26975 = CARTESIAN_POINT ( 'NONE',  ( 76.78867513459483973, 155.0000000000000000, -15.00000000000002487 ) ) ;
#26976 = CARTESIAN_POINT ( 'NONE',  ( 6.837824896291514243, 3.947820044545427454, -6.564402953523716278 ) ) ;
#26977 = ADVANCED_FACE ( 'NONE', ( #581 ), #29804, .F. ) ;
#26978 = CARTESIAN_POINT ( 'NONE',  ( 55.52499999726881441, 169.8198683612136222, -4.815267126137197984 ) ) ;
#26980 = VERTEX_POINT ( 'NONE', #10154 ) ;
#26979 = CARTESIAN_POINT ( 'NONE',  ( -6.220909254589537696, 198.5229672870051445, 15.05113791807856494 ) ) ;
#26981 = CARTESIAN_POINT ( 'NONE',  ( 117.5000000000000000, 155.0000000000000000, 97.99999999999997158 ) ) ;
#26982 = CARTESIAN_POINT ( 'NONE',  ( 67.72499999726881015, 169.8198683612136222, 4.815267126137181997 ) ) ;
#26983 = CARTESIAN_POINT ( 'NONE',  ( 78.37499999726883004, 155.0000000000000000, 15.58253174999999402 ) ) ;
#26984 = CARTESIAN_POINT ( 'NONE',  ( -3.662846001190052991, 218.4274158808045740, 79.10113791807857808 ) ) ;
#26985 = EDGE_CURVE ( 'NONE', #31219, #5170, #1673, .T. ) ;
#26986 = CARTESIAN_POINT ( 'NONE',  ( -10.00000000000000711, 207.0476921513413515, 96.50113791807856956 ) ) ;
#26987 = CARTESIAN_POINT ( 'NONE',  ( 84.78867513459482552, 155.0000000000000000, -15.00000000000002487 ) ) ;
#26988 = VECTOR ( 'NONE', #6542, 1000.000000000000000 ) ;
#26989 = EDGE_CURVE ( 'NONE', #12552, #16947, #6916, .T. ) ;
#26990 = ORIENTED_EDGE ( 'NONE', *, *, #30439, .F. ) ;
#26991 = CARTESIAN_POINT ( 'NONE',  ( 8.062137200540822946, 212.9164362838583315, 6.698862081921435063 ) ) ;
#26992 = CARTESIAN_POINT ( 'NONE',  ( 3.662846001189864698, 218.4274158808046593, 57.39886208192143613 ) ) ;
#26993 = CLOSED_SHELL ( 'NONE', ( #32289, #27292, #2846, #29299, #29542, #8156, #22475, #6896, #10726, #10610, #25834, #15860, #24162, #791, #1793, #14782, #12902, #3542, #15781, #9293, #10398, #13132, #30641, #11666, #21329, #24779, #20764, #13130, #14872, #20355 ) ) ;
#26994 = CARTESIAN_POINT ( 'NONE',  ( 9.984503880673420539, 210.2968891136705736, 66.84886208192142476 ) ) ;
#26995 = CARTESIAN_POINT ( 'NONE',  ( 12.01549611932659367, 203.1486557965466773, 1.148862081921433909 ) ) ;
#26996 = CARTESIAN_POINT ( 'NONE',  ( -3.250000000000003997, -5.629165124598849879, 0.000000000000000000 ) ) ;
#26997 = CARTESIAN_POINT ( 'NONE',  ( 10.00000000000000711, 206.9523078486586201, 23.00113791807856600 ) ) ;
#26998 = CARTESIAN_POINT ( 'NONE',  ( 3.044812012439969795, 216.5253028482143520, 87.39886208192143613 ) ) ;
#27000 = ORIENTED_EDGE ( 'NONE', *, *, #5845, .T. ) ;
#26999 = AXIS2_PLACEMENT_3D ( 'NONE', #33359, #32840, #20234 ) ;
#27001 = DIRECTION ( 'NONE',  ( 1.000000000000000000, 0.000000000000000000, 0.000000000000000000 ) ) ;
#27002 = ORIENTED_EDGE ( 'NONE', *, *, #27020, .F. ) ;
#27003 = FACE_OUTER_BOUND ( 'NONE', #25883, .T. ) ;
#27004 = CARTESIAN_POINT ( 'NONE',  ( -7.984503880673422316, 204.3529502787951628, 68.34886208192142476 ) ) ;
#27005 = ORIENTED_EDGE ( 'NONE', *, *, #26625, .F. ) ;
#27006 = EDGE_CURVE ( 'NONE', #19514, #22398, #24683, .T. ) ;
#27007 = CARTESIAN_POINT ( 'NONE',  ( 85.12499999726881583, 155.0000000000000000, -15.58253175000000823 ) ) ;
#27008 = ORIENTED_EDGE ( 'NONE', *, *, #4398, .T. ) ;
#27009 = CARTESIAN_POINT ( 'NONE',  ( 0.000000000000000000, 0.000000000000000000, -2.899999999999999911 ) ) ;
#27010 = EDGE_CURVE ( 'NONE', #32735, #7971, #18066, .T. ) ;
#27011 = CARTESIAN_POINT ( 'NONE',  ( 78.22499999726881015, 149.9369285172503510, 15.58253174999999580 ) ) ;
#27012 = CARTESIAN_POINT ( 'NONE',  ( -2.426778023690262742, 214.6231898156240163, 70.10113791807857808 ) ) ;
#27013 = DIRECTION ( 'NONE',  ( 0.000000000000000000, 0.04769215134145521340, 0.9988620819214352187 ) ) ;
#27014 = COLOUR_RGB ( '', 0.09019608, 0.27058824, 0.51372549) ;
#27015 =( GEOMETRIC_REPRESENTATION_CONTEXT ( 3 ) GLOBAL_UNCERTAINTY_ASSIGNED_CONTEXT ( ( #5888 ) ) GLOBAL_UNIT_ASSIGNED_CONTEXT ( ( #26387, #14104, #11392 ) ) REPRESENTATION_CONTEXT ( 'NONE', 'WORKASPACE' ) );
#27016 = CARTESIAN_POINT ( 'NONE',  ( 32.80000000000000426, 167.3344367211045096, -8.961492836873482304 ) ) ;
#27017 = CARTESIAN_POINT ( 'NONE',  ( -0.05014649552828365914, 215.4116977939061144, 45.24886208192144466 ) ) ;
#27018 = CARTESIAN_POINT ( 'NONE',  ( 8.062137200540920645, 201.0835637161417822, 89.30113791807858092 ) ) ;
#27019 = CARTESIAN_POINT ( 'NONE',  ( -6.220909254589537696, 198.5229672870051161, 69.05113791807858092 ) ) ;
#27020 = EDGE_CURVE ( 'NONE', #12770, #14229, #21531, .T. ) ;
#27021 = AXIS2_PLACEMENT_3D ( 'NONE', #30585, #7249, #7758 ) ;
#27022 = CARTESIAN_POINT ( 'NONE',  ( -64.50000000000000000, 120.3589838486224579, -20.00000000000000000 ) ) ;
#27023 = CARTESIAN_POINT ( 'NONE',  ( -7.984503880673488041, 209.6470497212046098, 21.65113791807856813 ) ) ;
#27024 = CARTESIAN_POINT ( 'NONE',  ( -27.50000000000000000, 0.000000000000000000, -18.00000000000000000 ) ) ;
#27025 = CYLINDRICAL_SURFACE ( 'NONE', #29078, 2.149999999999999023 ) ;
#27026 = CARTESIAN_POINT ( 'NONE',  ( 46.52499999726881441, 140.1801316387863778, 4.815267126137185549 ) ) ;
#27027 = CARTESIAN_POINT ( 'NONE',  ( -7.375838497908182134, 217.2372850707499765, 48.95113791807855108 ) ) ;
#27028 = CARTESIAN_POINT ( 'NONE',  ( 7.897836333153806621, 1.530409084195003988, -7.633857274177628049 ) ) ;
#27029 = CARTESIAN_POINT ( 'NONE',  ( -6.139770520408369237, 215.5359834540460042, 90.95113791807854398 ) ) ;
#27030 = CARTESIAN_POINT ( 'NONE',  ( 6.139770520408367460, 198.4640165459539389, 71.45113791807857240 ) ) ;
#27031 = CARTESIAN_POINT ( 'NONE',  ( 11.98450388067341876, 210.9467285061363953, 36.84886208192142476 ) ) ;
#27032 = CARTESIAN_POINT ( 'NONE',  ( -9.984503880673420539, 203.7031108863293980, 41.34886208192143187 ) ) ;
#27033 = CARTESIAN_POINT ( 'NONE',  ( 88.99999999453763166, 155.0000000000000000, 14.49999999999999467 ) ) ;
#27034 = CARTESIAN_POINT ( 'NONE',  ( 3.662846001190051659, 195.5725841191953691, 80.60113791807857808 ) ) ;
#27035 = AXIS2_PLACEMENT_3D ( 'NONE', #16266, #19327, #27167 ) ;
#27036 = CARTESIAN_POINT ( 'NONE',  ( -8.000000000000008882, 207.0476921513413515, 93.50113791807858377 ) ) ;
#27037 = ADVANCED_FACE ( 'NONE', ( #22118 ), #19895, .T. ) ;
#27038 = CARTESIAN_POINT ( 'NONE',  ( -10.00000000000000711, 206.9523078486584495, 59.49886208192143755 ) ) ;
#27039 = CARTESIAN_POINT ( 'NONE',  ( 0.000000000000000000, 0.000000000000000000, -1.540456584061364431 ) ) ;
#27040 = ORIENTED_EDGE ( 'NONE', *, *, #5398, .F. ) ;
#27041 = CARTESIAN_POINT ( 'NONE',  ( 3.662846001189864698, 218.4274158808046593, 60.39886208192143613 ) ) ;
#27042 = PRESENTATION_LAYER_ASSIGNMENT (  '', '', ( #11796 ) ) ;
#27043 = VERTEX_POINT ( 'NONE', #15256 ) ;
#27044 = CARTESIAN_POINT ( 'NONE',  ( 73.37499999726881583, 155.0000000000000000, -15.58253175000000823 ) ) ;
#27045 = CARTESIAN_POINT ( 'NONE',  ( -6.444103211790928043, 202.2591342207265939, 41.19886208192144750 ) ) ;
#27046 = EDGE_LOOP ( 'NONE', ( #16980, #22194, #24032, #32194, #21706 ) ) ;
#27047 = EDGE_CURVE ( 'NONE', #4795, #19546, #382, .T. ) ;
#27048 = CIRCLE ( 'NONE', #31420, 1.650000000000000133 ) ;
#27049 = CARTESIAN_POINT ( 'NONE',  ( 85.27499999726879309, 149.9369285172503510, -15.58253175000000823 ) ) ;
#27050 = DIRECTION ( 'NONE',  ( 1.000000000000000000, 0.000000000000000000, 0.000000000000000000 ) ) ;
#27051 = CARTESIAN_POINT ( 'NONE',  ( 59.68867513459483121, 159.8737954434935489, 15.00000000000006040 ) ) ;
#27052 = CARTESIAN_POINT ( 'NONE',  ( 0.05014649552807626948, 215.4116977939061144, 52.25113791807857666 ) ) ;
#27053 = FACE_OUTER_BOUND ( 'NONE', #23698, .T. ) ;
#27054 = CARTESIAN_POINT ( 'NONE',  ( 10.00000000000000711, 207.0476921513415220, 36.99886208192143755 ) ) ;
#27055 = CARTESIAN_POINT ( 'NONE',  ( 67.47499999726881015, 160.0630714827496206, -15.58253175000000823 ) ) ;
#27056 = ORIENTED_EDGE ( 'NONE', *, *, #18266, .F. ) ;
#27057 = DIRECTION ( 'NONE',  ( -1.000000000000000000, 0.000000000000000000, 0.000000000000000000 ) ) ;
#27058 = FACE_OUTER_BOUND ( 'NONE', #27541, .T. ) ;
#27059 = DIRECTION ( 'NONE',  ( 0.000000000000000000, 1.000000000000000000, 0.000000000000000000 ) ) ;
#27060 = CARTESIAN_POINT ( 'NONE',  ( -2.426778023690076225, 199.3768101843759553, 16.89886208192143613 ) ) ;
#27061 = VECTOR ( 'NONE', #21562, 1000.000000000000114 ) ;
#27062 = CARTESIAN_POINT ( 'NONE',  ( 10.01549611932653860, 210.2015048109876716, 61.85113791807857098 ) ) ;
#27063 = CARTESIAN_POINT ( 'NONE',  ( -10.01549611932653860, 203.7984951890123284, 33.35113791807855677 ) ) ;
#27064 = CARTESIAN_POINT ( 'NONE',  ( 81.87499999726880162, 171.3844434931184253, -7.942151717890132712E-15 ) ) ;
#27065 = ITEM_DEFINED_TRANSFORMATION ( 'NONE', 'NONE', #24622,  #2404 ) ;
#27066 = AXIS2_PLACEMENT_3D ( 'NONE', #5759, #16152, #5928 ) ;
#27067 = CARTESIAN_POINT ( 'NONE',  ( 6.444103211791042618, 202.2591342207267644, -0.6988620819214341751 ) ) ;
#27068 = CARTESIAN_POINT ( 'NONE',  ( 47.92499999726881299, 164.1591823560292198, 12.60653300113718167 ) ) ;
#27069 = CARTESIAN_POINT ( 'NONE',  ( 54.30000000000001137, -88.00000000000000000, 30.00000000000000000 ) ) ;
#27070 = DIRECTION ( 'NONE',  ( -1.000000000000000000, 0.000000000000000000, 0.000000000000000000 ) ) ;
#27071 = CARTESIAN_POINT ( 'NONE',  ( 9.680171189290831535, 199.9079932115568852, 23.30113791807857027 ) ) ;
#27072 = CARTESIAN_POINT ( 'NONE',  ( 5.112021521198788498, -5.708827036477115868, -7.069802615102037890 ) ) ;
#27073 = CARTESIAN_POINT ( 'NONE',  ( -8.062137200540920645, 212.9164362838581894, 63.80113791807858092 ) ) ;
#27074 = CARTESIAN_POINT ( 'NONE',  ( 10.01549611932653860, 210.2015048109876716, 43.85113791807856387 ) ) ;
#27075 = AXIS2_PLACEMENT_3D ( 'NONE', #7180, #6838, #30009 ) ;
#27076 = DIRECTION ( 'NONE',  ( -0.3500148194780949296, -0.04467534437043436946, 0.9356782244720136532 ) ) ;
#27077 = CARTESIAN_POINT ( 'NONE',  ( 1.734723475976807094E-14, 31.75426480542944319, -15.54379906938135214 ) ) ;
#27078 = CARTESIAN_POINT ( 'NONE',  ( 12.00000000000000711, 207.0476921513415220, 6.998862081921433997 ) ) ;
#27079 = CARTESIAN_POINT ( 'NONE',  ( -0.05014649552828402690, 217.5146222423826714, 9.248862081921433997 ) ) ;
#27080 = CARTESIAN_POINT ( 'NONE',  ( 67.69999999453763451, 142.6655632788954620, -8.961492836873480528 ) ) ;
#27081 = ORIENTED_EDGE ( 'NONE', *, *, #32237, .T. ) ;
#27082 = CARTESIAN_POINT ( 'NONE',  ( 7.375838497908181246, 196.7627149292499666, 47.45113791807857950 ) ) ;
#27083 = CARTESIAN_POINT ( 'NONE',  ( -6.444103211791042618, 211.7408657792732356, 69.80113791807856671 ) ) ;
#27084 = EDGE_CURVE ( 'NONE', #23379, #20617, #6304, .T. ) ;
#27085 = CARTESIAN_POINT ( 'NONE',  ( 5.000000000000000888, 0.000000000000000000, -10.00000000000000000 ) ) ;
#27086 = CARTESIAN_POINT ( 'NONE',  ( -3.044812012439970683, 197.4746971517856196, 34.89886208192143613 ) ) ;
#27087 = ADVANCED_FACE ( 'NONE', ( #32673 ), #19416, .T. ) ;
#27088 = DIRECTION ( 'NONE',  ( 1.000000000000000000, -0.000000000000000000, -0.000000000000000000 ) ) ;
#27089 = EDGE_LOOP ( 'NONE', ( #25052, #28978 ) ) ;
#27090 = CARTESIAN_POINT ( 'NONE',  ( -6.220909254589537696, 198.5229672870051161, 81.05113791807856671 ) ) ;
#27091 = CIRCLE ( 'NONE', #12977, 5.249999999999991118 ) ;
#27092 = PRODUCT_RELATED_PRODUCT_CATEGORY ( 'part', '', ( #14029 ) ) ;
#27093 = ORIENTED_EDGE ( 'NONE', *, *, #20351, .F. ) ;
#27094 = ADVANCED_FACE ( 'NONE', ( #4224 ), #13364, .F. ) ;
#27095 = PLANE ( 'NONE',  #971 ) ;
#27096 = AXIS2_PLACEMENT_3D ( 'NONE', #623, #15955, #5891 ) ;
#27097 = CARTESIAN_POINT ( 'NONE',  ( -4.574783636564919931, -5.228990388887469365, -6.171384342982607407 ) ) ;
#27098 = ORIENTED_EDGE ( 'NONE', *, *, #29781, .F. ) ;
#27099 = CARTESIAN_POINT ( 'NONE',  ( 8.015496119326531499, 209.5516654185219636, 25.85113791807856742 ) ) ;
#27100 = DIRECTION ( 'NONE',  ( 1.000000000000000000, 0.000000000000000000, 0.000000000000000000 ) ) ;
#27101 = CARTESIAN_POINT ( 'NONE',  ( -8.118202686958138514, 212.8392687619910930, 8.798862081921434708 ) ) ;
#27102 = CARTESIAN_POINT ( 'NONE',  ( 47.47499999726881015, 160.0630714827496206, -15.58253175000000823 ) ) ;
#27104 = ORIENTED_EDGE ( 'NONE', *, *, #14090, .T. ) ;
#27103 = VECTOR ( 'NONE', #12457, 1000.000000000000000 ) ;
#27105 = CARTESIAN_POINT ( 'NONE',  ( 57.32499999726881157, 164.1591823560292198, -12.60653300113719766 ) ) ;
#27106 = CARTESIAN_POINT ( 'NONE',  ( -2.426778023690262742, 214.6231898156240163, 52.10113791807857808 ) ) ;
#27107 = LINE ( 'NONE', #8538, #23784 ) ;
#27108 = FILL_AREA_STYLE_COLOUR ( '', #2939 ) ;
#27109 = CARTESIAN_POINT ( 'NONE',  ( 0.000000000000000000, 0.000000000000000000, 3.099999999999998757 ) ) ;
#27110 = CARTESIAN_POINT ( 'NONE',  ( -8.062137200540822946, 201.0835637161416400, 92.19886208192143329 ) ) ;
#27111 = CARTESIAN_POINT ( 'NONE',  ( 59.77499999726881441, 169.8198683612136222, -4.815267126137197984 ) ) ;
#27112 = CARTESIAN_POINT ( 'NONE',  ( -6.220909254589537696, 198.5229672870051161, 21.05113791807855961 ) ) ;
#27113 = DIRECTION ( 'NONE',  ( 0.000000000000000000, -0.7071067811865540120, -0.7071067811865411334 ) ) ;
#27114 = CARTESIAN_POINT ( 'NONE',  ( -7.375838497908014268, 196.7627149292498530, 77.04886208192142760 ) ) ;
#27115 = CARTESIAN_POINT ( 'NONE',  ( 82.50000000000000000, 155.0000000000000000, -14.50000000000000711 ) ) ;
#27116 = CARTESIAN_POINT ( 'NONE',  ( 62.21132485994281325, 170.7719333635740497, -7.904646289410545231E-15 ) ) ;
#27117 = CARTESIAN_POINT ( 'NONE',  ( 67.50000000000000000, 155.0000000000000000, 13.49999999999996270 ) ) ;
#27118 = CARTESIAN_POINT ( 'NONE',  ( 6.220909254589536808, 215.4770327129947702, 97.55113791807855250 ) ) ;
#27119 = AXIS2_PLACEMENT_3D ( 'NONE', #32084, #27474, #1084 ) ;
#27120 = DIRECTION ( 'NONE',  ( -1.000000000000000000, -0.000000000000000000, -0.000000000000000000 ) ) ;
#27121 = CARTESIAN_POINT ( 'NONE',  ( 46.47499999726880304, 149.9369285172503510, 15.58253174999999580 ) ) ;
#27122 = CARTESIAN_POINT ( 'NONE',  ( -0.05014649552810635652, 196.4853777576173002, 41.75113791807855534 ) ) ;
#27123 = AXIS2_PLACEMENT_3D ( 'NONE', #16651, #12222, #22610 ) ;
#27124 = CARTESIAN_POINT ( 'NONE',  ( 77.52499999726880731, 169.8198683612136222, -4.815267126137197984 ) ) ;
#27125 = VERTEX_POINT ( 'NONE', #8106 ) ;
#27126 = CARTESIAN_POINT ( 'NONE',  ( -1.305263714129178521, 8.377797850839286298, -7.792447862505335721 ) ) ;
#27127 = CARTESIAN_POINT ( 'NONE',  ( 47.69999999453762740, 142.6655632788954620, -8.961492836873480528 ) ) ;
#27128 = CARTESIAN_POINT ( 'NONE',  ( -11.98450388067348804, 210.9467285061362247, 18.65113791807856458 ) ) ;
#27129 = DIRECTION ( 'NONE',  ( 1.000000000000000000, 0.000000000000000000, 0.000000000000000000 ) ) ;
#27130 = CARTESIAN_POINT ( 'NONE',  ( 0.000000000000000000, 2.342598717236900718, -4.057500000000001883 ) ) ;
#27131 = ORIENTED_EDGE ( 'NONE', *, *, #8963, .F. ) ;
#27132 = CARTESIAN_POINT ( 'NONE',  ( -12.00000000000000711, 206.9523078486584780, 38.49886208192143044 ) ) ;
#27133 = DIRECTION ( 'NONE',  ( 1.000000000000000000, 0.000000000000000000, 0.000000000000000000 ) ) ;
#27134 = CARTESIAN_POINT ( 'NONE',  ( -8.062137200540920645, 212.9164362838581894, 51.80113791807857382 ) ) ;
#27135 = EDGE_LOOP ( 'NONE', ( #18563, #26174, #3124 ) ) ;
#27136 = CARTESIAN_POINT ( 'NONE',  ( 2.426778023690075337, 214.6231898156240447, 9.398862081921436129 ) ) ;
#27137 = UNCERTAINTY_MEASURE_WITH_UNIT (LENGTH_MEASURE( 1.000000000000000082E-05 ), #15341, 'distance_accuracy_value', 'NONE');
#27138 = CARTESIAN_POINT ( 'NONE',  ( 79.68867513459481700, 159.8737954434934920, 15.00000000000007994 ) ) ;
#27139 = VERTEX_POINT ( 'NONE', #23759 ) ;
#27140 = CARTESIAN_POINT ( 'NONE',  ( -6.444103211790928043, 202.2591342207265939, 104.1988620819214475 ) ) ;
#27141 = VECTOR ( 'NONE', #19831, 1000.000000000000000 ) ;
#27142 = CYLINDRICAL_SURFACE ( 'NONE', #16475, 15.00000000000001776 ) ;
#27143 = CARTESIAN_POINT ( 'NONE',  ( 4.984841277089725686, 213.7757310962907411, 40.55113791807856671 ) ) ;
#27144 = LINE ( 'NONE', #13857, #27643 ) ;
#27145 = EDGE_LOOP ( 'NONE', ( #21729, #15655, #22981, #391 ) ) ;
#27146 = CARTESIAN_POINT ( 'NONE',  ( 40.82499999726880446, 141.7447067706911810, -9.630534252274385310 ) ) ;
#27147 = VECTOR ( 'NONE', #22756, 1000.000000000000000 ) ;
#27148 = CARTESIAN_POINT ( 'NONE',  ( -31.74999999999995737, 2.449293598294707893E-16, -2.000000000000000888 ) ) ;
#27149 = CARTESIAN_POINT ( 'NONE',  ( 6.220909254589681581, 198.5229672870052582, 64.44886208192143329 ) ) ;
#27150 = CARTESIAN_POINT ( 'NONE',  ( 43.17499999726881299, 145.8408176439707802, -12.60653300113719588 ) ) ;
#27151 = DIRECTION ( 'NONE',  ( 0.000000000000000000, 0.000000000000000000, 1.000000000000000000 ) ) ;
#27152 = CARTESIAN_POINT ( 'NONE',  ( 6.500168698208129925, 211.6636982574063381, 97.70113791807858661 ) ) ;
#27153 = AXIS2_PLACEMENT_3D ( 'NONE', #10835, #3154, #23609 ) ;
#27154 = CARTESIAN_POINT ( 'NONE',  ( 54.50000000000000711, 155.0000000000000000, -14.50000000000000711 ) ) ;
#27155 = FACE_BOUND ( 'NONE', #23822, .T. ) ;
#27156 = CARTESIAN_POINT ( 'NONE',  ( -8.000000000000008882, 206.9523078486584780, 77.49886208192144466 ) ) ;
#27157 = CARTESIAN_POINT ( 'NONE',  ( 92.60208470531341618, 155.0000000000000000, 13.00000000000002487 ) ) ;
#27158 = DIRECTION ( 'NONE',  ( -0.000000000000000000, -0.000000000000000000, 1.000000000000000000 ) ) ;
#27159 = CARTESIAN_POINT ( 'NONE',  ( 58.92499999726881299, 145.8408176439707802, -12.60653300113719588 ) ) ;
#27161 = EDGE_LOOP ( 'NONE', ( #25036, #5226 ) ) ;
#27160 = CARTESIAN_POINT ( 'NONE',  ( -6.139770520408368348, 215.5359834540460042, 21.95113791807856529 ) ) ;
#27162 = CARTESIAN_POINT ( 'NONE',  ( 43.11132485994280472, 140.7341522555726669, 4.635254915624211769 ) ) ;
#27163 = CARTESIAN_POINT ( 'NONE',  ( 82.57499999726880446, 145.8408176439707802, 12.60653300113718345 ) ) ;
#27164 = CARTESIAN_POINT ( 'NONE',  ( 7.456977232089302632, 217.1783343296989131, 91.55113791807858092 ) ) ;
#27165 = AXIS2_PLACEMENT_3D ( 'NONE', #3275, #16059, #5996 ) ;
#27166 = CARTESIAN_POINT ( 'NONE',  ( 3.044812012440130555, 197.4746971517856764, 92.60113791807857808 ) ) ;
#27167 = DIRECTION ( 'NONE',  ( 0.000000000000000000, -1.000000000000000000, 1.478898702612462246E-15 ) ) ;
#27168 = EDGE_LOOP ( 'NONE', ( #4902, #1268 ) ) ;
#27169 = CARTESIAN_POINT ( 'NONE',  ( 3.044812012439969795, 216.5253028482143520, 6.398862081921435241 ) ) ;
#27170 = CARTESIAN_POINT ( 'NONE',  ( 7.456977232089471386, 196.8216656703012006, 61.44886208192143329 ) ) ;
#27171 = CARTESIAN_POINT ( 'NONE',  ( -0.05014649552828402690, 217.5146222423826714, 78.24886208192144466 ) ) ;
#27172 = CARTESIAN_POINT ( 'NONE',  ( -11.98450388067341876, 203.0532714938636047, 5.348862081921434530 ) ) ;
#27173 = FACE_OUTER_BOUND ( 'NONE', #26297, .T. ) ;
#27174 = CARTESIAN_POINT ( 'NONE',  ( 8.062137200540920645, 201.0835637161417822, 23.30113791807856671 ) ) ;
#27175 = CARTESIAN_POINT ( 'NONE',  ( -8.118202686958138514, 212.8392687619910930, 86.79886208192142760 ) ) ;
#27176 = VERTEX_POINT ( 'NONE', #10661 ) ;
#27177 = CARTESIAN_POINT ( 'NONE',  ( 1.058054217398695762, -6.894685612232789751, -0.3576316571898509600 ) ) ;
#27178 = ORIENTED_EDGE ( 'NONE', *, *, #29115, .T. ) ;
#27179 = CARTESIAN_POINT ( 'NONE',  ( 0.000000000000000000, 0.000000000000000000, 0.000000000000000000 ) ) ;
#27180 = CARTESIAN_POINT ( 'NONE',  ( 6.500168698208244500, 202.3363017425938324, 70.29886208192142760 ) ) ;
#27181 = VERTEX_POINT ( 'NONE', #12869 ) ;
#27182 = ADVANCED_FACE ( 'NONE', ( #31277 ), #26476, .F. ) ;
#27183 = CARTESIAN_POINT ( 'NONE',  ( 84.12499999726881583, 155.0000000000000000, 15.58253174999999402 ) ) ;
#27184 = ORIENTED_EDGE ( 'NONE', *, *, #25408, .T. ) ;
#27185 = DIRECTION ( 'NONE',  ( 1.000000000000000000, 0.000000000000000000, 0.000000000000000000 ) ) ;
#27186 = CIRCLE ( 'NONE', #2174, 2.000000000000000000 ) ;
#27187 = CARTESIAN_POINT ( 'NONE',  ( 74.32499999726881867, 145.8408176439707802, 12.60653300113718345 ) ) ;
#27188 = CARTESIAN_POINT ( 'NONE',  ( 6.444103211791042618, 202.2591342207267644, 71.30113791807856671 ) ) ;
#27189 = FACE_OUTER_BOUND ( 'NONE', #31048, .T. ) ;
#27190 = CARTESIAN_POINT ( 'NONE',  ( 34.39999999999999858, 150.2886644046228639, -14.50000000000000888 ) ) ;
#27191 = CARTESIAN_POINT ( 'NONE',  ( -4.984841277089891776, 213.7757310962905990, 47.94886208192144039 ) ) ;
#27192 = CARTESIAN_POINT ( 'NONE',  ( 10.01549611932653860, 210.2015048109876716, 91.85113791807853545 ) ) ;
#27193 = CARTESIAN_POINT ( 'NONE',  ( 8.062137200540920645, 201.0835637161417822, 80.30113791807858092 ) ) ;
#27194 = LINE ( 'NONE', #3188, #5559 ) ;
#27195 = CARTESIAN_POINT ( 'NONE',  ( 125.6872233929728395, -5.249999999999975131, 35.00001200000001234 ) ) ;
#27196 = DIRECTION ( 'NONE',  ( 1.000000000000000000, 0.000000000000000000, 0.000000000000000000 ) ) ;
#27197 = CARTESIAN_POINT ( 'NONE',  ( 51.62499999726881583, 171.3844434931184253, -7.942151717890134290E-15 ) ) ;
#27198 = CARTESIAN_POINT ( 'NONE',  ( -9.736236675707914401, 199.9851607334237542, 51.20113791807856529 ) ) ;
#27199 = CARTESIAN_POINT ( 'NONE',  ( 41.21132485994281325, 139.2280666364260071, -4.041636747397287284E-15 ) ) ;
#27200 = CARTESIAN_POINT ( 'NONE',  ( -3.135527875058821579, 197.5041725223112223, 101.9011379180785752 ) ) ;
#27201 = CARTESIAN_POINT ( 'NONE',  ( 0.05014649552810506589, 217.5146222423826714, 70.25113791807856956 ) ) ;
#27202 = CARTESIAN_POINT ( 'NONE',  ( 9.736236675708031640, 199.9851607334238963, 31.29886208192143826 ) ) ;
#27203 = CARTESIAN_POINT ( 'NONE',  ( 9.984503880673420539, 210.2968891136705736, 45.84886208192142476 ) ) ;
#27204 = CARTESIAN_POINT ( 'NONE',  ( 85.89999999453762314, 150.2886644046228639, -14.50000000000000888 ) ) ;
#27205 = CARTESIAN_POINT ( 'NONE',  ( -11.98450388067348804, 210.9467285061362247, 78.65113791807858945 ) ) ;
#27206 = CARTESIAN_POINT ( 'NONE',  ( 4.903702542908601636, 200.1653181626581102, 101.4511379180785866 ) ) ;
#27207 = EDGE_CURVE ( 'NONE', #11089, #33178, #18317, .T. ) ;
#27208 =( BOUNDED_CURVE ( )  B_SPLINE_CURVE ( 2, ( #6559, #16943, #27338, #27507, #3498, #29730, #21888, #4003, #30067, #6732, #29564 ),
 .UNSPECIFIED., .F., .T. ) 
 B_SPLINE_CURVE_WITH_KNOTS ( ( 3, 2, 2, 2, 2, 3 ),
 ( 0.08928571428571423219, 0.09285714285714280480, 0.09642857142857139130, 0.09999999999999996392, 0.1035714285714285365, 0.1071428571428571092 ),
 .UNSPECIFIED. ) 
 CURVE ( )  GEOMETRIC_REPRESENTATION_ITEM ( )  RATIONAL_B_SPLINE_CURVE ( ( 1.000000000000000666, 0.9510565162951526430, 1.000000000000000000, 0.9510565162951534202, 1.000000000000000000, 0.9510565162951534202, 1.000000000000000000, 0.9510565162951534202, 1.000000000000000000, 0.9510565162951537532, 0.9999999999999996669 ) ) 
 REPRESENTATION_ITEM ( '' )  );
#27209 = CARTESIAN_POINT ( 'NONE',  ( 10.01549611932659545, 203.7984951890123853, 64.14886208192145034 ) ) ;
#27210 = CARTESIAN_POINT ( 'NONE',  ( 125.5000000000000000, 261.0000000000000000, 2.149999999999985256 ) ) ;
#27211 = ORIENTED_EDGE ( 'NONE', *, *, #212, .T. ) ;
#27212 = CARTESIAN_POINT ( 'NONE',  ( 9.680171189290716072, 214.0920067884432854, 63.69886208192144039 ) ) ;
#27213 = VERTEX_POINT ( 'NONE', #31595 ) ;
#27214 = CARTESIAN_POINT ( 'NONE',  ( 74.47499999726881015, 149.9369285172503510, 15.58253174999999580 ) ) ;
#27215 = CARTESIAN_POINT ( 'NONE',  ( -2.517493886309087880, 214.5937144450984135, 42.09886208192144608 ) ) ;
#27216 = ORIENTED_EDGE ( 'NONE', *, *, #12098, .T. ) ;
#27217 = ADVANCED_FACE ( 'NONE', ( #31436 ), #28710, .T. ) ;
#27218 = CARTESIAN_POINT ( 'NONE',  ( 80.87499999726881583, 138.6155565068815747, -3.929120461958505118E-15 ) ) ;
#27219 = FACE_BOUND ( 'NONE', #27089, .T. ) ;
#27220 = CARTESIAN_POINT ( 'NONE',  ( -2.832728918602883006, -6.234773369952733901, -6.171481112545254000 ) ) ;
#27221 = CARTESIAN_POINT ( 'NONE',  ( -2.426778023690262742, 214.6231898156240163, 55.10113791807857808 ) ) ;
#27222 = SURFACE_STYLE_USAGE ( .BOTH. , #30460 ) ;
#27223 = CARTESIAN_POINT ( 'NONE',  ( -3.044812012439970683, 197.4746971517856196, 34.89886208192143613 ) ) ;
#27224 = CARTESIAN_POINT ( 'NONE',  ( 70.27499999726880731, 160.0630714827496206, 15.58253174999999224 ) ) ;
#27225 = EDGE_LOOP ( 'NONE', ( #31426, #24153 ) ) ;
#27226 = CARTESIAN_POINT ( 'NONE',  ( -60.00000000000000000, -7.347880794884118356E-15, -20.00000000000001776 ) ) ;
#27227 = EDGE_CURVE ( 'NONE', #28697, #7596, #11529, .T. ) ;
#27228 = DIRECTION ( 'NONE',  ( 1.000000000000000000, 0.000000000000000000, 0.000000000000000000 ) ) ;
#27229 = CARTESIAN_POINT ( 'NONE',  ( 43.18867513459481700, 169.2658477444273331, -4.635254915624224203 ) ) ;
#27230 = CARTESIAN_POINT ( 'NONE',  ( -6.444103211790928043, 202.2591342207265939, 11.19886208192143506 ) ) ;
#27231 = CARTESIAN_POINT ( 'NONE',  ( -8.062137200540920645, 212.9164362838581894, 60.80113791807857382 ) ) ;
#27232 = CARTESIAN_POINT ( 'NONE',  ( 8.062137200540920645, 201.0835637161417822, 38.30113791807857382 ) ) ;
#27233 = CARTESIAN_POINT ( 'NONE',  ( -31.74999999999995737, 0.000000000000000000, 0.000000000000000000 ) ) ;
#27234 = CARTESIAN_POINT ( 'NONE',  ( -7.984503880673488041, 209.6470497212046098, 0.6511379180785660248 ) ) ;
#27235 = CARTESIAN_POINT ( 'NONE',  ( 47.82499999726881867, 168.2552932293087906, 9.630534252274372875 ) ) ;
#27236 = PLANE ( 'NONE',  #32870 ) ;
#27237 = CARTESIAN_POINT ( 'NONE',  ( 87.50000000000002842, 154.6566093261667163, -15.35392587765464079 ) ) ;
#27238 = CARTESIAN_POINT ( 'NONE',  ( -9.680171189290831535, 214.0920067884431148, 15.80113791807856849 ) ) ;
#27239 = DIRECTION ( 'NONE',  ( 0.000000000000000000, 1.000000000000000000, -1.478898702612462246E-15 ) ) ;
#27240 = EDGE_CURVE ( 'NONE', #1694, #2760, #26317, .T. ) ;
#27241 = CARTESIAN_POINT ( 'NONE',  ( 6.139770520408368348, 198.4640165459539674, 62.45113791807857950 ) ) ;
#27242 = CARTESIAN_POINT ( 'NONE',  ( 6.220909254589536808, 215.4770327129947987, 43.55113791807857382 ) ) ;
#27243 = LINE ( 'NONE', #9190, #2353 ) ;
#27244 = CARTESIAN_POINT ( 'NONE',  ( 32.50000000000000000, 155.0000000000000000, -13.00000000000002487 ) ) ;
#27245 = CARTESIAN_POINT ( 'NONE',  ( -9.736236675708031640, 214.0148392665760753, 2.798862081921433820 ) ) ;
#27246 = CARTESIAN_POINT ( 'NONE',  ( -3.135527875058982783, 216.4958274776886924, 9.098862081921435419 ) ) ;
#27247 = CARTESIAN_POINT ( 'NONE',  ( 64.19999999453762030, 163.5228861582408797, -11.73074641843674470 ) ) ;
#27248 = ORIENTED_EDGE ( 'NONE', *, *, #27992, .F. ) ;
#27249 = CARTESIAN_POINT ( 'NONE',  ( -12.00000000000000711, 207.0476921513413515, 45.50113791807856956 ) ) ;
#27250 = CARTESIAN_POINT ( 'NONE',  ( 8.000000000000008882, 206.9523078486586485, 65.00113791807856956 ) ) ;
#27251 = EDGE_CURVE ( 'NONE', #7491, #4173, #15084, .T. ) ;
#27252 = CARTESIAN_POINT ( 'NONE',  ( 9.984503880673420539, 210.2968891136705167, 33.84886208192143187 ) ) ;
#27253 = CARTESIAN_POINT ( 'NONE',  ( 76.71132485994280614, 155.0000000000000000, 15.00000000000001243 ) ) ;
#27254 = ORIENTED_EDGE ( 'NONE', *, *, #12033, .T. ) ;
#27255 = CARTESIAN_POINT ( 'NONE',  ( -8.118202686958039038, 201.1607312380087080, 87.20113791807858661 ) ) ;
#27256 = ORIENTED_EDGE ( 'NONE', *, *, #25804, .F. ) ;
#27257 = CARTESIAN_POINT ( 'NONE',  ( 42.28867513459482552, 139.2280666364260071, -4.041636747397287284E-15 ) ) ;
#27258 = DIRECTION ( 'NONE',  ( -0.000000000000000000, -0.000000000000000000, 1.000000000000000000 ) ) ;
#27259 = ORIENTED_EDGE ( 'NONE', *, *, #18036, .F. ) ;
#27260 =( BOUNDED_CURVE ( )  B_SPLINE_CURVE ( 2, ( #3510, #11352, #21736, #20326, #27814, #9942, #11982, #12319, #30551, #30386, #33446 ),
 .UNSPECIFIED., .F., .T. ) 
 B_SPLINE_CURVE_WITH_KNOTS ( ( 3, 2, 2, 2, 2, 3 ),
 ( 0.4285714285714285476, 0.4321428571428571619, 0.4357142857142857206, 0.4392857142857142239, 0.4428571428571427826, 0.4464285714285713969 ),
 .UNSPECIFIED. ) 
 CURVE ( )  GEOMETRIC_REPRESENTATION_ITEM ( )  RATIONAL_B_SPLINE_CURVE ( ( 1.000000000000000000, 0.9510565162951534202, 1.000000000000000000, 0.9510565162951534202, 1.000000000000000000, 0.9510565162951534202, 1.000000000000000000, 0.9510565162951534202, 1.000000000000000000, 0.9510565162951541973, 0.9999999999999992228 ) ) 
 REPRESENTATION_ITEM ( '' )  );
#27261 = CARTESIAN_POINT ( 'NONE',  ( -0.05014649552807731031, 198.5883022060938572, 23.75113791807855890 ) ) ;
#27262 = CARTESIAN_POINT ( 'NONE',  ( -58.66522414286995968, 194.9217985566782545, 2.500000000000000444 ) ) ;
#27263 = CARTESIAN_POINT ( 'NONE',  ( -11.98450388067341876, 203.0532714938636047, 104.3488620819214532 ) ) ;
#27264 = CARTESIAN_POINT ( 'NONE',  ( 52.77499999726881441, 140.1801316387863778, 4.815267126137185549 ) ) ;
#27265 = VERTEX_POINT ( 'NONE', #18651 ) ;
#27266 = CARTESIAN_POINT ( 'NONE',  ( -6.444103211791042618, 211.7408657792732356, 51.80113791807858092 ) ) ;
#27267 = CARTESIAN_POINT ( 'NONE',  ( 67.01132485994281751, 142.2402378747194405, 9.270509831248432420 ) ) ;
#27268 = AXIS2_PLACEMENT_3D ( 'NONE', #28070, #16999, #9504 ) ;
#27269 = SURFACE_SIDE_STYLE ('',( #9378 ) ) ;
#27270 = DIRECTION ( 'NONE',  ( 0.000000000000000000, 0.000000000000000000, -1.000000000000000000 ) ) ;
#27271 = CARTESIAN_POINT ( 'NONE',  ( -3.044812012439970683, 197.4746971517856196, 94.89886208192143613 ) ) ;
#27272 = CARTESIAN_POINT ( 'NONE',  ( 61.67499999726881299, 168.2552932293087906, -9.630534252274385310 ) ) ;
#27273 = CARTESIAN_POINT ( 'NONE',  ( -6.220909254589537696, 198.5229672870051161, 33.05113791807857382 ) ) ;
#27274 = CARTESIAN_POINT ( 'NONE',  ( 7.500000000000000000, 2.886751345948125547, -7.198902722707427593 ) ) ;
#27275 = EDGE_CURVE ( 'NONE', #5869, #4349, #24351, .T. ) ;
#27276 = ADVANCED_FACE ( 'NONE', ( #18812 ), #12364, .T. ) ;
#27277 = CARTESIAN_POINT ( 'NONE',  ( -12.01549611932659722, 210.8513442034533227, 74.64886208192143613 ) ) ;
#27278 = CARTESIAN_POINT ( 'NONE',  ( 82.99999999999998579, 170.2462022514548323, -7.872454543227099337E-15 ) ) ;
#27279 = FACE_OUTER_BOUND ( 'NONE', #3084, .T. ) ;
#27280 = DIRECTION ( 'NONE',  ( 1.000000000000000000, 0.000000000000000000, 0.000000000000000000 ) ) ;
#27281 = CARTESIAN_POINT ( 'NONE',  ( -8.118202686958039038, 201.1607312380087080, 99.20113791807858661 ) ) ;
#27282 = CARTESIAN_POINT ( 'NONE',  ( 0.000000000000000000, 0.000000000000000000, 0.000000000000000000 ) ) ;
#27283 = CARTESIAN_POINT ( 'NONE',  ( 42.17499999726881299, 164.1591823560292198, 12.60653300113718167 ) ) ;
#27284 = PRODUCT_DEFINITION ( 'UNKNOWN', '', #13194, #903 ) ;
#27285 = EDGE_CURVE ( 'NONE', #26168, #23832, #2000, .T. ) ;
#27286 = CARTESIAN_POINT ( 'NONE',  ( -9.984503880673473830, 210.2968891136704315, 36.65113791807855392 ) ) ;
#27287 = CARTESIAN_POINT ( 'NONE',  ( 85.22499999726882436, 160.0630714827496206, -15.58253175000000823 ) ) ;
#27288 = ORIENTED_EDGE ( 'NONE', *, *, #23098, .T. ) ;
#27289 = CARTESIAN_POINT ( 'NONE',  ( 125.5000000000000000, 155.0000000000000000, -6.938893903907228378E-15 ) ) ;
#27290 = CARTESIAN_POINT ( 'NONE',  ( 44.89999999453763024, 159.7113355953771077, 14.49999999999999289 ) ) ;
#27291 = CARTESIAN_POINT ( 'NONE',  ( -0.05014649552807705357, 194.3824533091408000, 23.75113791807855890 ) ) ;
#27292 = ADVANCED_FACE ( 'NONE', ( #7937 ), #2819, .F. ) ;
#27293 = CARTESIAN_POINT ( 'NONE',  ( -67.50000000000000000, 155.0000000000000000, 6.938893903907228378E-15 ) ) ;
#27294 = CARTESIAN_POINT ( 'NONE',  ( -9.521242624480144912, 207.9188892840786878, 102.6634595774070533 ) ) ;
#27295 = EDGE_LOOP ( 'NONE', ( #24502, #17934 ) ) ;
#27296 = CIRCLE ( 'NONE', #2284, 12.10452846326767684 ) ;
#27297 = CARTESIAN_POINT ( 'NONE',  ( 0.05014649552828288198, 194.3824533091408000, 40.74886208192143044 ) ) ;
#27298 = CARTESIAN_POINT ( 'NONE',  ( -3.135527875058821579, 197.5041725223112223, 5.901137918078566358 ) ) ;
#27299 = CARTESIAN_POINT ( 'NONE',  ( 3.044812012440130555, 197.4746971517856764, 53.60113791807857098 ) ) ;
#27300 = CARTESIAN_POINT ( 'NONE',  ( 4.984841277089891776, 200.2242689037093726, 16.44886208192143684 ) ) ;
#27301 = CARTESIAN_POINT ( 'NONE',  ( 79.38867513459483405, 169.2658477444273331, 4.635254915624208216 ) ) ;
#27302 = ORIENTED_EDGE ( 'NONE', *, *, #6565, .T. ) ;
#27303 = CARTESIAN_POINT ( 'NONE',  ( -8.000000000000008882, 206.9523078486584780, 104.4988620819214304 ) ) ;
#27304 = CYLINDRICAL_SURFACE ( 'NONE', #32797, 50.00000000000000000 ) ;
#27305 = CARTESIAN_POINT ( 'NONE',  ( -6.500168698208129925, 202.3363017425936050, 36.20113791807857240 ) ) ;
#27306 = CARTESIAN_POINT ( 'NONE',  ( 33.77499999726880731, 169.8198683612136222, -4.815267126137197984 ) ) ;
#27307 = ORIENTED_EDGE ( 'NONE', *, *, #2478, .T. ) ;
#27308 = CARTESIAN_POINT ( 'NONE',  ( 35.02499999726880020, 149.9369285172503510, -15.58253175000000823 ) ) ;
#27309 = DIRECTION ( 'NONE',  ( 0.000000000000000000, -0.04769215134144196705, 0.9988620819214357738 ) ) ;
#27310 = CARTESIAN_POINT ( 'NONE',  ( -10.01549611932659722, 210.2015048109875011, 65.64886208192143613 ) ) ;
#27311 = CARTESIAN_POINT ( 'NONE',  ( 38.17499999726881299, 164.1591823560292198, 12.60653300113718167 ) ) ;
#27312 = DIRECTION ( 'NONE',  ( -1.000000000000000000, -0.000000000000000000, -0.000000000000000000 ) ) ;
#27313 = CARTESIAN_POINT ( 'NONE',  ( -3.135527875058821579, 197.5041725223112223, 5.901137918078566358 ) ) ;
#27314 = AXIS2_PLACEMENT_3D ( 'NONE', #25737, #15514, #31356 ) ;
#27315 = CARTESIAN_POINT ( 'NONE',  ( 61.70000000000000284, 146.4771138417591203, 11.73074641843673227 ) ) ;
#27316 = DIRECTION ( 'NONE',  ( 0.000000000000000000, 0.7071067811865475727, 0.7071067811865475727 ) ) ;
#27317 = CARTESIAN_POINT ( 'NONE',  ( 4.903702542908435547, 213.8346818373419751, 81.54886208192144181 ) ) ;
#27318 = CARTESIAN_POINT ( 'NONE',  ( -150.0000000000000000, 0.000000000000000000, -20.00000000000000000 ) ) ;
#27319 = CARTESIAN_POINT ( 'NONE',  ( 77.30950000000004252, 0.000000000000000000, 0.000000000000000000 ) ) ;
#27320 = CARTESIAN_POINT ( 'NONE',  ( 56.42499999726881299, 141.7447067706911810, 9.630534252274376428 ) ) ;
#27322 = ORIENTED_EDGE ( 'NONE', *, *, #723, .T. ) ;
#27321 = CARTESIAN_POINT ( 'NONE',  ( -3.044812012440131443, 216.5253028482142952, 22.10113791807856742 ) ) ;
#27323 = CARTESIAN_POINT ( 'NONE',  ( 45.71132485994280614, 155.0000000000000000, -15.00000000000002487 ) ) ;
#27324 = AXIS2_PLACEMENT_3D ( 'NONE', #24210, #21152, #29487 ) ;
#27325 = CARTESIAN_POINT ( 'NONE',  ( 83.97499999726882436, 169.8198683612136222, 4.815267126137181997 ) ) ;
#27326 = CARTESIAN_POINT ( 'NONE',  ( 3.662846001190051659, 195.5725841191953691, 83.60113791807857808 ) ) ;
#27327 = AXIS2_PLACEMENT_3D ( 'NONE', #402, #10135, #10639 ) ;
#27328 = CARTESIAN_POINT ( 'NONE',  ( 72.18867513459481700, 140.7341522555726669, 4.635254915624211769 ) ) ;
#27329 = CARTESIAN_POINT ( 'NONE',  ( 53.28867513459483263, 170.7719333635740497, -7.904646289410545231E-15 ) ) ;
#27330 = EDGE_LOOP ( 'NONE', ( #24868, #20448, #29891, #12889 ) ) ;
#27331 = CARTESIAN_POINT ( 'NONE',  ( -0.05014649552828442242, 219.6175466908591716, 69.24886208192143044 ) ) ;
#27332 = CARTESIAN_POINT ( 'NONE',  ( -10.00000000000000711, 206.9523078486584495, 77.49886208192144466 ) ) ;
#27333 = CARTESIAN_POINT ( 'NONE',  ( -11.98450388067341876, 203.0532714938636047, 17.34886208192143187 ) ) ;
#27334 = LINE ( 'NONE', #32613, #27881 ) ;
#27335 = CARTESIAN_POINT ( 'NONE',  ( -6.220909254589537696, 198.5229672870051161, 24.05113791807855961 ) ) ;
#27336 = CARTESIAN_POINT ( 'NONE',  ( 3.044812012439969795, 216.5253028482143520, 93.39886208192143613 ) ) ;
#27337 = ORIENTED_EDGE ( 'NONE', *, *, #10969, .F. ) ;
#27338 = CARTESIAN_POINT ( 'NONE',  ( 38.91132485994280898, 146.1832212156128890, 12.13525491562421976 ) ) ;
#27339 = ORIENTED_EDGE ( 'NONE', *, *, #18291, .T. ) ;
#27340 = LINE ( 'NONE', #27509, #23829 ) ;
#27341 = CARTESIAN_POINT ( 'NONE',  ( 7.984503880673422316, 209.6470497212048372, 75.84886208192143897 ) ) ;
#27342 = VERTEX_POINT ( 'NONE', #24252 ) ;
#27343 = CARTESIAN_POINT ( 'NONE',  ( 84.82499999726880446, 141.7447067706911810, -9.630534252274387086 ) ) ;
#27344 = VERTEX_POINT ( 'NONE', #8756 ) ;
#27345 = DIRECTION ( 'NONE',  ( 1.000000000000000000, 0.000000000000000000, 0.000000000000000000 ) ) ;
#27346 = CIRCLE ( 'NONE', #22456, 50.00000000000000000 ) ;
#27347 = CIRCLE ( 'NONE', #1788, 112.0000000000000426 ) ;
#27348 = CARTESIAN_POINT ( 'NONE',  ( 78.82499999726881867, 141.7447067706911810, -9.630534252274385310 ) ) ;
#27349 = CARTESIAN_POINT ( 'NONE',  ( -58.50000000000001421, -88.00000000000000000, -20.00000000000000000 ) ) ;
#27350 = CARTESIAN_POINT ( 'NONE',  ( -6.500168698208129925, 202.3363017425936050, 66.20113791807857240 ) ) ;
#27351 = CARTESIAN_POINT ( 'NONE',  ( 87.49999999999998579, 168.4103784519322176, 7.072258346144660202 ) ) ;
#27352 = PRESENTATION_STYLE_ASSIGNMENT (( #24465 ) ) ;
#27353 = CARTESIAN_POINT ( 'NONE',  ( 43.60000000000000142, 150.2886644046228639, 14.49999999999999645 ) ) ;
#27354 = CARTESIAN_POINT ( 'NONE',  ( 2.517493886309087436, 199.4062855549015865, 52.59886208192143897 ) ) ;
#27355 = CARTESIAN_POINT ( 'NONE',  ( 8.118202686958039038, 212.8392687619912635, 76.70113791807857240 ) ) ;
#27356 = AXIS2_PLACEMENT_3D ( 'NONE', #6974, #3897, #9349 ) ;
#27357 = CARTESIAN_POINT ( 'NONE',  ( 32.50000000000000000, 155.0000000000000000, -6.938893903907228378E-15 ) ) ;
#27358 = CARTESIAN_POINT ( 'NONE',  ( 78.58867513459483689, 146.1832212156128890, -12.13525491562423042 ) ) ;
#27359 = CARTESIAN_POINT ( 'NONE',  ( 32.50000000000000000, 155.0000000000000000, -15.00000000000002487 ) ) ;
#27360 = CARTESIAN_POINT ( 'NONE',  ( 49.22499999726881725, 160.0630714827496206, -15.58253175000000823 ) ) ;
#27361 = CARTESIAN_POINT ( 'NONE',  ( -9.680171189290831535, 214.0920067884431148, 57.80113791807857382 ) ) ;
#27362 = FACE_OUTER_BOUND ( 'NONE', #449, .T. ) ;
#27363 = CARTESIAN_POINT ( 'NONE',  ( 9.984503880673470277, 203.7031108863295401, 101.1511379180785752 ) ) ;
#27364 = EDGE_CURVE ( 'NONE', #6985, #27176, #31920, .T. ) ;
#27365 = CARTESIAN_POINT ( 'NONE',  ( -6.220909254589537696, 198.5229672870051445, 78.05113791807858092 ) ) ;
#27366 = CARTESIAN_POINT ( 'NONE',  ( 9.736236675708031640, 199.9851607334238963, 43.29886208192143471 ) ) ;
#27367 = CARTESIAN_POINT ( 'NONE',  ( 8.118202686958138514, 201.1607312380088501, 52.29886208192143471 ) ) ;
#27368 = CARTESIAN_POINT ( 'NONE',  ( 85.59999999453762598, 141.2096805137202580, -4.480746418436742040 ) ) ;
#27369 = CARTESIAN_POINT ( 'NONE',  ( 11.98450388067348271, 203.0532714938637753, 89.15113791807856103 ) ) ;
#27370 = CARTESIAN_POINT ( 'NONE',  ( 8.000000000000008882, 206.9523078486586485, 101.0011379180785696 ) ) ;
#27371 = CARTESIAN_POINT ( 'NONE',  ( 3.135527875058981895, 197.5041725223112792, 61.59886208192143897 ) ) ;
#27372 = AXIS2_PLACEMENT_3D ( 'NONE', #25006, #4386, #14610 ) ;
#27373 =( NAMED_UNIT ( * ) SI_UNIT ( $, .STERADIAN. ) SOLID_ANGLE_UNIT ( ) );
#27374 = ORIENTED_EDGE ( 'NONE', *, *, #25562, .F. ) ;
#27375 = CARTESIAN_POINT ( 'NONE',  ( 7.375838497908012492, 217.2372850707501186, 60.54886208192144181 ) ) ;
#27376 = EDGE_LOOP ( 'NONE', ( #16528, #14946 ) ) ;
#27377 = CARTESIAN_POINT ( 'NONE',  ( 70.87499999726878741, 138.6155565068815463, -3.929120461958505118E-15 ) ) ;
#27378 = CARTESIAN_POINT ( 'NONE',  ( 0.05014649552828262524, 198.5883022060938572, 37.74886208192143755 ) ) ;
#27379 = ORIENTED_EDGE ( 'NONE', *, *, #33469, .F. ) ;
#27380 = CARTESIAN_POINT ( 'NONE',  ( 81.87499999726881583, 171.3844434931184253, -7.942151717890134290E-15 ) ) ;
#27381 = FACE_BOUND ( 'NONE', #7545, .T. ) ;
#27382 = CONICAL_SURFACE ( 'NONE', #8880, 32.00000000000002842, 1.466076571675244411 ) ;
#27383 = CARTESIAN_POINT ( 'NONE',  ( 125.5000000000000000, 152.8499999999996533, -106.0000000000000000 ) ) ;
#27384 = CARTESIAN_POINT ( 'NONE',  ( -2.517493886308901807, 199.4062855549015012, 59.90113791807856813 ) ) ;
#27385 =( GEOMETRIC_REPRESENTATION_CONTEXT ( 3 ) GLOBAL_UNCERTAINTY_ASSIGNED_CONTEXT ( ( #5552 ) ) GLOBAL_UNIT_ASSIGNED_CONTEXT ( ( #29579, #21901, #11692 ) ) REPRESENTATION_CONTEXT ( 'NONE', 'WORKASPACE' ) );
#27386 = LINE ( 'NONE', #19559, #23789 ) ;
#27387 = CARTESIAN_POINT ( 'NONE',  ( 0.05014649552828275708, 196.4853777576173002, 46.74886208192143755 ) ) ;
#27388 = ORIENTED_EDGE ( 'NONE', *, *, #16433, .F. ) ;
#27389 = DIRECTION ( 'NONE',  ( 0.000000000000000000, 0.000000000000000000, -1.000000000000000000 ) ) ;
#27390 = CARTESIAN_POINT ( 'NONE',  ( 52.68867513459483831, 150.1262045565068206, -15.00000000000030909 ) ) ;
#27391 = ADVANCED_FACE ( 'NONE', ( #24771 ), #21071, .T. ) ;
#27392 = CARTESIAN_POINT ( 'NONE',  ( 115.4999999999999858, 155.0000000000000000, -6.938893903907228378E-15 ) ) ;
#27393 = CARTESIAN_POINT ( 'NONE',  ( 6.500168698208244500, 202.3363017425938324, 19.29886208192143471 ) ) ;
#27394 = AXIS2_PLACEMENT_3D ( 'NONE', #30534, #27632, #27800 ) ;
#27395 = CARTESIAN_POINT ( 'NONE',  ( -3.044812012440131443, 216.5253028482142952, 64.10113791807857808 ) ) ;
#27396 = CARTESIAN_POINT ( 'NONE',  ( 10.01549611932653860, 210.2015048109876716, 43.85113791807854966 ) ) ;
#27397 = CARTESIAN_POINT ( 'NONE',  ( 87.87499999726877320, 171.3844434931184253, -7.942151717890132712E-15 ) ) ;
#27398 = CIRCLE ( 'NONE', #7821, 98.00000000000000000 ) ;
#27399 = ITEM_DEFINED_TRANSFORMATION ( 'NONE', 'NONE', #19168,  #2404 ) ;
#27400 = CARTESIAN_POINT ( 'NONE',  ( 6.220909254589536808, 215.4770327129947702, 22.55113791807856671 ) ) ;
#27401 = CARTESIAN_POINT ( 'NONE',  ( 4.903702542908435547, 213.8346818373419751, 99.54886208192144181 ) ) ;
#27402 = CARTESIAN_POINT ( 'NONE',  ( 43.22499999726881015, 160.0630714827496206, -15.58253175000000823 ) ) ;
#27403 = DIRECTION ( 'NONE',  ( -0.000000000000000000, -0.000000000000000000, 1.000000000000000000 ) ) ;
#27404 = CARTESIAN_POINT ( 'NONE',  ( 34.32499999726881157, 145.8408176439707802, 12.60653300113718345 ) ) ;
#27405 = CARTESIAN_POINT ( 'NONE',  ( 0.05014649552807549926, 219.6175466908591716, 25.25113791807856956 ) ) ;
#27406 = FACE_OUTER_BOUND ( 'NONE', #33248, .T. ) ;
#27407 =( BOUNDED_CURVE ( )  B_SPLINE_CURVE ( 2, ( #15359, #10271, #7703, #30704, #18086, #15691, #28483, #5138, #15192, #15525, #2590 ),
 .UNSPECIFIED., .F., .T. ) 
 B_SPLINE_CURVE_WITH_KNOTS ( ( 3, 2, 2, 2, 2, 3 ),
 ( 0.2321428571428572063, 0.2357142857142857373, 0.2392857142857142960, 0.2428571428571428548, 0.2464285714285714135, 0.2499999999999999445 ),
 .UNSPECIFIED. ) 
 CURVE ( )  GEOMETRIC_REPRESENTATION_ITEM ( )  RATIONAL_B_SPLINE_CURVE ( ( 0.9999999999999992228, 0.9510565162951541973, 1.000000000000000000, 0.9510565162951534202, 1.000000000000000000, 0.9510565162951534202, 1.000000000000000000, 0.9510565162951534202, 1.000000000000000000, 0.9510565162951541973, 0.9999999999999992228 ) ) 
 REPRESENTATION_ITEM ( '' )  );
#27408 = CARTESIAN_POINT ( 'NONE',  ( -3.135527875058821579, 197.5041725223112223, 77.90113791807857524 ) ) ;
#27409 = EDGE_CURVE ( 'NONE', #3255, #26876, #23793, .T. ) ;
#27410 = CARTESIAN_POINT ( 'NONE',  ( 10.00000000000000711, 206.9523078486586201, 35.00113791807856956 ) ) ;
#27411 = CARTESIAN_POINT ( 'NONE',  ( 76.38867513459481984, 140.7341522555726669, -4.635254915624220651 ) ) ;
#27412 = DIRECTION ( 'NONE',  ( 0.000000000000000000, 0.000000000000000000, -1.000000000000000000 ) ) ;
#27413 = CARTESIAN_POINT ( 'NONE',  ( -11.98450388067341876, 203.0532714938636047, 2.348862081921434530 ) ) ;
#27414 = CARTESIAN_POINT ( 'NONE',  ( 8.118202686958138514, 201.1607312380088501, 16.29886208192143471 ) ) ;
#27415 = CARTESIAN_POINT ( 'NONE',  ( 65.19999999453762030, 146.4771138417591203, 11.73074641843673227 ) ) ;
#27416 = ORIENTED_EDGE ( 'NONE', *, *, #8272, .T. ) ;
#27417 = CARTESIAN_POINT ( 'NONE',  ( 0.05014649552807549926, 219.6175466908591716, 52.25113791807857666 ) ) ;
#27418 = CARTESIAN_POINT ( 'NONE',  ( -2.517493886308901807, 199.4062855549015012, 71.90113791807856103 ) ) ;
#27419 = CARTESIAN_POINT ( 'NONE',  ( -6.139770520408224463, 198.4640165459539389, 35.04886208192144181 ) ) ;
#27420 = FILL_AREA_STYLE_COLOUR ( '', #27014 ) ;
#27421 = EDGE_LOOP ( 'NONE', ( #1363, #32205, #7875, #20217, #14843 ) ) ;
#27422 = EDGE_CURVE ( 'NONE', #16362, #17208, #19439, .T. ) ;
#27423 = STYLED_ITEM ( 'NONE', ( #26402 ), #12730 ) ;
#27424 = CARTESIAN_POINT ( 'NONE',  ( 6.139770520408368348, 198.4640165459539674, 89.45113791807857240 ) ) ;
#27425 = CONICAL_SURFACE ( 'NONE', #10035, 3.309499999999999886, 0.7853981633974710386 ) ;
#27426 = ORIENTED_EDGE ( 'NONE', *, *, #115, .T. ) ;
#27427 = CARTESIAN_POINT ( 'NONE',  ( 87.49999999999997158, 161.8888959785116413, -14.01425902168828408 ) ) ;
#27428 = DIRECTION ( 'NONE',  ( 1.000000000000000000, 0.000000000000000000, 0.000000000000000000 ) ) ;
#27429 = VERTEX_POINT ( 'NONE', #1096 ) ;
#27430 = CARTESIAN_POINT ( 'NONE',  ( -7.984503880673488041, 209.6470497212046098, 36.65113791807856103 ) ) ;
#27431 = EDGE_CURVE ( 'NONE', #8808, #3666, #25464, .T. ) ;
#27432 = CARTESIAN_POINT ( 'NONE',  ( 54.91132485994280898, 146.1832212156128890, 12.13525491562421976 ) ) ;
#27433 = CARTESIAN_POINT ( 'NONE',  ( -6.220909254589682469, 215.4770327129946850, 17.94886208192143684 ) ) ;
#27434 = CARTESIAN_POINT ( 'NONE',  ( 50.17499999726881299, 164.1591823560292198, 12.60653300113718167 ) ) ;
#27435 = EDGE_LOOP ( 'NONE', ( #1286, #17166 ) ) ;
#27436 = CARTESIAN_POINT ( 'NONE',  ( -6.500168698208129925, 202.3363017425936050, 48.20113791807858661 ) ) ;
#27437 = CARTESIAN_POINT ( 'NONE',  ( 67.71132485994280614, 155.0000000000000000, -15.00000000000002487 ) ) ;
#27438 = PRESENTATION_LAYER_ASSIGNMENT (  '', '', ( #8929 ) ) ;
#27439 =( NAMED_UNIT ( * ) PLANE_ANGLE_UNIT ( ) SI_UNIT ( $, .RADIAN. ) );
#27440 = DIRECTION ( 'NONE',  ( 0.000000000000000000, 0.000000000000000000, -1.000000000000000000 ) ) ;
#27441 = CARTESIAN_POINT ( 'NONE',  ( 3.044812012439969795, 216.5253028482143520, 87.39886208192143613 ) ) ;
#27442 = EDGE_CURVE ( 'NONE', #17155, #24999, #29378, .T. ) ;
#27443 = CARTESIAN_POINT ( 'NONE',  ( 60.27499999726880020, 160.0630714827496206, 15.58253174999999402 ) ) ;
#27444 = CARTESIAN_POINT ( 'NONE',  ( 6.220909254589536808, 215.4770327129947702, 28.55113791807855961 ) ) ;
#27445 = FACE_OUTER_BOUND ( 'NONE', #363, .T. ) ;
#27446 = CARTESIAN_POINT ( 'NONE',  ( 3.044812012440130555, 197.4746971517856764, 17.60113791807856742 ) ) ;
#27447 = DIRECTION ( 'NONE',  ( 1.000000000000000000, 0.000000000000000000, 6.123233995736766036E-17 ) ) ;
#27448 = CARTESIAN_POINT ( 'NONE',  ( 80.19999999999997442, 142.6655632788954620, -8.961492836873480528 ) ) ;
#27449 = DIRECTION ( 'NONE',  ( 0.000000000000000000, 0.000000000000000000, 1.000000000000000000 ) ) ;
#27450 = CARTESIAN_POINT ( 'NONE',  ( -6.139770520408369237, 215.5359834540460042, 90.95113791807854398 ) ) ;
#27451 = CARTESIAN_POINT ( 'NONE',  ( 32.50000000000000000, 155.0000000000000000, -6.938893903907228378E-15 ) ) ;
#27452 = CARTESIAN_POINT ( 'NONE',  ( 46.87499999726880873, 138.6155565068815463, -3.929120461958505118E-15 ) ) ;
#27453 = CARTESIAN_POINT ( 'NONE',  ( -9.984503880673473830, 210.2968891136704315, 45.65113791807855392 ) ) ;
#27454 = CARTESIAN_POINT ( 'NONE',  ( 81.52499999726880731, 169.8198683612136222, -4.815267126137197984 ) ) ;
#27455 = DIRECTION ( 'NONE',  ( 0.000000000000000000, 0.000000000000000000, -1.000000000000000000 ) ) ;
#27456 = CARTESIAN_POINT ( 'NONE',  ( 64.71132485994279193, 155.0000000000000000, 15.00000000000001243 ) ) ;
#27457 = CARTESIAN_POINT ( 'NONE',  ( 48.39999999453763024, 168.7903194862797420, -4.480746418436745593 ) ) ;
#27458 = EDGE_LOOP ( 'NONE', ( #1439, #17937, #13067, #31865 ) ) ;
#27459 = CARTESIAN_POINT ( 'NONE',  ( 3.753561863808689836, 218.3979405102790565, 16.40113791807856458 ) ) ;
#27460 = CARTESIAN_POINT ( 'NONE',  ( 61.11132485994280472, 140.7341522555726669, 4.635254915624211769 ) ) ;
#27461 = FACE_OUTER_BOUND ( 'NONE', #3581, .T. ) ;
#27462 = ORIENTED_EDGE ( 'NONE', *, *, #23076, .T. ) ;
#27463 = CARTESIAN_POINT ( 'NONE',  ( 9.736236675708031640, 199.9851607334238963, 40.29886208192143471 ) ) ;
#27464 = CARTESIAN_POINT ( 'NONE',  ( 0.05014649552810505201, 217.5146222423826714, 1.251137918078566003 ) ) ;
#27465 = CARTESIAN_POINT ( 'NONE',  ( -9.984503880673473830, 210.2968891136704315, 57.65113791807858235 ) ) ;
#27466 = CARTESIAN_POINT ( 'NONE',  ( -6.444103211790928043, 202.2591342207265939, 26.19886208192144039 ) ) ;
#27467 = EDGE_CURVE ( 'NONE', #29176, #860, #26509, .T. ) ;
#27468 = LINE ( 'NONE', #17754, #21391 ) ;
#27469 = ORIENTED_EDGE ( 'NONE', *, *, #11204, .F. ) ;
#27470 = CARTESIAN_POINT ( 'NONE',  ( 8.000000000000008882, 207.0476921513415220, 99.99886208192143044 ) ) ;
#27471 = EDGE_CURVE ( 'NONE', #21367, #9657, #5857, .T. ) ;
#27472 = FACE_OUTER_BOUND ( 'NONE', #24866, .T. ) ;
#27473 = CARTESIAN_POINT ( 'NONE',  ( -6.444103211791042618, 211.7408657792732356, 36.80113791807856671 ) ) ;
#27474 = DIRECTION ( 'NONE',  ( 0.000000000000000000, 0.000000000000000000, -1.000000000000000000 ) ) ;
#27475 = ORIENTED_EDGE ( 'NONE', *, *, #8139, .F. ) ;
#27476 = CARTESIAN_POINT ( 'NONE',  ( 38.82499999726881157, 141.7447067706911810, -9.630534252274385310 ) ) ;
#27477 = DIRECTION ( 'NONE',  ( 0.000000000000000000, 0.000000000000000000, -1.000000000000000000 ) ) ;
#27478 = FACE_OUTER_BOUND ( 'NONE', #27965, .T. ) ;
#27479 = CARTESIAN_POINT ( 'NONE',  ( -9.984503880673420539, 203.7031108863293980, 59.34886208192141765 ) ) ;
#27480 = EDGE_CURVE ( 'NONE', #5476, #28404, #29241, .T. ) ;
#27481 = CARTESIAN_POINT ( 'NONE',  ( 39.27499999726880020, 149.9369285172503510, -15.58253175000000823 ) ) ;
#27482 = FACE_BOUND ( 'NONE', #25425, .T. ) ;
#27483 = CARTESIAN_POINT ( 'NONE',  ( -6.139770520408369237, 215.5359834540460042, 6.951137918078566180 ) ) ;
#27484 = CARTESIAN_POINT ( 'NONE',  ( 95.70416941062676131, 155.0000000000000000, -32.00000000000005684 ) ) ;
#27485 =( REPRESENTATION_RELATIONSHIP ('NONE','NONE', #25663, #12832 ) REPRESENTATION_RELATIONSHIP_WITH_TRANSFORMATION ( #29123 )SHAPE_REPRESENTATION_RELATIONSHIP( ) );
#27486 = CARTESIAN_POINT ( 'NONE',  ( 61.59999999999999432, 150.2886644046228639, 14.49999999999999645 ) ) ;
#27487 = CARTESIAN_POINT ( 'NONE',  ( -6.999999999999969802, -1.734723475976807094E-14, -2.899999999999999911 ) ) ;
#27488 = CARTESIAN_POINT ( 'NONE',  ( 0.05014649552828262524, 198.5883022060938572, 85.74886208192143044 ) ) ;
#27489 = CARTESIAN_POINT ( 'NONE',  ( -2.325424218463065351, 7.317669739334662360, -7.030005583190789054 ) ) ;
#27490 = CARTESIAN_POINT ( 'NONE',  ( 117.5000000000000000, 155.0000000000000000, -98.00000000000000000 ) ) ;
#27491 = CARTESIAN_POINT ( 'NONE',  ( 62.62499999726881583, 138.6155565068815463, -3.929120461958505118E-15 ) ) ;
#27493 = VERTEX_POINT ( 'NONE', #27318 ) ;
#27492 = CARTESIAN_POINT ( 'NONE',  ( 3.135527875058820690, 216.4958274776887492, 19.40113791807856813 ) ) ;
#27494 = CARTESIAN_POINT ( 'NONE',  ( -7.940546747334013666, 27.16978800334332433, -0.4491195576436714521 ) ) ;
#27495 = CARTESIAN_POINT ( 'NONE',  ( 81.17499999726882720, 145.8408176439707802, -12.60653300113719588 ) ) ;
#27496 = CARTESIAN_POINT ( 'NONE',  ( -12.00000000000000711, 207.0476921513413515, 90.50113791807858377 ) ) ;
#27497 = CARTESIAN_POINT ( 'NONE',  ( 5.000000000000000000, -2.342598717236903383, 4.057500000000001883 ) ) ;
#27498 = VERTEX_POINT ( 'NONE', #32094 ) ;
#27499 = CARTESIAN_POINT ( 'NONE',  ( 9.680171189290716072, 214.0920067884432854, 72.69886208192143329 ) ) ;
#27500 = CARTESIAN_POINT ( 'NONE',  ( -3.044812012439970683, 197.4746971517856196, 73.89886208192143613 ) ) ;
#27501 = CARTESIAN_POINT ( 'NONE',  ( 3.753561863808876797, 195.6020594897209719, 13.59886208192143719 ) ) ;
#27502 = CARTESIAN_POINT ( 'NONE',  ( -27.50000000000000355, -10.64700562007355344, -16.86587997430611807 ) ) ;
#27503 = CARTESIAN_POINT ( 'NONE',  ( -6.220909254589537696, 198.5229672870051161, 30.05113791807856671 ) ) ;
#27504 = DIRECTION ( 'NONE',  ( 0.8660254037844383745, -0.5000000000000004441, 0.000000000000000000 ) ) ;
#27505 = CARTESIAN_POINT ( 'NONE',  ( 8.062137200540822946, 212.9164362838583315, 84.69886208192144750 ) ) ;
#27506 = EDGE_CURVE ( 'NONE', #16034, #26664, #24432, .T. ) ;
#27507 = CARTESIAN_POINT ( 'NONE',  ( 39.01132485994280330, 142.2402378747194405, 9.270509831248432420 ) ) ;
#27508 = ORIENTED_EDGE ( 'NONE', *, *, #25629, .F. ) ;
#27509 = CARTESIAN_POINT ( 'NONE',  ( 4.000000000000000000, 3.518949890710768802, -4.770489558936219510E-15 ) ) ;
#27510 = CARTESIAN_POINT ( 'NONE',  ( -4.984841277089891776, 213.7757310962905990, 68.94886208192144750 ) ) ;
#27511 = EDGE_CURVE ( 'NONE', #3377, #25076, #26809, .T. ) ;
#27512 = ORIENTED_EDGE ( 'NONE', *, *, #22865, .T. ) ;
#27513 = EDGE_CURVE ( 'NONE', #11140, #17374, #25990, .T. ) ;
#27514 = CARTESIAN_POINT ( 'NONE',  ( 81.72499999726881015, 169.8198683612136222, 4.815267126137181997 ) ) ;
#27515 = ORIENTED_EDGE ( 'NONE', *, *, #22411, .F. ) ;
#27516 = CARTESIAN_POINT ( 'NONE',  ( 69.31132485994278625, 140.7341522555726669, -4.635254915624220651 ) ) ;
#27517 = CARTESIAN_POINT ( 'NONE',  ( 73.22499999726881015, 160.0630714827496206, -15.58253175000000823 ) ) ;
#27518 = CARTESIAN_POINT ( 'NONE',  ( 0.000000000000000000, 0.000000000000000000, 2.066666666666666430 ) ) ;
#27519 = CARTESIAN_POINT ( 'NONE',  ( 8.000000000000008882, 206.9523078486586485, 80.00113791807856956 ) ) ;
#27520 = CARTESIAN_POINT ( 'NONE',  ( 87.50000000000002842, 170.3903390413697707, -0.7067623181846339753 ) ) ;
#27521 = CARTESIAN_POINT ( 'NONE',  ( 44.79999999999999005, 167.3344367211045096, -8.961492836873482304 ) ) ;
#27522 = CARTESIAN_POINT ( 'NONE',  ( 4.984841277089891776, 200.2242689037093726, 55.44886208192143329 ) ) ;
#27523 = PLANE ( 'NONE',  #17550 ) ;
#27524 = CARTESIAN_POINT ( 'NONE',  ( -18.00000000000000711, 0.000000000000000000, -17.97459999999999525 ) ) ;
#27525 = CARTESIAN_POINT ( 'NONE',  ( 27.50000000000000000, 1.342284157770883724, -18.00000000000000000 ) ) ;
#27526 = CARTESIAN_POINT ( 'NONE',  ( 51.92499999726880588, 164.1591823560292198, 12.60653300113718167 ) ) ;
#27527 = CARTESIAN_POINT ( 'NONE',  ( 66.27499999726880731, 160.0630714827496206, 15.58253174999999402 ) ) ;
#27528 = CARTESIAN_POINT ( 'NONE',  ( 0.05014649552807549926, 219.6175466908591716, 61.25113791807856245 ) ) ;
#27529 = CARTESIAN_POINT ( 'NONE',  ( 4.102348501002488490, 207.3577873115561943, -8.835681806194324750 ) ) ;
#27530 = CARTESIAN_POINT ( 'NONE',  ( 12.01549611932652972, 210.8513442034534933, 1.851137918078565647 ) ) ;
#27531 = CARTESIAN_POINT ( 'NONE',  ( 6.139770520408367460, 198.4640165459539389, 80.45113791807857240 ) ) ;
#27532 = CARTESIAN_POINT ( 'NONE',  ( 7.375838497908012492, 217.2372850707501186, 39.54886208192143471 ) ) ;
#27533 = CARTESIAN_POINT ( 'NONE',  ( -3.044812012439970683, 197.4746971517856196, 46.89886208192143613 ) ) ;
#27534 = CARTESIAN_POINT ( 'NONE',  ( 85.99999999453764588, 155.0000000000000000, -14.50000000000000711 ) ) ;
#27535 = CARTESIAN_POINT ( 'NONE',  ( -7.456977232089304408, 196.8216656703010301, 84.05113791807858092 ) ) ;
#27536 = CARTESIAN_POINT ( 'NONE',  ( 0.05014649552807626948, 215.4116977939061144, 94.25113791807859798 ) ) ;
#27537 = CARTESIAN_POINT ( 'NONE',  ( 8.062137200540822946, 212.9164362838583315, 60.69886208192143329 ) ) ;
#27538 =( NAMED_UNIT ( * ) PLANE_ANGLE_UNIT ( ) SI_UNIT ( $, .RADIAN. ) );
#27539 = ORIENTED_EDGE ( 'NONE', *, *, #17989, .F. ) ;
#27540 = CARTESIAN_POINT ( 'NONE',  ( -12.00000000000000711, 206.9523078486584780, 71.49886208192144466 ) ) ;
#27541 = EDGE_LOOP ( 'NONE', ( #21205, #21833, #5144, #33135 ) ) ;
#27542 = CARTESIAN_POINT ( 'NONE',  ( 69.97499999726881015, 169.8198683612136222, 4.815267126137181997 ) ) ;
#27543 = CARTESIAN_POINT ( 'NONE',  ( 6.500168698208244500, 202.3363017425938324, 46.29886208192144892 ) ) ;
#27544 = ORIENTED_EDGE ( 'NONE', *, *, #17100, .T. ) ;
#27545 = VECTOR ( 'NONE', #28646, 1000.000000000000000 ) ;
#27546 = CARTESIAN_POINT ( 'NONE',  ( 85.67499999726881299, 168.2552932293087906, -9.630534252274387086 ) ) ;
#27547 = CYLINDRICAL_SURFACE ( 'NONE', #20585, 15.00000000000001776 ) ;
#27548 = CARTESIAN_POINT ( 'NONE',  ( 60.00000000000000000, 7.347880794884118356E-15, 35.00000000000000000 ) ) ;
#27549 = CARTESIAN_POINT ( 'NONE',  ( -8.015496119326531499, 204.4483345814780364, 63.35113791807857098 ) ) ;
#27550 =( LENGTH_UNIT ( ) NAMED_UNIT ( * ) SI_UNIT ( .MILLI., .METRE. ) );
#27551 = CARTESIAN_POINT ( 'NONE',  ( 8.118202686958138514, 201.1607312380088501, 40.29886208192143471 ) ) ;
#27552 = ORIENTED_EDGE ( 'NONE', *, *, #18695, .T. ) ;
#27553 = CIRCLE ( 'NONE', #15042, 5.200000000000009948 ) ;
#27554 = DIRECTION ( 'NONE',  ( -1.000000000000000000, 0.000000000000000000, 0.000000000000000000 ) ) ;
#27555 = DIRECTION ( 'NONE',  ( 0.7071067811865454633, -0.000000000000000000, 0.7071067811865495711 ) ) ;
#27556 = DIRECTION ( 'NONE',  ( 1.000000000000000000, 0.000000000000000000, 0.000000000000000000 ) ) ;
#27557 = CARTESIAN_POINT ( 'NONE',  ( -6.500168698208244500, 211.6636982574061676, 23.79886208192143826 ) ) ;
#27558 = CARTESIAN_POINT ( 'NONE',  ( -6.139770520408369237, 215.5359834540460042, 60.95113791807857950 ) ) ;
#27559 = CARTESIAN_POINT ( 'NONE',  ( 6.220909254589536808, 215.4770327129947702, 49.55113791807855250 ) ) ;
#27560 = CONTEXT_DEPENDENT_SHAPE_REPRESENTATION ( #25549, #1120 ) ;
#27561 = CARTESIAN_POINT ( 'NONE',  ( 9.984503880673470277, 203.7031108863295401, 17.15113791807856103 ) ) ;
#27562 = CARTESIAN_POINT ( 'NONE',  ( 6.444103211791042618, 202.2591342207267644, 8.301137918078564937 ) ) ;
#27563 = CARTESIAN_POINT ( 'NONE',  ( 44.52499999726881441, 140.1801316387863778, 4.815267126137185549 ) ) ;
#27564 = CARTESIAN_POINT ( 'NONE',  ( 33.32499999726881157, 164.1591823560292198, -12.60653300113719766 ) ) ;
#27565 = CARTESIAN_POINT ( 'NONE',  ( -0.05014649552807705357, 194.3824533091408000, 26.75113791807856956 ) ) ;
#27566 = DIRECTION ( 'NONE',  ( 0.000000000000000000, 0.9988620819214357738, 0.04769215134144196705 ) ) ;
#27567 = CARTESIAN_POINT ( 'NONE',  ( 0.05014649552810505201, 217.5146222423826714, 73.25113791807855534 ) ) ;
#27568 = CARTESIAN_POINT ( 'NONE',  ( 8.118202686958039038, 212.8392687619912635, 49.70113791807857240 ) ) ;
#27569 = AXIS2_PLACEMENT_3D ( 'NONE', #7496, #15316, #23657 ) ;
#27570 = CARTESIAN_POINT ( 'NONE',  ( 76.28867513459483973, 139.2280666364260071, -4.041636747397287284E-15 ) ) ;
#27571 = CIRCLE ( 'NONE', #6913, 3.500000000000000444 ) ;
#27572 = CARTESIAN_POINT ( 'NONE',  ( 1.734723475976807094E-14, 31.75426480542944319, -15.54379906938135214 ) ) ;
#27573 = CARTESIAN_POINT ( 'NONE',  ( -12.00000000000000711, 206.9523078486584780, 17.49886208192143400 ) ) ;
#27574 = CARTESIAN_POINT ( 'NONE',  ( 10.00000000000000711, 207.0476921513415220, 18.99886208192143755 ) ) ;
#27575 = CARTESIAN_POINT ( 'NONE',  ( 68.49999999453761745, 170.2462022514548323, -7.872454543227099337E-15 ) ) ;
#27576 = VERTEX_POINT ( 'NONE', #11487 ) ;
#27577 = CARTESIAN_POINT ( 'NONE',  ( -9.680171189290831535, 214.0920067884431148, 60.80113791807858092 ) ) ;
#27578 = CARTESIAN_POINT ( 'NONE',  ( -6.500168698208129925, 202.3363017425936050, 66.20113791807857240 ) ) ;
#27579 = CARTESIAN_POINT ( 'NONE',  ( 10.00000000000000711, 207.0476921513415220, 27.99886208192143755 ) ) ;
#27580 = CARTESIAN_POINT ( 'NONE',  ( 76.01132485994281751, 167.7597621252805880, -9.270509831248443078 ) ) ;
#27581 = CIRCLE ( 'NONE', #10721, 19.99999999999998934 ) ;
#27582 = ORIENTED_EDGE ( 'NONE', *, *, #2287, .F. ) ;
#27583 = CARTESIAN_POINT ( 'NONE',  ( -6.139770520408369237, 215.5359834540460042, 90.95113791807854398 ) ) ;
#27584 = ORIENTED_EDGE ( 'NONE', *, *, #27635, .T. ) ;
#27585 = CARTESIAN_POINT ( 'NONE',  ( 98.19869130599479945, 155.0000000000000000, 0.000000000000000000 ) ) ;
#27586 = CARTESIAN_POINT ( 'NONE',  ( 2.262848203703083261, 6.566616684922145453, -6.208169345099790348 ) ) ;
#27587 = ORIENTED_EDGE ( 'NONE', *, *, #9111, .T. ) ;
#27588 = CARTESIAN_POINT ( 'NONE',  ( 6.444103211791042618, 202.2591342207267644, 32.30113791807856671 ) ) ;
#27589 = CIRCLE ( 'NONE', #6363, 3.500000000000000444 ) ;
#27590 = CARTESIAN_POINT ( 'NONE',  ( 85.11132485994279762, 140.7341522555726669, 4.635254915624211769 ) ) ;
#27591 = EDGE_CURVE ( 'NONE', #30720, #19012, #5841, .T. ) ;
#27592 = CIRCLE ( 'NONE', #21088, 7.500000000000015099 ) ;
#27593 = CARTESIAN_POINT ( 'NONE',  ( -6.220909254589682469, 215.4770327129946850, 11.94886208192143684 ) ) ;
#27594 = CARTESIAN_POINT ( 'NONE',  ( 58.17499999726881299, 164.1591823560292198, 12.60653300113718167 ) ) ;
#27595 = ORIENTED_EDGE ( 'NONE', *, *, #7298, .F. ) ;
#27596 = CARTESIAN_POINT ( 'NONE',  ( -8.015496119326531499, 204.4483345814780364, 54.35113791807857098 ) ) ;
#27597 = CIRCLE ( 'NONE', #13447, 0.4000000000000001887 ) ;
#27598 = CIRCLE ( 'NONE', #18823, 2.200000000000001066 ) ;
#27599 = DIRECTION ( 'NONE',  ( 0.000000000000000000, 0.000000000000000000, 1.000000000000000000 ) ) ;
#27600 = CARTESIAN_POINT ( 'NONE',  ( 6.220909254589681581, 198.5229672870052582, 97.44886208192143329 ) ) ;
#27601 = CARTESIAN_POINT ( 'NONE',  ( 64.17499999726879878, 164.1591823560292198, 12.60653300113718167 ) ) ;
#27602 = CARTESIAN_POINT ( 'NONE',  ( -8.118202686958039038, 201.1607312380087080, 30.20113791807856884 ) ) ;
#27603 = FILL_AREA_STYLE ('',( #17215 ) ) ;
#27604 = CARTESIAN_POINT ( 'NONE',  ( 10.00000000000000711, 206.9523078486586201, 14.00113791807856600 ) ) ;
#27605 = VECTOR ( 'NONE', #19316, 1000.000000000000000 ) ;
#27606 = DIRECTION ( 'NONE',  ( 1.000000000000000000, 0.000000000000000000, 0.000000000000000000 ) ) ;
#27607 = CARTESIAN_POINT ( 'NONE',  ( 78.89999999999999147, 168.7903194862797420, -4.480746418436745593 ) ) ;
#27608 = CARTESIAN_POINT ( 'NONE',  ( -56.12844631811822893, 194.9921284422999292, -0.8077925457893648797 ) ) ;
#27609 = DIRECTION ( 'NONE',  ( -0.000000000000000000, -0.000000000000000000, 1.000000000000000000 ) ) ;
#27610 = CARTESIAN_POINT ( 'NONE',  ( 11.98450388067348271, 203.0532714938637753, 2.151137918078565914 ) ) ;
#27611 = FACE_OUTER_BOUND ( 'NONE', #19132, .T. ) ;
#27612 = CARTESIAN_POINT ( 'NONE',  ( 41.67499999726881299, 168.2552932293087906, -9.630534252274385310 ) ) ;
#27613 = CARTESIAN_POINT ( 'NONE',  ( -3.044812012440131443, 216.5253028482142952, 46.10113791807857098 ) ) ;
#27614 = CARTESIAN_POINT ( 'NONE',  ( 80.82499999726880446, 141.7447067706911810, -9.630534252274385310 ) ) ;
#27615 = CARTESIAN_POINT ( 'NONE',  ( -6.127431526422343306E-17, 9.147862274876549904, -8.047472243342932430 ) ) ;
#27616 = FACE_OUTER_BOUND ( 'NONE', #17890, .T. ) ;
#27617 = CARTESIAN_POINT ( 'NONE',  ( 50.39999999453763024, 168.7903194862797420, -4.480746418436745593 ) ) ;
#27618 = ORIENTED_EDGE ( 'NONE', *, *, #2040, .F. ) ;
#27619 = CARTESIAN_POINT ( 'NONE',  ( -0.05014649552807705357, 194.3824533091408000, 26.75113791807856956 ) ) ;
#27620 = AXIS2_PLACEMENT_3D ( 'NONE', #12783, #8012, #31176 ) ;
#27621 = LINE ( 'NONE', #4291, #3446 ) ;
#27622 = AXIS2_PLACEMENT_3D ( 'NONE', #32874, #27760, #28102 ) ;
#27623 = DIRECTION ( 'NONE',  ( 1.000000000000000000, 0.000000000000000000, 0.000000000000000000 ) ) ;
#27624 = ORIENTED_EDGE ( 'NONE', *, *, #31268, .T. ) ;
#27625 = VECTOR ( 'NONE', #24804, 1000.000000000000000 ) ;
#27626 = CARTESIAN_POINT ( 'NONE',  ( -3.753561863808878130, 218.3979405102790281, 45.09886208192143897 ) ) ;
#27627 = CARTESIAN_POINT ( 'NONE',  ( -58.50000000000002132, 209.9999999999999716, -2.500000000000000000 ) ) ;
#27628 = CARTESIAN_POINT ( 'NONE',  ( -8.062137200540920645, 212.9164362838581894, 60.80113791807857382 ) ) ;
#27629 = EDGE_CURVE ( 'NONE', #20607, #22066, #14971, .T. ) ;
#27630 = CARTESIAN_POINT ( 'NONE',  ( -6.444103211790928043, 202.2591342207265939, 20.19886208192143684 ) ) ;
#27631 = AXIS2_PLACEMENT_3D ( 'NONE', #24896, #20289, #1719 ) ;
#27632 = DIRECTION ( 'NONE',  ( -0.000000000000000000, -0.000000000000000000, 1.000000000000000000 ) ) ;
#27633 = EDGE_LOOP ( 'NONE', ( #5962, #7752, #29525, #32602 ) ) ;
#27634 = CARTESIAN_POINT ( 'NONE',  ( 6.500168698208129925, 211.6636982574063381, 1.701137918078565958 ) ) ;
#27635 = EDGE_CURVE ( 'NONE', #22398, #20653, #33452, .T. ) ;
#27636 = CARTESIAN_POINT ( 'NONE',  ( -3.750000000000007105, -6.495190528383289141, 0.000000000000000000 ) ) ;
#27637 = CARTESIAN_POINT ( 'NONE',  ( 11.98450388067341876, 210.9467285061363953, 87.84886208192142476 ) ) ;
#27638 = CARTESIAN_POINT ( 'NONE',  ( 35.97499999726881015, 169.8198683612136222, 4.815267126137181997 ) ) ;
#27639 = VERTEX_POINT ( 'NONE', #24939 ) ;
#27640 = CARTESIAN_POINT ( 'NONE',  ( 46.12499999726880873, 155.0000000000000000, 15.58253174999999402 ) ) ;
#27641 = CARTESIAN_POINT ( 'NONE',  ( 9.576885917778305668, 206.5919175358980624, 112.0468591418754869 ) ) ;
#27642 = CARTESIAN_POINT ( 'NONE',  ( -2.654873707089686533E-16, -7.550815748621508838, -6.286450516130496879 ) ) ;
#27643 = VECTOR ( 'NONE', #3967, 1000.000000000000000 ) ;
#27644 = CARTESIAN_POINT ( 'NONE',  ( 6.220909254589681581, 198.5229672870052582, 73.44886208192139065 ) ) ;
#27645 = CARTESIAN_POINT ( 'NONE',  ( 42.27499999726880731, 160.0630714827496206, 15.58253174999999402 ) ) ;
#27646 = DIRECTION ( 'NONE',  ( 1.000000000000000000, 0.000000000000000000, 0.000000000000000000 ) ) ;
#27647 = CARTESIAN_POINT ( 'NONE',  ( -3.044812012440131443, 216.5253028482142952, 4.101137918078565647 ) ) ;
#27648 = CARTESIAN_POINT ( 'NONE',  ( -3.499999999999999112, 0.6879904500768249109, -0.03016324292412032870 ) ) ;
#27649 = CIRCLE ( 'NONE', #5878, 11.99999999999998224 ) ;
#27650 = EDGE_CURVE ( 'NONE', #16155, #14265, #27818, .T. ) ;
#27651 = CARTESIAN_POINT ( 'NONE',  ( 58.89999999999999858, 168.7903194862797420, -4.480746418436745593 ) ) ;
#27652 = DIRECTION ( 'NONE',  ( -1.000000000000000000, -0.000000000000000000, 0.000000000000000000 ) ) ;
#27653 = CARTESIAN_POINT ( 'NONE',  ( -8.000000000000008882, 206.9523078486584780, 86.49886208192144466 ) ) ;
#27654 = CARTESIAN_POINT ( 'NONE',  ( -0.5620262070071414540, 7.564407249984292037, -6.443844059477446429 ) ) ;
#27655 = DIRECTION ( 'NONE',  ( 1.000000000000000000, 0.000000000000000000, 0.000000000000000000 ) ) ;
#27656 = CARTESIAN_POINT ( 'NONE',  ( -11.98450388067341876, 203.0532714938636047, 86.34886208192143897 ) ) ;
#27657 = CIRCLE ( 'NONE', #10800, 40.00000000000000711 ) ;
#27658 = CARTESIAN_POINT ( 'NONE',  ( 66.72499999726881015, 140.1801316387863778, -4.815267126137194431 ) ) ;
#27660 = ORIENTED_EDGE ( 'NONE', *, *, #24492, .T. ) ;
#27659 = CARTESIAN_POINT ( 'NONE',  ( 3.044812012440130555, 197.4746971517856764, 17.60113791807856742 ) ) ;
#27661 = DIRECTION ( 'NONE',  ( 0.000000000000000000, 0.000000000000000000, 1.000000000000000000 ) ) ;
#27662 = CARTESIAN_POINT ( 'NONE',  ( 79.97499999726881015, 169.8198683612136222, 4.815267126137181997 ) ) ;
#27663 = CARTESIAN_POINT ( 'NONE',  ( 9.736236675707914401, 214.0148392665762458, 88.70113791807857240 ) ) ;
#27664 = ADVANCED_FACE ( 'NONE', ( #25440 ), #12933, .T. ) ;
#27665 = CARTESIAN_POINT ( 'NONE',  ( -10.00000000000000711, 207.0476921513413515, 102.5011379180785838 ) ) ;
#27666 = ORIENTED_EDGE ( 'NONE', *, *, #11894, .T. ) ;
#27667 = CARTESIAN_POINT ( 'NONE',  ( -3.662846001189865142, 195.5725841191952838, 67.89886208192143613 ) ) ;
#27668 = CARTESIAN_POINT ( 'NONE',  ( -8.118202686958138514, 212.8392687619910930, 77.79886208192144181 ) ) ;
#27669 = CARTESIAN_POINT ( 'NONE',  ( -0.05014649552828442242, 219.6175466908591716, 9.248862081921435774 ) ) ;
#27670 = CARTESIAN_POINT ( 'NONE',  ( 127.5000000000000000, 48.99999999999998579, -1.387778780781445676E-14 ) ) ;
#27671 = AXIS2_PLACEMENT_3D ( 'NONE', #22080, #12025, #4185 ) ;
#27672 = CARTESIAN_POINT ( 'NONE',  ( 8.118202686958039038, 212.8392687619912635, 28.70113791807856884 ) ) ;
#27673 = EDGE_CURVE ( 'NONE', #23405, #6991, #9597, .T. ) ;
#27674 = DIRECTION ( 'NONE',  ( 0.000000000000000000, 0.000000000000000000, 1.000000000000000000 ) ) ;
#27675 = CARTESIAN_POINT ( 'NONE',  ( -8.118202686958138514, 212.8392687619910930, 98.79886208192144181 ) ) ;
#27676 = CIRCLE ( 'NONE', #18972, 2.149999999999984812 ) ;
#27677 = SHAPE_REPRESENTATION_RELATIONSHIP ( 'NONE' , 'NONE' ,  #18505, #10045 ) ;
#27678 = DIRECTION ( 'NONE',  ( 0.000000000000000000, 0.000000000000000000, 1.000000000000000000 ) ) ;
#27679 = EDGE_LOOP ( 'NONE', ( #32657, #33219, #862, #13367 ) ) ;
#27680 = CARTESIAN_POINT ( 'NONE',  ( 70.21132485994283456, 170.7719333635740497, -7.904646289410545231E-15 ) ) ;
#27681 = CARTESIAN_POINT ( 'NONE',  ( -4.984841277089891776, 213.7757310962905990, 83.94886208192144750 ) ) ;
#27682 = EDGE_LOOP ( 'NONE', ( #28676, #17615, #15153 ) ) ;
#27683 = APPLICATION_CONTEXT ( 'automotive_design' ) ;
#27684 = AXIS2_PLACEMENT_3D ( 'NONE', #597, #9234, #18497 ) ;
#27685 = CARTESIAN_POINT ( 'NONE',  ( 84.22499999726881015, 149.9369285172503510, 15.58253174999999580 ) ) ;
#27686 = ORIENTED_EDGE ( 'NONE', *, *, #11152, .F. ) ;
#27687 = LINE ( 'NONE', #29914, #29750 ) ;
#27688 = CARTESIAN_POINT ( 'NONE',  ( 74.62499999726883004, 138.6155565068815463, -3.929120461958505118E-15 ) ) ;
#27689 = DIRECTION ( 'NONE',  ( 1.000000000000000000, 0.000000000000000000, 0.000000000000000000 ) ) ;
#27690 = CARTESIAN_POINT ( 'NONE',  ( 2.426778023690261410, 199.3768101843759837, 74.60113791807854966 ) ) ;
#27691 = DIRECTION ( 'NONE',  ( 1.000000000000000000, 0.000000000000000000, 0.000000000000000000 ) ) ;
#27692 = CARTESIAN_POINT ( 'NONE',  ( 40.40000000000000568, 150.2886644046228639, -14.50000000000000888 ) ) ;
#27693 = CARTESIAN_POINT ( 'NONE',  ( -2.426778023690076225, 199.3768101843759553, 55.89886208192144323 ) ) ;
#27694 = AXIS2_PLACEMENT_3D ( 'NONE', #33286, #26776, #18622 ) ;
#27695 = ADVANCED_FACE ( 'NONE', ( #22372 ), #17405, .F. ) ;
#27696 = EDGE_CURVE ( 'NONE', #25951, #1291, #30391, .T. ) ;
#27697 = DIRECTION ( 'NONE',  ( -0.000000000000000000, -0.000000000000000000, -1.000000000000000000 ) ) ;
#27698 = LINE ( 'NONE', #4360, #31177 ) ;
#27699 = CARTESIAN_POINT ( 'NONE',  ( -7.500000000000005329, 4.330127018922187432, -7.564335161054492218 ) ) ;
#27700 = PLANE ( 'NONE',  #10061 ) ;
#27701 = CARTESIAN_POINT ( 'NONE',  ( 50.62499999726880873, 138.6155565068815747, -3.929120461958505118E-15 ) ) ;
#27702 = CARTESIAN_POINT ( 'NONE',  ( 65.37499999726881583, 155.0000000000000000, -15.58253175000000823 ) ) ;
#27703 = CARTESIAN_POINT ( 'NONE',  ( -9.736236675707914401, 199.9851607334237542, 54.20113791807856529 ) ) ;
#27704 = CARTESIAN_POINT ( 'NONE',  ( 117.5000000000000142, 155.0000000000000000, -6.938893903907228378E-15 ) ) ;
#27705 = PRODUCT_DEFINITION ( 'UNKNOWN', '', #9395, #26342 ) ;
#27706 = CARTESIAN_POINT ( 'NONE',  ( 8.062137200540920645, 201.0835637161417822, 101.3011379180785809 ) ) ;
#27707 = EDGE_CURVE ( 'NONE', #25104, #27576, #11986, .T. ) ;
#27708 = CARTESIAN_POINT ( 'NONE',  ( -10.00000000000000711, 207.0476921513413515, 75.50113791807858377 ) ) ;
#27709 = CARTESIAN_POINT ( 'NONE',  ( -7.456977232089471386, 217.1783343296987709, 41.94886208192144039 ) ) ;
#27710 = CARTESIAN_POINT ( 'NONE',  ( 3.135527875058981895, 197.5041725223112792, 46.59886208192143187 ) ) ;
#27711 = CARTESIAN_POINT ( 'NONE',  ( 125.5000000000000000, 228.4330392262228600, -76.47359838532524634 ) ) ;
#27712 = CARTESIAN_POINT ( 'NONE',  ( 3.753561863808689836, 218.3979405102790565, 88.40113791807857524 ) ) ;
#27713 = CARTESIAN_POINT ( 'NONE',  ( 5.000000000000000000, 4.685197434473814759, -5.637851296924623057E-15 ) ) ;
#27714 = CARTESIAN_POINT ( 'NONE',  ( 10.00000000000000711, 206.9523078486586201, 2.001137918078565558 ) ) ;
#27715 = ADVANCED_FACE ( 'NONE', ( #22888 ), #25098, .T. ) ;
#27716 = CARTESIAN_POINT ( 'NONE',  ( -8.062137200540822946, 201.0835637161416400, 74.19886208192143329 ) ) ;
#27717 = CARTESIAN_POINT ( 'NONE',  ( 67.50000000000000000, 155.0000000000000000, -6.938893903907228378E-15 ) ) ;
#27718 = ORIENTED_EDGE ( 'NONE', *, *, #12294, .T. ) ;
#27719 = CARTESIAN_POINT ( 'NONE',  ( -11.98450388067341876, 203.0532714938636047, 74.34886208192142476 ) ) ;
#27720 = ORIENTED_EDGE ( 'NONE', *, *, #7946, .T. ) ;
#27721 = CARTESIAN_POINT ( 'NONE',  ( 70.97499999726881015, 140.1801316387863778, -4.815267126137194431 ) ) ;
#27722 = CARTESIAN_POINT ( 'NONE',  ( -6.444103211790928043, 202.2591342207265939, 47.19886208192144750 ) ) ;
#27723 = AXIS2_PLACEMENT_3D ( 'NONE', #28310, #33068, #12972 ) ;
#27724 = ORIENTED_EDGE ( 'NONE', *, *, #1661, .F. ) ;
#27725 = CARTESIAN_POINT ( 'NONE',  ( 80.27499999726879309, 160.0630714827496206, 15.58253174999999224 ) ) ;
#27726 = DIRECTION ( 'NONE',  ( 0.000000000000000000, 1.000000000000000000, -0.000000000000000000 ) ) ;
#27727 = FACE_OUTER_BOUND ( 'NONE', #4426, .T. ) ;
#27728 = CARTESIAN_POINT ( 'NONE',  ( 54.72499999726881015, 140.1801316387863778, -4.815267126137194431 ) ) ;
#27729 = CARTESIAN_POINT ( 'NONE',  ( -3.135527875058982783, 216.4958274776886924, 45.09886208192143897 ) ) ;
#27730 = ORIENTED_EDGE ( 'NONE', *, *, #7663, .F. ) ;
#27731 = CARTESIAN_POINT ( 'NONE',  ( 0.000000000000000000, 0.000000000000000000, 0.000000000000000000 ) ) ;
#27732 = CARTESIAN_POINT ( 'NONE',  ( 0.000000000000000000, 0.000000000000000000, 0.000000000000000000 ) ) ;
#27733 = CARTESIAN_POINT ( 'NONE',  ( 98.19869130599479945, 155.0000000000000000, -32.10452846326769816 ) ) ;
#27734 = CARTESIAN_POINT ( 'NONE',  ( 6.500168698208244500, 202.3363017425938324, 28.29886208192143826 ) ) ;
#27735 = CARTESIAN_POINT ( 'NONE',  ( -6.220909254589537696, 198.5229672870051161, 63.05113791807858092 ) ) ;
#27736 = CARTESIAN_POINT ( 'NONE',  ( 9.984503880673470277, 203.7031108863295401, 44.15113791807856813 ) ) ;
#27737 = CARTESIAN_POINT ( 'NONE',  ( -2.466666666666999408, 3.020795437897212205E-16, 2.066666666667000385 ) ) ;
#27738 = CARTESIAN_POINT ( 'NONE',  ( -6.139770520408369237, 215.5359834540460042, 18.95113791807856884 ) ) ;
#27739 = CARTESIAN_POINT ( 'NONE',  ( -7.984503880673488041, 209.6470497212046098, 3.651137918078566802 ) ) ;
#27740 = CARTESIAN_POINT ( 'NONE',  ( 45.82499999726881157, 168.2552932293087906, 9.630534252274372875 ) ) ;
#27741 = CARTESIAN_POINT ( 'NONE',  ( 1.750000000000016209, -3.031088913245524985, -2.899999999999999911 ) ) ;
#27742 = CARTESIAN_POINT ( 'NONE',  ( 34.92499999726881299, 145.8408176439707802, -12.60653300113719588 ) ) ;
#27743 = CARTESIAN_POINT ( 'NONE',  ( 7.375838497908181246, 196.7627149292499666, 32.45113791807856529 ) ) ;
#27744 = DIRECTION ( 'NONE',  ( 0.000000000000000000, 0.000000000000000000, 1.000000000000000000 ) ) ;
#27745 = CARTESIAN_POINT ( 'NONE',  ( 10.01549611932653860, 210.2015048109876716, 79.85113791807853545 ) ) ;
#27746 = CARTESIAN_POINT ( 'NONE',  ( -8.062137200540920645, 212.9164362838581894, 51.80113791807857382 ) ) ;
#27747 = CARTESIAN_POINT ( 'NONE',  ( 6.902527771671632451, 4.675077770780898589, -0.7026937717022819774 ) ) ;
#27748 = CARTESIAN_POINT ( 'NONE',  ( 54.68867513459483121, 150.1262045565066785, -15.00000000000021316 ) ) ;
#27749 = CARTESIAN_POINT ( 'NONE',  ( -3.662846001189865142, 195.5725841191952838, 10.89886208192143613 ) ) ;
#27750 = CARTESIAN_POINT ( 'NONE',  ( -3.135527875058982783, 216.4958274776886924, 15.09886208192143542 ) ) ;
#27751 = CARTESIAN_POINT ( 'NONE',  ( 70.59999999453762598, 168.7903194862797420, 4.480746418436729606 ) ) ;
#27752 = ORIENTED_EDGE ( 'NONE', *, *, #23038, .T. ) ;
#27753 = CARTESIAN_POINT ( 'NONE',  ( 9.680171189290831535, 199.9079932115568852, 62.30113791807858092 ) ) ;
#27754 = CARTESIAN_POINT ( 'NONE',  ( -8.000000000000008882, 207.0476921513413515, 75.50113791807856956 ) ) ;
#27755 = CARTESIAN_POINT ( 'NONE',  ( -10.01549611932659722, 210.2015048109875011, 26.64886208192142902 ) ) ;
#27756 = VECTOR ( 'NONE', #676, 1000.000000000000000 ) ;
#27757 = ORIENTED_EDGE ( 'NONE', *, *, #12425, .F. ) ;
#27758 = ORIENTED_EDGE ( 'NONE', *, *, #23044, .F. ) ;
#27759 = VERTEX_POINT ( 'NONE', #1937 ) ;
#27760 = DIRECTION ( 'NONE',  ( 0.000000000000000000, 1.000000000000000000, -1.224646799147353207E-16 ) ) ;
#27761 = CARTESIAN_POINT ( 'NONE',  ( 2.971071886220372438, 5.790204346174072647, 1.063026348804146728E-15 ) ) ;
#27762 = VERTEX_POINT ( 'NONE', #17265 ) ;
#27763 = CARTESIAN_POINT ( 'NONE',  ( -6.500168698208129925, 202.3363017425936050, 33.20113791807857240 ) ) ;
#27764 = DIRECTION ( 'NONE',  ( -1.000000000000000000, 0.000000000000000000, 0.000000000000000000 ) ) ;
#27765 = CARTESIAN_POINT ( 'NONE',  ( 3.044812012439969795, 216.5253028482143520, 18.39886208192143613 ) ) ;
#27766 = CARTESIAN_POINT ( 'NONE',  ( 54.87499999726880873, 138.6155565068815747, -3.929120461958505118E-15 ) ) ;
#27767 = ORIENTED_EDGE ( 'NONE', *, *, #3882, .T. ) ;
#27768 = CARTESIAN_POINT ( 'NONE',  ( -8.015496119326531499, 204.4483345814780364, 45.35113791807857098 ) ) ;
#27769 = DIRECTION ( 'NONE',  ( 1.000000000000000000, 0.000000000000000000, 0.000000000000000000 ) ) ;
#27770 = LINE ( 'NONE', #4615, #496 ) ;
#27771 = CARTESIAN_POINT ( 'NONE',  ( 3.044812012439969795, 216.5253028482143520, 96.39886208192145034 ) ) ;
#27772 = CARTESIAN_POINT ( 'NONE',  ( 65.67499999726881299, 168.2552932293087906, -9.630534252274385310 ) ) ;
#27773 = CARTESIAN_POINT ( 'NONE',  ( 3.135527875058820690, 216.4958274776887492, 31.40113791807857524 ) ) ;
#27774 = CARTESIAN_POINT ( 'NONE',  ( 69.88867513459481984, 150.1262045565062238, 14.99999999999987388 ) ) ;
#27775 = CARTESIAN_POINT ( 'NONE',  ( 8.062137200540920645, 201.0835637161417822, 14.30113791807856671 ) ) ;
#27776 = VECTOR ( 'NONE', #6280, 1000.000000000000000 ) ;
#27777 = DIRECTION ( 'NONE',  ( 1.000000000000000000, 0.000000000000000000, 0.000000000000000000 ) ) ;
#27778 = CIRCLE ( 'NONE', #21264, 32.00000000000002842 ) ;
#27779 = CARTESIAN_POINT ( 'NONE',  ( 78.50000000000000000, 155.0000000000000000, -14.50000000000000711 ) ) ;
#27780 = CARTESIAN_POINT ( 'NONE',  ( -55.99986651211894184, 195.0000083429897586, 0.1629166443388770646 ) ) ;
#27781 = CARTESIAN_POINT ( 'NONE',  ( 0.1999999999999987899, 0.000000000000000000, 3.299999999999999822 ) ) ;
#27782 = CARTESIAN_POINT ( 'NONE',  ( -12.00000000000000711, 207.0476921513413515, 0.5011379180785653364 ) ) ;
#27783 = CARTESIAN_POINT ( 'NONE',  ( 4.000000000000000000, -2.639212418033075380, 1.523750000000003268 ) ) ;
#27784 = CARTESIAN_POINT ( 'NONE',  ( 51.27499999726880731, 149.9369285172503510, -15.58253175000000823 ) ) ;
#27785 = CARTESIAN_POINT ( 'NONE',  ( 10.00000000000000711, 206.9523078486586201, 50.00113791807856956 ) ) ;
#27786 = CARTESIAN_POINT ( 'NONE',  ( 83.22499999726879594, 160.0630714827496206, -15.58253175000000823 ) ) ;
#27787 = CARTESIAN_POINT ( 'NONE',  ( -6.601567268551443490, 5.319966374295965750, -7.792327460285856766 ) ) ;
#27788 = DIRECTION ( 'NONE',  ( -1.000000000000000000, -0.000000000000000000, -0.000000000000000000 ) ) ;
#27789 = CARTESIAN_POINT ( 'NONE',  ( 45.39999999453763024, 141.2096805137202580, 4.480746418436733158 ) ) ;
#27790 = ORIENTED_EDGE ( 'NONE', *, *, #27650, .F. ) ;
#27791 = CARTESIAN_POINT ( 'NONE',  ( -12.00000000000000711, 207.0476921513413515, 27.50113791807856956 ) ) ;
#27792 = DIRECTION ( 'NONE',  ( 0.000000000000000000, -1.000000000000000000, 0.000000000000000000 ) ) ;
#27793 = EDGE_CURVE ( 'NONE', #17333, #26168, #30733, .T. ) ;
#27794 = CARTESIAN_POINT ( 'NONE',  ( 7.456977232089471386, 196.8216656703012006, 103.4488620819214475 ) ) ;
#27795 = CYLINDRICAL_SURFACE ( 'NONE', #29743, 15.00000000000001776 ) ;
#27796 = ORIENTED_EDGE ( 'NONE', *, *, #6328, .F. ) ;
#27797 = CARTESIAN_POINT ( 'NONE',  ( 3.044812012440130555, 197.4746971517856764, 5.601137918078566535 ) ) ;
#27798 = CARTESIAN_POINT ( 'NONE',  ( -0.05014649552810635652, 196.4853777576173002, 65.75113791807856956 ) ) ;
#27799 = CARTESIAN_POINT ( 'NONE',  ( 7.984503880673422316, 209.6470497212048372, 27.84886208192143897 ) ) ;
#27800 = DIRECTION ( 'NONE',  ( 1.000000000000000000, 0.000000000000000000, 0.000000000000000000 ) ) ;
#27801 = ORIENTED_EDGE ( 'NONE', *, *, #4311, .T. ) ;
#27802 = CARTESIAN_POINT ( 'NONE',  ( -6.444103211791042618, 211.7408657792732356, 0.8011379180785661580 ) ) ;
#27803 = DIRECTION ( 'NONE',  ( 1.000000000000000000, 0.000000000000000000, 0.000000000000000000 ) ) ;
#27804 = CARTESIAN_POINT ( 'NONE',  ( 11.98450388067341876, 210.9467285061363953, 90.84886208192142476 ) ) ;
#27805 = CARTESIAN_POINT ( 'NONE',  ( 36.07499999726880446, 168.2552932293087906, 9.630534252274372875 ) ) ;
#27806 = VERTEX_POINT ( 'NONE', #12326 ) ;
#27807 = CARTESIAN_POINT ( 'NONE',  ( 42.02499999726880731, 160.0630714827496206, 15.58253174999999402 ) ) ;
#27808 = DIRECTION ( 'NONE',  ( -6.106226635438360972E-16, 0.04769215134144213358, -0.9988620819214358848 ) ) ;
#27809 = DIRECTION ( 'NONE',  ( 0.000000000000000000, 0.4999999999999990008, -0.8660254037844391517 ) ) ;
#27810 = CARTESIAN_POINT ( 'NONE',  ( 3.135527875058981895, 197.5041725223112792, 67.59886208192143897 ) ) ;
#27811 = CARTESIAN_POINT ( 'NONE',  ( 49.97499999726881725, 169.8198683612136222, 4.815267126137181997 ) ) ;
#27812 = LINE ( 'NONE', #12149, #17928 ) ;
#27813 = CARTESIAN_POINT ( 'NONE',  ( 10.00000000000000711, 206.9523078486586201, 8.001137918078566003 ) ) ;
#27814 = CARTESIAN_POINT ( 'NONE',  ( 58.11132485994280472, 169.2658477444273331, -4.635254915624224203 ) ) ;
#27815 = CARTESIAN_POINT ( 'NONE',  ( 62.70000000000000284, 163.5228861582408797, -11.73074641843674470 ) ) ;
#27816 = CARTESIAN_POINT ( 'NONE',  ( 8.118202686958039038, 212.8392687619912635, 88.70113791807857240 ) ) ;
#27817 = CARTESIAN_POINT ( 'NONE',  ( 64.71132485994279193, 155.0000000000000000, 15.00000000000001243 ) ) ;
#27818 = LINE ( 'NONE', #28172, #3676 ) ;
#27819 = CARTESIAN_POINT ( 'NONE',  ( -3.399999999999999911, 4.163799117101000559E-16, -8.000000000000000000 ) ) ;
#27820 = CARTESIAN_POINT ( 'NONE',  ( -9.680171189290716072, 199.9079932115567146, 89.19886208192144750 ) ) ;
#27821 = CARTESIAN_POINT ( 'NONE',  ( 67.12499999726881583, 155.0000000000000000, -15.58253175000000823 ) ) ;
#27823 = EDGE_LOOP ( 'NONE', ( #21475, #27005, #7586, #25552, #4644, #12331 ) ) ;
#27822 = CARTESIAN_POINT ( 'NONE',  ( -8.062137200540920645, 212.9164362838581894, 18.80113791807856671 ) ) ;
#27824 = CARTESIAN_POINT ( 'NONE',  ( 42.91132485994280188, 146.1832212156128890, 12.13525491562421976 ) ) ;
#27825 = AXIS2_PLACEMENT_3D ( 'NONE', #19654, #32759, #30044 ) ;
#27826 = CARTESIAN_POINT ( 'NONE',  ( 84.97499999726882436, 140.1801316387863778, -4.815267126137194431 ) ) ;
#27827 = CARTESIAN_POINT ( 'NONE',  ( 0.05014649552807549926, 219.6175466908591716, 85.25113791807856956 ) ) ;
#27828 = LINE ( 'NONE', #22050, #26262 ) ;
#27829 = ADVANCED_FACE ( 'NONE', ( #14706 ), #7053, .F. ) ;
#27830 = EDGE_LOOP ( 'NONE', ( #24109, #23949, #27752, #10729 ) ) ;
#27831 = CARTESIAN_POINT ( 'NONE',  ( 12.01549611932659367, 203.1486557965466773, 67.14886208192143613 ) ) ;
#27832 = CARTESIAN_POINT ( 'NONE',  ( 3.044812012439969795, 216.5253028482143520, 75.39886208192143613 ) ) ;
#27833 = CARTESIAN_POINT ( 'NONE',  ( -3.753561863808878130, 218.3979405102790281, 15.09886208192143719 ) ) ;
#27834 = DIRECTION ( 'NONE',  ( -0.000000000000000000, 0.000000000000000000, 1.000000000000000000 ) ) ;
#27835 = CARTESIAN_POINT ( 'NONE',  ( -8.118202686958039038, 201.1607312380087080, 36.20113791807857240 ) ) ;
#27836 = DIRECTION ( 'NONE',  ( 0.000000000000000000, 0.000000000000000000, 1.000000000000000000 ) ) ;
#27837 = CARTESIAN_POINT ( 'NONE',  ( -3.135527875058982783, 216.4958274776886924, 102.0988620819214390 ) ) ;
#27838 = EDGE_CURVE ( 'NONE', #28486, #31748, #18906, .T. ) ;
#27839 = CARTESIAN_POINT ( 'NONE',  ( 2.055025722542103583, 6.319083845363847374, -5.720331885005371042 ) ) ;
#27840 = ORIENTED_EDGE ( 'NONE', *, *, #7501, .F. ) ;
#27841 = PLANE ( 'NONE',  #31971 ) ;
#27842 = CARTESIAN_POINT ( 'NONE',  ( 6.500168698208244500, 202.3363017425938324, 82.29886208192144181 ) ) ;
#27843 = ORIENTED_EDGE ( 'NONE', *, *, #27849, .F. ) ;
#27844 = CARTESIAN_POINT ( 'NONE',  ( 10.00000000000000888, 207.8771832641648984, -0.04188241574673567946 ) ) ;
#27845 = ORIENTED_EDGE ( 'NONE', *, *, #6402, .T. ) ;
#27846 = CARTESIAN_POINT ( 'NONE',  ( 0.000000000000000000, 0.000000000000000000, -8.499999999999998224 ) ) ;
#27847 = CARTESIAN_POINT ( 'NONE',  ( 72.67499999726881299, 141.7447067706911810, 9.630534252274376428 ) ) ;
#27848 = CARTESIAN_POINT ( 'NONE',  ( 85.92499999726881299, 164.1591823560292198, 12.60653300113718167 ) ) ;
#27849 = EDGE_CURVE ( 'NONE', #31511, #10102, #11727, .T. ) ;
#27850 = PLANE ( 'NONE',  #5628 ) ;
#27851 = CARTESIAN_POINT ( 'NONE',  ( -6.444103211791042618, 211.7408657792732356, 75.80113791807858092 ) ) ;
#27852 = CARTESIAN_POINT ( 'NONE',  ( 87.50000000000005684, 169.8231623009795328, -4.699990950160915837 ) ) ;
#27853 = AXIS2_PLACEMENT_3D ( 'NONE', #1046, #19268, #18606 ) ;
#27854 = CARTESIAN_POINT ( 'NONE',  ( 39.90000000000000568, 141.2096805137202580, 4.480746418436733158 ) ) ;
#27855 = CARTESIAN_POINT ( 'NONE',  ( -6.444103211790928043, 202.2591342207265939, 50.19886208192144750 ) ) ;
#27856 = EDGE_CURVE ( 'NONE', #18054, #24364, #26280, .T. ) ;
#27857 = DIRECTION ( 'NONE',  ( -1.000000000000000000, -0.000000000000000000, -0.000000000000000000 ) ) ;
#27858 = CARTESIAN_POINT ( 'NONE',  ( 73.41132485994282320, 142.2402378747194405, -9.270509831248439525 ) ) ;
#27859 = DIRECTION ( 'NONE',  ( -1.000000000000000000, 0.000000000000000000, 0.000000000000000000 ) ) ;
#27860 = CARTESIAN_POINT ( 'NONE',  ( 55.82499999726881157, 168.2552932293087906, 9.630534252274372875 ) ) ;
#27861 = CARTESIAN_POINT ( 'NONE',  ( 60.67499999726881299, 141.7447067706911810, 9.630534252274376428 ) ) ;
#27862 = CARTESIAN_POINT ( 'NONE',  ( -7.456977232089304408, 196.8216656703010301, 57.05113791807856671 ) ) ;
#27863 = CARTESIAN_POINT ( 'NONE',  ( -119.7499999999999858, -0.6872233929727689095, 35.00001199999999812 ) ) ;
#27864 = CARTESIAN_POINT ( 'NONE',  ( 12.00000000000000711, 206.9523078486586485, -0.9988620819214344415 ) ) ;
#27865 = CARTESIAN_POINT ( 'NONE',  ( -3.044812012440131443, 216.5253028482142952, 79.10113791807857808 ) ) ;
#27866 = CARTESIAN_POINT ( 'NONE',  ( 7.456977232089471386, 196.8216656703012006, 46.44886208192143329 ) ) ;
#27867 = PRODUCT_DEFINITION_FORMATION_WITH_SPECIFIED_SOURCE ( 'ANY', '', #30091, .NOT_KNOWN. ) ;
#27868 = CARTESIAN_POINT ( 'NONE',  ( -6.220909254589682469, 215.4770327129947134, 50.94886208192142618 ) ) ;
#27869 = CARTESIAN_POINT ( 'NONE',  ( -6.500000000000000000, 3.453380256388206782, -0.6809028088495794329 ) ) ;
#27870 = CARTESIAN_POINT ( 'NONE',  ( 3.662846001190051659, 195.5725841191953691, 86.60113791807857808 ) ) ;
#27871 = CARTESIAN_POINT ( 'NONE',  ( 67.81132485994280046, 159.8737954434934920, -15.00000000000012434 ) ) ;
#27872 = CARTESIAN_POINT ( 'NONE',  ( -3.135527875058821579, 197.5041725223112223, 5.901137918078566358 ) ) ;
#27873 = CARTESIAN_POINT ( 'NONE',  ( -10.00000000000000711, 206.9523078486584495, 68.49886208192143044 ) ) ;
#27874 = DIRECTION ( 'NONE',  ( 0.000000000000000000, 0.000000000000000000, -1.000000000000000000 ) ) ;
#27875 = EDGE_LOOP ( 'NONE', ( #32362, #25915 ) ) ;
#27876 = CARTESIAN_POINT ( 'NONE',  ( -0.05014649552828442242, 219.6175466908591716, 75.24886208192143044 ) ) ;
#27877 = CIRCLE ( 'NONE', #13199, 40.00000000000000711 ) ;
#27878 = VERTEX_POINT ( 'NONE', #2453 ) ;
#27879 = CARTESIAN_POINT ( 'NONE',  ( 81.17499999726882720, 145.8408176439707802, -12.60653300113719588 ) ) ;
#27880 = CARTESIAN_POINT ( 'NONE',  ( -8.000000000000008882, 206.9523078486584780, 56.49886208192145176 ) ) ;
#27881 = VECTOR ( 'NONE', #24954, 1000.000000000000114 ) ;
#27882 = EDGE_LOOP ( 'NONE', ( #5595, #27552, #12993, #10105 ) ) ;
#27883 = EDGE_CURVE ( 'NONE', #23868, #32869, #13008, .T. ) ;
#27884 = EDGE_CURVE ( 'NONE', #7373, #18104, #33524, .T. ) ;
#27885 = CARTESIAN_POINT ( 'NONE',  ( 69.82499999726879025, 168.2552932293087906, 9.630534252274372875 ) ) ;
#27886 = LINE ( 'NONE', #18015, #26575 ) ;
#27887 = DIRECTION ( 'NONE',  ( 1.000000000000000000, 0.000000000000000000, 0.000000000000000000 ) ) ;
#27888 = CARTESIAN_POINT ( 'NONE',  ( 59.92499999726881299, 164.1591823560292198, 12.60653300113718167 ) ) ;
#27889 = EDGE_CURVE ( 'NONE', #23288, #32773, #8054, .T. ) ;
#27890 = CARTESIAN_POINT ( 'NONE',  ( 8.000000000000000000, 0.000000000000000000, 0.000000000000000000 ) ) ;
#27891 = CARTESIAN_POINT ( 'NONE',  ( 10.01549611932659545, 203.7984951890123853, 40.14886208192143613 ) ) ;
#27892 = ORIENTED_EDGE ( 'NONE', *, *, #9401, .F. ) ;
#27893 = CARTESIAN_POINT ( 'NONE',  ( -63.49999999999884892, 212.5000000000003695, -3.061616997868142046E-16 ) ) ;
#27894 = AXIS2_PLACEMENT_3D ( 'NONE', #134, #15468, #12907 ) ;
#27895 =( NAMED_UNIT ( * ) SI_UNIT ( $, .STERADIAN. ) SOLID_ANGLE_UNIT ( ) );
#27896 = CARTESIAN_POINT ( 'NONE',  ( 2.241046694638796133, -6.576374040525796438, -6.171384342982452864 ) ) ;
#27897 = DIRECTION ( 'NONE',  ( -0.000000000000000000, -0.000000000000000000, 1.000000000000000000 ) ) ;
#27898 = CARTESIAN_POINT ( 'NONE',  ( 0.05014649552828262524, 198.5883022060938572, 28.74886208192144110 ) ) ;
#27899 = EDGE_CURVE ( 'NONE', #20973, #18094, #21164, .T. ) ;
#27900 = CARTESIAN_POINT ( 'NONE',  ( -8.118202686958039038, 201.1607312380087080, 66.20113791807857240 ) ) ;
#27901 = CARTESIAN_POINT ( 'NONE',  ( 45.78867513459482552, 155.0000000000000000, 15.00000000000001243 ) ) ;
#27902 = CARTESIAN_POINT ( 'NONE',  ( -6.220909254589537696, 198.5229672870051161, 42.05113791807857382 ) ) ;
#27903 = ITEM_DEFINED_TRANSFORMATION ( 'NONE', 'NONE', #5573,  #2404 ) ;
#27904 = CARTESIAN_POINT ( 'NONE',  ( 3.135527875058820690, 216.4958274776887492, 19.40113791807856813 ) ) ;
#27905 = CARTESIAN_POINT ( 'NONE',  ( 8.000000000000008882, 206.9523078486586485, 5.001137918078565114 ) ) ;
#27906 = CIRCLE ( 'NONE', #20892, 2.149999999999984812 ) ;
#27907 = DIRECTION ( 'NONE',  ( 1.000000000000000000, 0.000000000000000000, 0.000000000000000000 ) ) ;
#27908 = FACE_OUTER_BOUND ( 'NONE', #32789, .T. ) ;
#27909 = CARTESIAN_POINT ( 'NONE',  ( -12.01549611932652972, 203.1486557965464499, 33.35113791807857098 ) ) ;
#27910 = CARTESIAN_POINT ( 'NONE',  ( 6.500000000000000000, -3.752776749732574135, -6.064240316920400886 ) ) ;
#27911 = AXIS2_PLACEMENT_3D ( 'NONE', #23413, #77, #15736 ) ;
#27912 = CARTESIAN_POINT ( 'NONE',  ( 6.220909254589536808, 215.4770327129947702, 73.55113791807858092 ) ) ;
#27913 = CARTESIAN_POINT ( 'NONE',  ( -6.220909254589537696, 198.5229672870051445, 48.05113791807857382 ) ) ;
#27914 = DIRECTION ( 'NONE',  ( 0.000000000000000000, 0.7071067811865506814, 0.7071067811865442421 ) ) ;
#27915 = CARTESIAN_POINT ( 'NONE',  ( 77.50000000000000000, 155.0000000000000000, -6.938893903907228378E-15 ) ) ;
#27916 = CARTESIAN_POINT ( 'NONE',  ( 9.680171189290716072, 214.0920067884432854, 15.69886208192143684 ) ) ;
#27917 = CARTESIAN_POINT ( 'NONE',  ( 10.01549611932659367, 203.7984951890124421, 22.14886208192143613 ) ) ;
#27918 = CARTESIAN_POINT ( 'NONE',  ( 71.29999999453761461, 142.6655632788954620, 8.961492836873471646 ) ) ;
#27919 = VERTEX_POINT ( 'NONE', #5331 ) ;
#27920 = CARTESIAN_POINT ( 'NONE',  ( 7.375838497908181246, 196.7627149292499666, 59.45113791807857240 ) ) ;
#27921 = CARTESIAN_POINT ( 'NONE',  ( 8.000000000000008882, 206.9523078486586485, 77.00113791807858377 ) ) ;
#27922 = CARTESIAN_POINT ( 'NONE',  ( 9.984503880673420539, 210.2968891136705167, 36.84886208192143187 ) ) ;
#27923 = CARTESIAN_POINT ( 'NONE',  ( 75.21132485994282035, 139.2280666364260071, -4.041636747397287284E-15 ) ) ;
#27924 = VERTEX_POINT ( 'NONE', #31074 ) ;
#27925 = VECTOR ( 'NONE', #5031, 1000.000000000000000 ) ;
#27926 = ORIENTED_EDGE ( 'NONE', *, *, #7539, .T. ) ;
#27927 = ORIENTED_EDGE ( 'NONE', *, *, #3864, .F. ) ;
#27928 = PRODUCT_DEFINITION_SHAPE ( 'NONE', 'NONE',  #32279 ) ;
#27929 = EDGE_CURVE ( 'NONE', #258, #24119, #6820, .T. ) ;
#27930 =( REPRESENTATION_RELATIONSHIP ('NONE','NONE', #25663, #12832 ) REPRESENTATION_RELATIONSHIP_WITH_TRANSFORMATION ( #29796 )SHAPE_REPRESENTATION_RELATIONSHIP( ) );
#27931 = CARTESIAN_POINT ( 'NONE',  ( 58.28867513459482552, 139.2280666364260071, -4.041636747397287284E-15 ) ) ;
#27932 = CARTESIAN_POINT ( 'NONE',  ( -4.336808689942017736E-16, 7.505553499465137612, -0.8000000000000003775 ) ) ;
#27933 = ORIENTED_EDGE ( 'NONE', *, *, #31812, .F. ) ;
#27934 = AXIS2_PLACEMENT_3D ( 'NONE', #24048, #3778, #32217 ) ;
#27935 = CARTESIAN_POINT ( 'NONE',  ( 8.015496119326531499, 209.5516654185219636, 34.85113791807857098 ) ) ;
#27936 = CIRCLE ( 'NONE', #8893, 2.149999999999984812 ) ;
#27937 = FACE_OUTER_BOUND ( 'NONE', #27135, .T. ) ;
#27938 = CARTESIAN_POINT ( 'NONE',  ( 6.220909254589681581, 198.5229672870052582, 13.44886208192143151 ) ) ;
#27939 = AXIS2_PLACEMENT_3D ( 'NONE', #24025, #688, #18423 ) ;
#27940 = CARTESIAN_POINT ( 'NONE',  ( 57.87499999726880873, 171.3844434931184253, -7.942151717890134290E-15 ) ) ;
#27941 = ORIENTED_EDGE ( 'NONE', *, *, #30201, .F. ) ;
#27942 = CARTESIAN_POINT ( 'NONE',  ( -2.426778023690262742, 214.6231898156240163, 64.10113791807857808 ) ) ;
#27943 = CARTESIAN_POINT ( 'NONE',  ( 4.200000000000001954, 2.449293598294707893E-16, -2.000000000000000888 ) ) ;
#27944 =( NAMED_UNIT ( * ) PLANE_ANGLE_UNIT ( ) SI_UNIT ( $, .RADIAN. ) );
#27945 = DIRECTION ( 'NONE',  ( 0.000000000000000000, -0.5000000000000009992, -0.8660254037844380415 ) ) ;
#27946 = CARTESIAN_POINT ( 'NONE',  ( 3.135527875058981895, 197.5041725223112792, 97.59886208192143897 ) ) ;
#27947 = CARTESIAN_POINT ( 'NONE',  ( 65.17499999726881299, 145.8408176439707802, -12.60653300113719588 ) ) ;
#27948 = CARTESIAN_POINT ( 'NONE',  ( -8.118202686958039038, 201.1607312380087080, 36.20113791807857240 ) ) ;
#27949 = CARTESIAN_POINT ( 'NONE',  ( -2.346298152288380567, 2.686816014504556538, 2.727401335159862919E-15 ) ) ;
#27950 = CARTESIAN_POINT ( 'NONE',  ( 0.05014649552810505201, 217.5146222423826714, 16.25113791807856600 ) ) ;
#27951 = DIRECTION ( 'NONE',  ( 1.000000000000000000, 0.000000000000000000, 0.000000000000000000 ) ) ;
#27952 =( GEOMETRIC_REPRESENTATION_CONTEXT ( 3 ) GLOBAL_UNCERTAINTY_ASSIGNED_CONTEXT ( ( #20908 ) ) GLOBAL_UNIT_ASSIGNED_CONTEXT ( ( #19935, #6312, #14324 ) ) REPRESENTATION_CONTEXT ( 'NONE', 'WORKASPACE' ) );
#27953 = CARTESIAN_POINT ( 'NONE',  ( 85.10000000000000853, 168.7903194862797420, 4.480746418436729606 ) ) ;
#27954 = CARTESIAN_POINT ( 'NONE',  ( -2.249320974685042440, -30.45561873520117757, -1.706427272390177663 ) ) ;
#27955 = CARTESIAN_POINT ( 'NONE',  ( 32.50000000000000000, 155.0000000000000000, -15.00000000000002487 ) ) ;
#27956 = CARTESIAN_POINT ( 'NONE',  ( 0.05014649552807549926, 219.6175466908591716, 4.251137918078565114 ) ) ;
#27957 = DIRECTION ( 'NONE',  ( -1.000000000000000000, -0.000000000000000000, -0.000000000000000000 ) ) ;
#27958 = CARTESIAN_POINT ( 'NONE',  ( 52.77499999726881441, 140.1801316387863778, 4.815267126137185549 ) ) ;
#27959 = CARTESIAN_POINT ( 'NONE',  ( 9.984503880673470277, 203.7031108863295401, 44.15113791807856813 ) ) ;
#27960 = CARTESIAN_POINT ( 'NONE',  ( 84.12499999726881583, 155.0000000000000000, 15.58253174999999402 ) ) ;
#27961 = DIRECTION ( 'NONE',  ( -1.000000000000000000, -0.000000000000000000, 0.000000000000000000 ) ) ;
#27962 = CARTESIAN_POINT ( 'NONE',  ( -3.749999999999998224, -6.495190528383296247, -6.991905250253752868 ) ) ;
#27963 = AXIS2_PLACEMENT_3D ( 'NONE', #31675, #8669, #3222 ) ;
#27964 = CARTESIAN_POINT ( 'NONE',  ( 53.59999999453762598, 141.2096805137202580, -4.480746418436742040 ) ) ;
#27965 = EDGE_LOOP ( 'NONE', ( #3961, #18770, #10817, #10606 ) ) ;
#27966 = CARTESIAN_POINT ( 'NONE',  ( -0.05014649552807705357, 194.3824533091408000, 32.75113791807856956 ) ) ;
#27967 = AXIS2_PLACEMENT_3D ( 'NONE', #30494, #9208, #6815 ) ;
#27968 = CARTESIAN_POINT ( 'NONE',  ( 61.71132485994280614, 155.0000000000000000, -15.00000000000002487 ) ) ;
#27969 = CARTESIAN_POINT ( 'NONE',  ( -10.00000000000000711, 206.9523078486584495, 11.49886208192143577 ) ) ;
#27970 = CARTESIAN_POINT ( 'NONE',  ( 125.5000000000000000, 155.0000000000010800, 106.0000000000000142 ) ) ;
#27971 = ORIENTED_EDGE ( 'NONE', *, *, #24398, .F. ) ;
#27972 = CARTESIAN_POINT ( 'NONE',  ( -10.00000000000000711, 207.0476921513413515, 3.501137918078566003 ) ) ;
#27973 = CARTESIAN_POINT ( 'NONE',  ( -3.044812012440131443, 216.5253028482142952, 58.10113791807857808 ) ) ;
#27974 = ORIENTED_EDGE ( 'NONE', *, *, #26552, .T. ) ;
#27975 = CARTESIAN_POINT ( 'NONE',  ( 4.903702542908435547, 213.8346818373419751, 24.54886208192144181 ) ) ;
#27976 = CARTESIAN_POINT ( 'NONE',  ( 79.50000000000000000, 155.0000000000000000, -6.938893903907228378E-15 ) ) ;
#27977 = ORIENTED_EDGE ( 'NONE', *, *, #5564, .T. ) ;
#27978 = CARTESIAN_POINT ( 'NONE',  ( 6.444103211791042618, 202.2591342207267644, 5.301137918078567601 ) ) ;
#27979 = CARTESIAN_POINT ( 'NONE',  ( 117.5000000000000000, 102.0000000000001990, 91.79869280115065067 ) ) ;
#27980 = CARTESIAN_POINT ( 'NONE',  ( -7.375838497908014268, 196.7627149292498530, 92.04886208192142760 ) ) ;
#27981 = CARTESIAN_POINT ( 'NONE',  ( 39.27499999726880731, 149.9369285172503510, -15.58253175000000823 ) ) ;
#27982 = ORIENTED_EDGE ( 'NONE', *, *, #13893, .T. ) ;
#27983 = CARTESIAN_POINT ( 'NONE',  ( 45.52499999726881441, 169.8198683612136222, -4.815267126137197984 ) ) ;
#27984 = FACE_OUTER_BOUND ( 'NONE', #4040, .T. ) ;
#27985 = LINE ( 'NONE', #28160, #12718 ) ;
#27986 = CIRCLE ( 'NONE', #17093, 10.12668159690567649 ) ;
#27987 = CARTESIAN_POINT ( 'NONE',  ( 6.220909254589681581, 198.5229672870052582, 67.44886208192143329 ) ) ;
#27988 = CARTESIAN_POINT ( 'NONE',  ( 49.77499999726880731, 169.8198683612136222, -4.815267126137197984 ) ) ;
#27989 = DIRECTION ( 'NONE',  ( 0.000000000000000000, 0.000000000000000000, -1.000000000000000000 ) ) ;
#27990 = CARTESIAN_POINT ( 'NONE',  ( -6.139770520408369237, 215.5359834540460042, 3.951137918078566180 ) ) ;
#27991 = CARTESIAN_POINT ( 'NONE',  ( 6.500000000000000000, 3.453380256388213887, -0.6809028088495826525 ) ) ;
#27992 = EDGE_CURVE ( 'NONE', #31209, #1032, #29004, .T. ) ;
#27993 = CARTESIAN_POINT ( 'NONE',  ( 60.39999999999999147, 150.2886644046228639, -14.50000000000000888 ) ) ;
#27994 = CARTESIAN_POINT ( 'NONE',  ( 3.135527875058820690, 216.4958274776887492, 94.40113791807857524 ) ) ;
#27995 = CARTESIAN_POINT ( 'NONE',  ( 115.4999999999999858, 127.5651812191323557, -102.3881375866411645 ) ) ;
#27996 = CARTESIAN_POINT ( 'NONE',  ( -10.01549611932653860, 203.7984951890123284, 72.35113791807859229 ) ) ;
#27997 = CARTESIAN_POINT ( 'NONE',  ( -7.848314987057850800, 4.129027267381560229, -7.493854785173809319 ) ) ;
#27998 = CARTESIAN_POINT ( 'NONE',  ( 27.50000000000000355, 1.342284157770885500, -7.623296525288699970E-18 ) ) ;
#27999 = CARTESIAN_POINT ( 'NONE',  ( 7.456977232089471386, 196.8216656703012006, 91.44886208192143329 ) ) ;
#28000 = CARTESIAN_POINT ( 'NONE',  ( 61.62499999726881583, 171.3844434931184253, -7.942151717890132712E-15 ) ) ;
#28002 = EDGE_LOOP ( 'NONE', ( #6141, #32150, #28818, #19372 ) ) ;
#28001 = CARTESIAN_POINT ( 'NONE',  ( 6.220909254589536808, 215.4770327129947987, 28.55113791807856671 ) ) ;
#28003 = PLANE ( 'NONE',  #14641 ) ;
#28004 = CARTESIAN_POINT ( 'NONE',  ( 86.47499999726879594, 149.9369285172503510, 15.58253174999999580 ) ) ;
#28005 = CARTESIAN_POINT ( 'NONE',  ( 0.05014649552807549926, 219.6175466908591716, 97.25113791807856956 ) ) ;
#28006 = CARTESIAN_POINT ( 'NONE',  ( 115.4999999999999858, 183.9550983604194698, 103.9084171661920095 ) ) ;
#28007 = ORIENTED_EDGE ( 'NONE', *, *, #26879, .T. ) ;
#28008 = CARTESIAN_POINT ( 'NONE',  ( -0.05014649552828402690, 217.5146222423826714, 87.24886208192144466 ) ) ;
#28009 = CARTESIAN_POINT ( 'NONE',  ( -12.00000000000000711, 206.9523078486584780, 11.49886208192143577 ) ) ;
#28010 = DIRECTION ( 'NONE',  ( 1.000000000000000000, 0.000000000000000000, 0.000000000000000000 ) ) ;
#28011 = CARTESIAN_POINT ( 'NONE',  ( -9.984503880673473830, 210.2968891136704315, 36.65113791807855392 ) ) ;
#28012 = LINE ( 'NONE', #4678, #9631 ) ;
#28013 = CARTESIAN_POINT ( 'NONE',  ( 8.062137200540822946, 212.9164362838583315, 99.69886208192144750 ) ) ;
#28014 = B_SPLINE_CURVE_WITH_KNOTS ( 'NONE', 3,
 ( #24415, #1080, #26627, #9071, #11469, #3290, #21517, #21848, #19300, #19466 ),
 .UNSPECIFIED., .F., .F.,
 ( 4, 2, 2, 2, 4 ),
 ( 0.01606529487141865678, 0.01806591702017409581, 0.02006653916892953138, 0.02406778346644039210, 0.03207027206146211701 ),
 .UNSPECIFIED. ) ;
#28015 = DIRECTION ( 'NONE',  ( 1.000000000000000000, 0.000000000000000000, 0.000000000000000000 ) ) ;
#28016 = ORIENTED_EDGE ( 'NONE', *, *, #32608, .F. ) ;
#28017 = CARTESIAN_POINT ( 'NONE',  ( -1.750000000000016209, -3.031088913245524985, 0.000000000000000000 ) ) ;
#28018 = CARTESIAN_POINT ( 'NONE',  ( 4.903702542908435547, 213.8346818373419751, 78.54886208192142760 ) ) ;
#28019 = EDGE_CURVE ( 'NONE', #1785, #253, #12968, .T. ) ;
#28020 = ORIENTED_EDGE ( 'NONE', *, *, #3972, .T. ) ;
#28021 = CARTESIAN_POINT ( 'NONE',  ( 33.91132485994280188, 163.8167787843871110, -12.13525491562423397 ) ) ;
#28022 = ORIENTED_EDGE ( 'NONE', *, *, #29470, .F. ) ;
#28023 = CARTESIAN_POINT ( 'NONE',  ( 81.71132485994280614, 155.0000000000000000, -15.00000000000002487 ) ) ;
#28024 = CARTESIAN_POINT ( 'NONE',  ( 83.62499999726881583, 171.3844434931184253, -7.942151717890132712E-15 ) ) ;
#28025 = CARTESIAN_POINT ( 'NONE',  ( -7.500000000000000000, 4.330127018922191873, -0.9999999999999970024 ) ) ;
#28026 = CARTESIAN_POINT ( 'NONE',  ( 6.444103211791042618, 202.2591342207267644, 80.30113791807858092 ) ) ;
#28027 = FACE_OUTER_BOUND ( 'NONE', #7448, .T. ) ;
#28028 = EDGE_CURVE ( 'NONE', #18434, #10227, #15553, .T. ) ;
#28029 = FILL_AREA_STYLE_COLOUR ( '', #31744 ) ;
#28030 = CARTESIAN_POINT ( 'NONE',  ( 40.50000000000000000, 155.0000000000000000, -14.50000000000000711 ) ) ;
#28031 = CARTESIAN_POINT ( 'NONE',  ( -2.426778023690076225, 199.3768101843759553, 52.89886208192144323 ) ) ;
#28032 = ADVANCED_FACE ( 'NONE', ( #7902 ), #28672, .F. ) ;
#28033 = EDGE_CURVE ( 'NONE', #15375, #18299, #19045, .T. ) ;
#28034 = CARTESIAN_POINT ( 'NONE',  ( 10.01549611932653860, 210.2015048109876716, 1.851137918078565425 ) ) ;
#28035 = CARTESIAN_POINT ( 'NONE',  ( 73.01132485994281751, 142.2402378747194405, 9.270509831248432420 ) ) ;
#28036 = CARTESIAN_POINT ( 'NONE',  ( -119.8866434474913660, 1.374176392886222065, 35.00001199999999812 ) ) ;
#28037 = CARTESIAN_POINT ( 'NONE',  ( 57.42499999726880588, 168.2552932293087906, -9.630534252274387086 ) ) ;
#28038 = CARTESIAN_POINT ( 'NONE',  ( 69.37499999726881583, 155.0000000000000000, -15.58253175000000823 ) ) ;
#28039 = CARTESIAN_POINT ( 'NONE',  ( 7.456977232089302632, 217.1783343296989131, 61.55113791807858092 ) ) ;
#28040 = FACE_BOUND ( 'NONE', #26338, .T. ) ;
#28041 = CARTESIAN_POINT ( 'NONE',  ( -12.01549611932652972, 203.1486557965464499, 9.351137918078563871 ) ) ;
#28042 = CARTESIAN_POINT ( 'NONE',  ( -3.135527875058821579, 197.5041725223112223, 74.90113791807857524 ) ) ;
#28043 = CARTESIAN_POINT ( 'NONE',  ( -11.98450388067341876, 203.0532714938636047, 44.34886208192143897 ) ) ;
#28044 = CARTESIAN_POINT ( 'NONE',  ( 0.05014649552828275014, 196.4853777576173002, 52.74886208192143755 ) ) ;
#28045 = EDGE_CURVE ( 'NONE', #8245, #17833, #16713, .T. ) ;
#28046 = DIRECTION ( 'NONE',  ( 0.000000000000000000, 0.000000000000000000, -1.000000000000000000 ) ) ;
#28047 = CARTESIAN_POINT ( 'NONE',  ( -9.680171189290831535, 214.0920067884431148, 87.80113791807858092 ) ) ;
#28048 = CARTESIAN_POINT ( 'NONE',  ( 74.58867513459482268, 146.1832212156128890, -12.13525491562423042 ) ) ;
#28049 = CARTESIAN_POINT ( 'NONE',  ( 8.062137200540920645, 201.0835637161417822, 8.301137918078566713 ) ) ;
#28050 = CARTESIAN_POINT ( 'NONE',  ( -8.062137200540822946, 201.0835637161416400, 68.19886208192144750 ) ) ;
#28051 = DIRECTION ( 'NONE',  ( 0.000000000000000000, 0.000000000000000000, 1.000000000000000000 ) ) ;
#28052 = ORIENTED_EDGE ( 'NONE', *, *, #19753, .T. ) ;
#28053 = CARTESIAN_POINT ( 'NONE',  ( 12.00000000000000711, 207.0476921513415220, 72.99886208192144466 ) ) ;
#28054 = B_SPLINE_CURVE_WITH_KNOTS ( 'NONE', 3,
 ( #19858, #30256, #6918, #17309, #27699, #4361 ),
 .UNSPECIFIED., .F., .F.,
 ( 4, 2, 4 ),
 ( -5.145455527297706927E-06, 0.0004153350442917282917, 0.0008358155441107560776 ),
 .UNSPECIFIED. ) ;
#28055 = ORIENTED_EDGE ( 'NONE', *, *, #8485, .F. ) ;
#28056 = CARTESIAN_POINT ( 'NONE',  ( 76.17499999726881299, 164.1591823560292198, 12.60653300113718167 ) ) ;
#28057 = CARTESIAN_POINT ( 'NONE',  ( 4.984841277089891776, 200.2242689037093726, 49.44886208192144750 ) ) ;
#28058 = EDGE_CURVE ( 'NONE', #21522, #23586, #27048, .T. ) ;
#28059 = ORIENTED_EDGE ( 'NONE', *, *, #3127, .F. ) ;
#28060 = CARTESIAN_POINT ( 'NONE',  ( 71.62499999726881583, 171.3844434931184253, -7.942151717890134290E-15 ) ) ;
#28061 = CARTESIAN_POINT ( 'NONE',  ( 104.9083388212530537, 155.0000000000000000, 0.000000000000000000 ) ) ;
#28062 = CARTESIAN_POINT ( 'NONE',  ( 10.00000000000000888, 207.0000000000002842, 5.551115123125782702E-14 ) ) ;
#28063 = CARTESIAN_POINT ( 'NONE',  ( 65.32499999726881867, 164.1591823560292198, -12.60653300113719766 ) ) ;
#28064 = DIRECTION ( 'NONE',  ( -0.000000000000000000, -0.000000000000000000, 1.000000000000000000 ) ) ;
#28065 = ADVANCED_FACE ( 'NONE', ( #29502 ), #32388, .T. ) ;
#28066 = CARTESIAN_POINT ( 'NONE',  ( -6.139770520408224463, 198.4640165459539389, 38.04886208192144181 ) ) ;
#28067 = VERTEX_POINT ( 'NONE', #885 ) ;
#28068 = CARTESIAN_POINT ( 'NONE',  ( 27.50000000000000355, 15.87713240271474291, -15.54379906938135214 ) ) ;
#28069 = CARTESIAN_POINT ( 'NONE',  ( -0.2259792476677704443, -7.636022678937404606, -6.470294263593365791 ) ) ;
#28070 = CARTESIAN_POINT ( 'NONE',  ( -60.00000000000000000, -7.347880794884118356E-15, -20.00000000000000355 ) ) ;
#28071 = CARTESIAN_POINT ( 'NONE',  ( -2.517493886309087880, 214.5937144450984135, 21.09886208192143897 ) ) ;
#28072 = CARTESIAN_POINT ( 'NONE',  ( 0.05014649552810505201, 217.5146222423826714, 67.25113791807856956 ) ) ;
#28073 = DIRECTION ( 'NONE',  ( 1.000000000000000000, 0.000000000000000000, 0.000000000000000000 ) ) ;
#28074 = CARTESIAN_POINT ( 'NONE',  ( -10.01549611932653860, 203.7984951890123284, 51.35113791807858519 ) ) ;
#28075 = CONTEXT_DEPENDENT_SHAPE_REPRESENTATION ( #5929, #13340 ) ;
#28076 = CARTESIAN_POINT ( 'NONE',  ( 8.062137200540920645, 201.0835637161417822, 20.30113791807856671 ) ) ;
#28077 = CARTESIAN_POINT ( 'NONE',  ( -8.000000000000008882, 207.0476921513413515, 9.501137918078566003 ) ) ;
#28078 = CARTESIAN_POINT ( 'NONE',  ( 1.750000000000016209, -3.031088913245524985, 0.000000000000000000 ) ) ;
#28079 = CARTESIAN_POINT ( 'NONE',  ( 37.92499999726881299, 164.1591823560292198, 12.60653300113718167 ) ) ;
#28080 = CARTESIAN_POINT ( 'NONE',  ( 0.05014649552807549926, 219.6175466908591716, 31.25113791807856956 ) ) ;
#28081 = CARTESIAN_POINT ( 'NONE',  ( 110.1179863365115636, 155.0000000000000000, 32.10452846326764131 ) ) ;
#28082 = EDGE_CURVE ( 'NONE', #22384, #10127, #20003, .T. ) ;
#28083 = CARTESIAN_POINT ( 'NONE',  ( 9.984503880673470277, 203.7031108863295401, 77.15113791807857524 ) ) ;
#28084 = CARTESIAN_POINT ( 'NONE',  ( 3.135527875058820690, 216.4958274776887492, 52.40113791807857524 ) ) ;
#28085 = PLANE ( 'NONE',  #20859 ) ;
#28086 = CARTESIAN_POINT ( 'NONE',  ( 54.58867513459482268, 146.1832212156128890, -12.13525491562423042 ) ) ;
#28087 = CARTESIAN_POINT ( 'NONE',  ( 0.05014649552828288198, 194.3824533091408000, 10.74886208192143577 ) ) ;
#28088 = CARTESIAN_POINT ( 'NONE',  ( 3.135527875058981895, 197.5041725223112792, 22.59886208192143542 ) ) ;
#28089 = CARTESIAN_POINT ( 'NONE',  ( 72.09999999453764019, 159.7113355953771077, -14.50000000000000888 ) ) ;
#28090 = ORIENTED_EDGE ( 'NONE', *, *, #22842, .T. ) ;
#28091 = CARTESIAN_POINT ( 'NONE',  ( -12.01549611932652972, 203.1486557965464499, 54.35113791807857098 ) ) ;
#28092 = CARTESIAN_POINT ( 'NONE',  ( -8.015496119326531499, 204.4483345814780364, 78.35113791807857808 ) ) ;
#28093 = ADVANCED_FACE ( 'NONE', ( #6325 ), #3939, .F. ) ;
#28094 = CARTESIAN_POINT ( 'NONE',  ( -0.05014649552828403384, 217.5146222423826714, 45.24886208192143755 ) ) ;
#28095 = VECTOR ( 'NONE', #9568, 1000.000000000000000 ) ;
#28096 = FACE_BOUND ( 'NONE', #16815, .T. ) ;
#28097 = ORIENTED_EDGE ( 'NONE', *, *, #24542, .T. ) ;
#28098 = CLOSED_SHELL ( 'NONE', ( #20604, #33318, #10618, #22898, #7540, #3354, #2516, #13083, #14768, #11831, #14519, #10847, #9016, #14968, #2808, #30158, #14316, #24089, #33560, #24681, #29361, #12254, #19553, #28976, #4332, #18469, #30211, #9100, #25824, #1798, #7427, #7254, #13469, #18136, #20649, #11637, #6592, #6245, #7190, #20587 ) ) ;
#28099 = ORIENTED_EDGE ( 'NONE', *, *, #1631, .T. ) ;
#28100 = ORIENTED_EDGE ( 'NONE', *, *, #30102, .T. ) ;
#28101 = VECTOR ( 'NONE', #18526, 999.9999999999998863 ) ;
#28102 = DIRECTION ( 'NONE',  ( 0.000000000000000000, 0.000000000000000000, 1.000000000000000000 ) ) ;
#28103 = CARTESIAN_POINT ( 'NONE',  ( 5.000000000000000000, -3.513898075855363512, -2.028749999999998277 ) ) ;
#28104 = ORIENTED_EDGE ( 'NONE', *, *, #945, .F. ) ;
#28105 = CARTESIAN_POINT ( 'NONE',  ( 7.984503880673485376, 204.3529502787953902, 32.15113791807857524 ) ) ;
#28106 = CARTESIAN_POINT ( 'NONE',  ( 115.4999999999999858, 248.9486928011511679, 52.99999999999880629 ) ) ;
#28107 = CARTESIAN_POINT ( 'NONE',  ( 3.135527875058981895, 197.5041725223112792, 16.59886208192143542 ) ) ;
#28108 = CARTESIAN_POINT ( 'NONE',  ( 55.07499999726880446, 141.7447067706911810, -9.630534252274387086 ) ) ;
#28109 = VERTEX_POINT ( 'NONE', #31886 ) ;
#28110 = CARTESIAN_POINT ( 'NONE',  ( 2.426778023690261410, 199.3768101843759837, 56.60113791807857808 ) ) ;
#28111 = CARTESIAN_POINT ( 'NONE',  ( 68.58867513459482268, 146.1832212156128890, -12.13525491562423042 ) ) ;
#28112 = CARTESIAN_POINT ( 'NONE',  ( 0.000000000000000000, 0.000000000000000000, 0.000000000000000000 ) ) ;
#28113 = CARTESIAN_POINT ( 'NONE',  ( 9.984503880673420539, 210.2968891136705167, 96.84886208192139634 ) ) ;
#28114 = CARTESIAN_POINT ( 'NONE',  ( 67.17499999726881299, 145.8408176439707802, -12.60653300113719588 ) ) ;
#28115 = CARTESIAN_POINT ( 'NONE',  ( -9.984503880673473830, 210.2968891136704315, 39.65113791807857524 ) ) ;
#28116 = CARTESIAN_POINT ( 'NONE',  ( 70.78867513459482552, 155.0000000000000000, -15.00000000000002487 ) ) ;
#28117 = CARTESIAN_POINT ( 'NONE',  ( -0.05014649552810635652, 196.4853777576173002, 17.75113791807856245 ) ) ;
#28118 = CYLINDRICAL_SURFACE ( 'NONE', #28255, 15.00000000000001776 ) ;
#28119 = AXIS2_PLACEMENT_3D ( 'NONE', #19371, #9486, #12041 ) ;
#28120 = PRODUCT_CONTEXT ( 'NONE', #13745, 'mechanical' ) ;
#28121 = CIRCLE ( 'NONE', #8021, 10.62447292484156947 ) ;
#28122 = CARTESIAN_POINT ( 'NONE',  ( 33.42499999726881299, 168.2552932293087906, -9.630534252274385310 ) ) ;
#28123 = DIRECTION ( 'NONE',  ( 1.000000000000000000, 0.000000000000000000, 0.000000000000000000 ) ) ;
#28124 = CYLINDRICAL_SURFACE ( 'NONE', #14163, 15.00000000000001776 ) ;
#28125 = CARTESIAN_POINT ( 'NONE',  ( 0.05014649552807549926, 219.6175466908591716, 1.251137918078565558 ) ) ;
#28126 = CARTESIAN_POINT ( 'NONE',  ( 25.25067902531501574, -17.17577847294299076, -1.706427272390178773 ) ) ;
#28127 = CARTESIAN_POINT ( 'NONE',  ( 51.67499999726879878, 168.2552932293087906, -9.630534252274385310 ) ) ;
#28128 = ADVANCED_FACE ( 'NONE', ( #9052 ), #20568, .F. ) ;
#28129 = CARTESIAN_POINT ( 'NONE',  ( -0.05014649552810635652, 196.4853777576173002, 47.75113791807855534 ) ) ;
#28130 = EDGE_CURVE ( 'NONE', #17333, #28277, #26724, .T. ) ;
#28131 = CARTESIAN_POINT ( 'NONE',  ( 32.50000000000000000, 155.0000000000000000, -6.938893903907228378E-15 ) ) ;
#28132 = DIRECTION ( 'NONE',  ( -0.1045284632676468234, 0.000000000000000000, 0.9945218953682740670 ) ) ;
#28133 = CYLINDRICAL_SURFACE ( 'NONE', #12469, 15.00000000000001776 ) ;
#28134 = CARTESIAN_POINT ( 'NONE',  ( 56.09999999453763309, 159.7113355953771077, -14.50000000000000888 ) ) ;
#28135 = ORIENTED_EDGE ( 'NONE', *, *, #8078, .T. ) ;
#28136 = CARTESIAN_POINT ( 'NONE',  ( 9.680171189290831535, 199.9079932115568852, 32.30113791807855961 ) ) ;
#28137 = EDGE_CURVE ( 'NONE', #22347, #2881, #3703, .T. ) ;
#28138 = EDGE_CURVE ( 'NONE', #21331, #33564, #31723, .T. ) ;
#28139 = CARTESIAN_POINT ( 'NONE',  ( 32.50000000000000000, 155.0000000000000000, 15.00000000000001243 ) ) ;
#28140 = CARTESIAN_POINT ( 'NONE',  ( 6.139770520408223575, 215.5359834540460611, 15.54886208192143293 ) ) ;
#28141 = APPLICATION_CONTEXT ( 'automotive_design' ) ;
#28142 = LINE ( 'NONE', #30877, #15587 ) ;
#28143 = ORIENTED_EDGE ( 'NONE', *, *, #9364, .T. ) ;
#28144 = CARTESIAN_POINT ( 'NONE',  ( 8.118202686958039038, 212.8392687619912635, 10.70113791807856529 ) ) ;
#28145 = CARTESIAN_POINT ( 'NONE',  ( 10.01549611932653860, 210.2015048109876716, 58.85113791807856387 ) ) ;
#28146 = CIRCLE ( 'NONE', #25415, 24.99999999999999289 ) ;
#28147 = ORIENTED_EDGE ( 'NONE', *, *, #164, .T. ) ;
#28148 = CARTESIAN_POINT ( 'NONE',  ( 4.903702542908435547, 213.8346818373419751, 21.54886208192143471 ) ) ;
#28149 = STYLED_ITEM ( 'NONE', ( #9149 ), #23813 ) ;
#28150 = CIRCLE ( 'NONE', #33600, 4.250000000000000000 ) ;
#28151 = DIRECTION ( 'NONE',  ( 0.000000000000000000, 0.000000000000000000, 1.000000000000000000 ) ) ;
#28152 = ORIENTED_EDGE ( 'NONE', *, *, #32280, .T. ) ;
#28153 = CARTESIAN_POINT ( 'NONE',  ( -2.517493886308901807, 199.4062855549015012, 5.901137918078568134 ) ) ;
#28154 = CARTESIAN_POINT ( 'NONE',  ( 3.662846001189864698, 218.4274158808046593, 93.39886208192143613 ) ) ;
#28155 = CARTESIAN_POINT ( 'NONE',  ( 39.17499999726881299, 145.8408176439707802, -12.60653300113719588 ) ) ;
#28157 = VERTEX_POINT ( 'NONE', #26607 ) ;
#28156 = VECTOR ( 'NONE', #32937, 1000.000000000000000 ) ;
#28158 = CARTESIAN_POINT ( 'NONE',  ( 45.62499999726880162, 171.3844434931184253, -7.942151717890132712E-15 ) ) ;
#28159 = CARTESIAN_POINT ( 'NONE',  ( 5.000000000000000000, 2.342598717236910488, 4.057499999999995666 ) ) ;
#28160 = CARTESIAN_POINT ( 'NONE',  ( -63.50000000000004263, 215.0000000000000000, 2.500000000000000000 ) ) ;
#28161 = CARTESIAN_POINT ( 'NONE',  ( 10.00000000000000711, 207.0476921513415220, 69.99886208192143044 ) ) ;
#28162 = CARTESIAN_POINT ( 'NONE',  ( 49.07499999726880446, 141.7447067706911810, -9.630534252274385310 ) ) ;
#28163 = CARTESIAN_POINT ( 'NONE',  ( -67.50001199999996970, 138.5437169723398085, 4.407803664655115305 ) ) ;
#28164 = CARTESIAN_POINT ( 'NONE',  ( -3.044812012440131443, 216.5253028482142952, 16.10113791807856742 ) ) ;
#28165 = CARTESIAN_POINT ( 'NONE',  ( 117.5000000000000000, 257.3881375866408803, -27.43481878086871717 ) ) ;
#28166 = CARTESIAN_POINT ( 'NONE',  ( 69.50000000000000000, 155.0000000000000000, 14.49999999999999467 ) ) ;
#28167 =( BOUNDED_CURVE ( )  B_SPLINE_CURVE ( 3, ( #3945, #24900, #14840, #14344 ),
 .UNSPECIFIED., .F., .T. ) 
 B_SPLINE_CURVE_WITH_KNOTS ( ( 4, 4 ),
 ( 2.616713720088120532, 3.141592653589793116 ),
 .UNSPECIFIED. ) 
 CURVE ( )  GEOMETRIC_REPRESENTATION_ITEM ( )  RATIONAL_B_SPLINE_CURVE ( ( 1.000000000000000000, 0.9771733092046011038, 0.9771733092046011038, 1.000000000000000000 ) ) 
 REPRESENTATION_ITEM ( '' )  );
#28168 = CARTESIAN_POINT ( 'NONE',  ( -3.044812012440131443, 216.5253028482142952, 94.10113791807857808 ) ) ;
#28169 = CARTESIAN_POINT ( 'NONE',  ( 64.50000000000000000, -103.0000000000000000, -30.00000000000000000 ) ) ;
#28170 = CARTESIAN_POINT ( 'NONE',  ( -10.00000000000000711, 207.0476921513413515, 75.50113791807858377 ) ) ;
#28171 = AXIS2_PLACEMENT_3D ( 'NONE', #3218, #13604, #999 ) ;
#28172 = CARTESIAN_POINT ( 'NONE',  ( -5.000000000000001776, 0.000000000000000000, -9.974600000000000577 ) ) ;
#28173 = CARTESIAN_POINT ( 'NONE',  ( 33.47499999726881015, 160.0630714827496206, -15.58253175000000823 ) ) ;
#28174 = CARTESIAN_POINT ( 'NONE',  ( -3.662846001189865142, 195.5725841191952838, 91.89886208192143613 ) ) ;
#28175 = AXIS2_PLACEMENT_3D ( 'NONE', #29399, #6047, #16439 ) ;
#28176 = CARTESIAN_POINT ( 'NONE',  ( 68.92499999726881299, 145.8408176439707802, -12.60653300113719588 ) ) ;
#28177 = AXIS2_PLACEMENT_3D ( 'NONE', #8298, #3013, #10688 ) ;
#28179 = ORIENTED_EDGE ( 'NONE', *, *, #30113, .F. ) ;
#28178 = CARTESIAN_POINT ( 'NONE',  ( 6.139770520408367460, 198.4640165459539389, 29.45113791807856884 ) ) ;
#28180 = CARTESIAN_POINT ( 'NONE',  ( 7.500000000000000000, 4.330127018922190096, -7.422398894150032511 ) ) ;
#28181 = CARTESIAN_POINT ( 'NONE',  ( 35.99999999453763166, 155.0000000000000000, -14.50000000000000711 ) ) ;
#28182 = CARTESIAN_POINT ( 'NONE',  ( -9.736236675707914401, 199.9851607334237542, 99.20113791807858661 ) ) ;
#28183 = CARTESIAN_POINT ( 'NONE',  ( 90.49452189536829394, 155.0000000000000000, 0.000000000000000000 ) ) ;
#28184 = VECTOR ( 'NONE', #9390, 1000.000000000000000 ) ;
#28185 = EDGE_LOOP ( 'NONE', ( #13513, #12259 ) ) ;
#28186 = CARTESIAN_POINT ( 'NONE',  ( -10.01549611932659545, 210.2015048109875011, 86.64886208192142192 ) ) ;
#28187 = CARTESIAN_POINT ( 'NONE',  ( 3.753561863808876797, 195.6020594897209719, 25.59886208192143897 ) ) ;
#28188 = DIRECTION ( 'NONE',  ( -1.000000000000000000, -0.000000000000000000, 0.000000000000000000 ) ) ;
#28189 = CARTESIAN_POINT ( 'NONE',  ( 6.220909254589536808, 215.4770327129947702, 34.55113791807855250 ) ) ;
#28190 = CARTESIAN_POINT ( 'NONE',  ( 66.78867513459482552, 155.0000000000000000, -15.00000000000002487 ) ) ;
#28191 = CARTESIAN_POINT ( 'NONE',  ( 6.139770520408223575, 215.5359834540460611, 102.5488620819214134 ) ) ;
#28192 = CARTESIAN_POINT ( 'NONE',  ( 5.727634848076855967, 4.575561887447700649, -6.326622577870477215 ) ) ;
#28193 = ORIENTED_EDGE ( 'NONE', *, *, #22701, .T. ) ;
#28194 = CARTESIAN_POINT ( 'NONE',  ( 4.336808689942017736E-16, 8.660254037844390851, -1.000000000000000888 ) ) ;
#28195 = CARTESIAN_POINT ( 'NONE',  ( 4.984841277089891776, 200.2242689037093726, 76.44886208192143329 ) ) ;
#28196 = CIRCLE ( 'NONE', #23304, 3.499999999999999556 ) ;
#28197 = ORIENTED_EDGE ( 'NONE', *, *, #17799, .T. ) ;
#28198 = CARTESIAN_POINT ( 'NONE',  ( 0.000000000000000000, 0.000000000000000000, 0.000000000000000000 ) ) ;
#28199 = ORIENTED_EDGE ( 'NONE', *, *, #32082, .T. ) ;
#28200 = CARTESIAN_POINT ( 'NONE',  ( 2.000000000000000000, -0.8865213383406685965, 1.535500000000000531 ) ) ;
#28201 = CARTESIAN_POINT ( 'NONE',  ( 6.500168698208129925, 211.6636982574063381, 58.70113791807857240 ) ) ;
#28202 = CARTESIAN_POINT ( 'NONE',  ( 80.42499999726879878, 141.7447067706911810, 9.630534252274376428 ) ) ;
#28203 = DIRECTION ( 'NONE',  ( 1.000000000000000000, 0.000000000000000000, 0.000000000000000000 ) ) ;
#28204 = CARTESIAN_POINT ( 'NONE',  ( 8.015496119326531499, 209.5516654185219636, 76.85113791807856387 ) ) ;
#28205 = DIRECTION ( 'NONE',  ( 0.000000000000000000, 0.000000000000000000, -1.000000000000000000 ) ) ;
#28206 = AXIS2_PLACEMENT_3D ( 'NONE', #23974, #8638, #29593 ) ;
#28207 = SURFACE_SIDE_STYLE ('',( #25306 ) ) ;
#28208 = CARTESIAN_POINT ( 'NONE',  ( 48.10000000000000142, 141.2096805137202580, -4.480746418436742040 ) ) ;
#28209 = CARTESIAN_POINT ( 'NONE',  ( -4.903702542908436435, 200.1653181626580249, 68.04886208192144181 ) ) ;
#28210 = DIRECTION ( 'NONE',  ( 0.000000000000000000, 0.000000000000000000, -1.000000000000000000 ) ) ;
#28211 = CARTESIAN_POINT ( 'NONE',  ( -6.838238953609876880, 3.993985489099932007, -6.572971244646267586 ) ) ;
#28212 = LINE ( 'NONE', #4475, #22407 ) ;
#28213 = CARTESIAN_POINT ( 'NONE',  ( 57.72499999726881015, 169.8198683612136222, 4.815267126137181997 ) ) ;
#28214 = CARTESIAN_POINT ( 'NONE',  ( 68.67499999726879878, 141.7447067706911810, 9.630534252274376428 ) ) ;
#28215 = CARTESIAN_POINT ( 'NONE',  ( 3.753561863808689836, 218.3979405102790565, 64.40113791807856103 ) ) ;
#28216 = DIRECTION ( 'NONE',  ( 0.000000000000000000, 0.000000000000000000, -1.000000000000000000 ) ) ;
#28217 = CIRCLE ( 'NONE', #18422, 2.000000000000000000 ) ;
#28218 = PRODUCT_DEFINITION_SHAPE ( 'NONE', 'NONE',  #18980 ) ;
#28219 = CARTESIAN_POINT ( 'NONE',  ( -9.680171189290831535, 214.0920067884431148, 9.801137918078564937 ) ) ;
#28220 = CARTESIAN_POINT ( 'NONE',  ( 10.01549611932653860, 210.2015048109876716, 85.85113791807857808 ) ) ;
#28221 = AXIS2_PLACEMENT_3D ( 'NONE', #7669, #28281, #3371 ) ;
#28222 = CARTESIAN_POINT ( 'NONE',  ( -7.375838497908014268, 196.7627149292498530, 56.04886208192144181 ) ) ;
#28223 = CARTESIAN_POINT ( 'NONE',  ( -9.984503880673420539, 203.7031108863293980, 53.34886208192144608 ) ) ;
#28224 = DIRECTION ( 'NONE',  ( 1.000000000000000000, 0.000000000000000000, -0.000000000000000000 ) ) ;
#28225 = CARTESIAN_POINT ( 'NONE',  ( -7.375838497908182134, 217.2372850707499765, 96.95113791807857240 ) ) ;
#28226 = DIRECTION ( 'NONE',  ( 1.000000000000000000, -0.000000000000000000, -0.000000000000000000 ) ) ;
#28227 = CARTESIAN_POINT ( 'NONE',  ( -10.01549611932653860, 203.7984951890123284, 0.3511379180785655363 ) ) ;
#28228 = CARTESIAN_POINT ( 'NONE',  ( 6.139770520408223575, 215.5359834540460611, 66.54886208192144181 ) ) ;
#28229 = EDGE_CURVE ( 'NONE', #11543, #9113, #15017, .T. ) ;
#28230 = CARTESIAN_POINT ( 'NONE',  ( 89.50000000000001421, 155.0000000000000000, -6.938893903907228378E-15 ) ) ;
#28231 = VECTOR ( 'NONE', #22172, 1000.000000000000000 ) ;
#28232 = ORIENTED_EDGE ( 'NONE', *, *, #13542, .T. ) ;
#28233 = CARTESIAN_POINT ( 'NONE',  ( 12.00000000000000711, 207.0476921513415220, 66.99886208192144466 ) ) ;
#28234 = CARTESIAN_POINT ( 'NONE',  ( 6.220909254589536808, 215.4770327129947702, 85.55113791807858092 ) ) ;
#28235 = EDGE_LOOP ( 'NONE', ( #10955, #32114 ) ) ;
#28236 = CARTESIAN_POINT ( 'NONE',  ( 77.07499999726881867, 141.7447067706911810, -9.630534252274385310 ) ) ;
#28237 = CARTESIAN_POINT ( 'NONE',  ( -6.500168698208244500, 211.6636982574061676, 53.79886208192144892 ) ) ;
#28238 = ORIENTED_EDGE ( 'NONE', *, *, #10027, .T. ) ;
#28239 = CARTESIAN_POINT ( 'NONE',  ( 72.12499999726881583, 155.0000000000000000, 15.58253174999999402 ) ) ;
#28240 = DIRECTION ( 'NONE',  ( -1.000000000000000000, 0.000000000000000000, 0.000000000000000000 ) ) ;
#28241 = CARTESIAN_POINT ( 'NONE',  ( 117.5000000000000000, 155.0000000000000000, -112.0000000000000426 ) ) ;
#28242 = VECTOR ( 'NONE', #18991, 1000.000000000000000 ) ;
#28243 = CARTESIAN_POINT ( 'NONE',  ( 66.32499999726881867, 145.8408176439707802, 12.60653300113718345 ) ) ;
#28244 = CARTESIAN_POINT ( 'NONE',  ( -125.0000000000000000, -25.00000000000000000, 20.00000000000000000 ) ) ;
#28245 = CARTESIAN_POINT ( 'NONE',  ( 9.984503880673420539, 210.2968891136705167, 54.84886208192141765 ) ) ;
#28246 = ORIENTED_EDGE ( 'NONE', *, *, #25595, .T. ) ;
#28247 = DIRECTION ( 'NONE',  ( 0.000000000000000000, 0.7071067811865434649, -0.7071067811865515695 ) ) ;
#28248 = ORIENTED_EDGE ( 'NONE', *, *, #31855, .F. ) ;
#28249 = LINE ( 'NONE', #15290, #18308 ) ;
#28250 = FACE_OUTER_BOUND ( 'NONE', #22690, .T. ) ;
#28251 = CARTESIAN_POINT ( 'NONE',  ( 4.984841277089891776, 200.2242689037093726, 34.44886208192144039 ) ) ;
#28252 = CARTESIAN_POINT ( 'NONE',  ( 6.220909254589536808, 215.4770327129947702, 73.55113791807858092 ) ) ;
#28253 = DIRECTION ( 'NONE',  ( 0.000000000000000000, 0.000000000000000000, -1.000000000000000000 ) ) ;
#28254 = CARTESIAN_POINT ( 'NONE',  ( -6.139770520408369237, 215.5359834540460042, 57.95113791807856529 ) ) ;
#28255 = AXIS2_PLACEMENT_3D ( 'NONE', #15175, #33407, #25567 ) ;
#28256 = CONTEXT_DEPENDENT_SHAPE_REPRESENTATION ( #16828, #29120 ) ;
#28257 = CARTESIAN_POINT ( 'NONE',  ( -9.984503880673473830, 210.2968891136704315, 30.65113791807856813 ) ) ;
#28258 = CARTESIAN_POINT ( 'NONE',  ( -8.015496119326531499, 204.4483345814780364, 6.351137918078565647 ) ) ;
#28259 = CARTESIAN_POINT ( 'NONE',  ( 87.27499999726880731, 149.9369285172503510, -15.58253175000000823 ) ) ;
#28260 = DIRECTION ( 'NONE',  ( 1.000000000000000000, 0.000000000000000000, 0.000000000000000000 ) ) ;
#28261 = CARTESIAN_POINT ( 'NONE',  ( 40.32499999726881157, 145.8408176439707802, 12.60653300113718345 ) ) ;
#28262 = CARTESIAN_POINT ( 'NONE',  ( 9.680171189290831535, 199.9079932115568852, 41.30113791807857382 ) ) ;
#28263 = DIRECTION ( 'NONE',  ( 0.000000000000000000, 0.000000000000000000, -1.000000000000000000 ) ) ;
#28264 = CARTESIAN_POINT ( 'NONE',  ( 9.984503880673470277, 203.7031108863295401, 86.15113791807857524 ) ) ;
#28265 = CARTESIAN_POINT ( 'NONE',  ( -9.984503880673475606, 210.2968891136704315, 51.65113791807855392 ) ) ;
#28266 = PLANE ( 'NONE',  #7803 ) ;
#28267 = CARTESIAN_POINT ( 'NONE',  ( -11.98450388067341876, 203.0532714938636047, 17.34886208192143187 ) ) ;
#28268 = CARTESIAN_POINT ( 'NONE',  ( 8.118202686958138514, 201.1607312380088501, 25.29886208192143826 ) ) ;
#28269 = CARTESIAN_POINT ( 'NONE',  ( 73.59999999453762598, 141.2096805137202580, -4.480746418436742040 ) ) ;
#28270 = VERTEX_POINT ( 'NONE', #21326 ) ;
#28271 = CARTESIAN_POINT ( 'NONE',  ( 7.375838497908181246, 196.7627149292499666, 65.45113791807858661 ) ) ;
#28272 = AXIS2_PLACEMENT_3D ( 'NONE', #15520, #2074, #5295 ) ;
#28273 = CARTESIAN_POINT ( 'NONE',  ( 0.05014649552807626948, 215.4116977939061144, 79.25113791807856956 ) ) ;
#28274 = CARTESIAN_POINT ( 'NONE',  ( -6.139770520408224463, 198.4640165459539389, 38.04886208192144181 ) ) ;
#28275 = EDGE_CURVE ( 'NONE', #3255, #29401, #24395, .T. ) ;
#28276 = FACE_OUTER_BOUND ( 'NONE', #18420, .T. ) ;
#28277 = VERTEX_POINT ( 'NONE', #19786 ) ;
#28278 = CARTESIAN_POINT ( 'NONE',  ( 9.736236675708031640, 199.9851607334238963, 46.29886208192144181 ) ) ;
#28279 = VERTEX_POINT ( 'NONE', #22167 ) ;
#28280 = ORIENTED_EDGE ( 'NONE', *, *, #27511, .F. ) ;
#28281 = DIRECTION ( 'NONE',  ( 1.000000000000000000, 0.000000000000000000, 0.000000000000000000 ) ) ;
#28282 = EDGE_CURVE ( 'NONE', #28362, #21367, #29266, .T. ) ;
#28283 = CARTESIAN_POINT ( 'NONE',  ( 2.000000000000000000, 1.773042676681340968, -2.276824562219559311E-15 ) ) ;
#28284 = EDGE_LOOP ( 'NONE', ( #8907, #944, #1608, #13060, #3288, #9706 ) ) ;
#28285 = CARTESIAN_POINT ( 'NONE',  ( -7.984503880673488041, 209.6470497212046098, 39.65113791807857524 ) ) ;
#28286 = CARTESIAN_POINT ( 'NONE',  ( 82.11132485994279762, 169.2658477444273331, -4.635254915624224203 ) ) ;
#28287 = CARTESIAN_POINT ( 'NONE',  ( 9.984503880673420539, 210.2968891136705167, 21.84886208192143542 ) ) ;
#28288 = CARTESIAN_POINT ( 'NONE',  ( 57.17499999726881299, 145.8408176439707802, -12.60653300113719588 ) ) ;
#28289 = EDGE_LOOP ( 'NONE', ( #6601, #28059, #2344, #25160 ) ) ;
#28290 = CARTESIAN_POINT ( 'NONE',  ( 8.015496119326531499, 209.5516654185219636, 61.85113791807857098 ) ) ;
#28291 = CARTESIAN_POINT ( 'NONE',  ( 4.406842699996126989, -6.115962218725295330, -6.291760732204942919E-15 ) ) ;
#28292 = SURFACE_STYLE_USAGE ( .BOTH. , #2398 ) ;
#28293 = CARTESIAN_POINT ( 'NONE',  ( -1.306442393143578462, -8.377108146505394259, -7.792327460285862983 ) ) ;
#28294 = CARTESIAN_POINT ( 'NONE',  ( -10.01549611932659722, 210.2015048109875011, 98.64886208192143613 ) ) ;
#28295 = CARTESIAN_POINT ( 'NONE',  ( 67.77499999726880731, 169.8198683612136222, -4.815267126137197984 ) ) ;
#28296 = CARTESIAN_POINT ( 'NONE',  ( -10.01549611932653860, 203.7984951890123284, 42.35113791807855677 ) ) ;
#28297 =( NAMED_UNIT ( * ) SI_UNIT ( $, .STERADIAN. ) SOLID_ANGLE_UNIT ( ) );
#28298 = EDGE_CURVE ( 'NONE', #25373, #5220, #12119, .T. ) ;
#28299 = CARTESIAN_POINT ( 'NONE',  ( 9.984503880673470277, 203.7031108863295401, 23.15113791807856813 ) ) ;
#28300 = CARTESIAN_POINT ( 'NONE',  ( 0.05014649552828275014, 196.4853777576173002, 100.7488620819214304 ) ) ;
#28301 = CARTESIAN_POINT ( 'NONE',  ( 4.984841277089891776, 200.2242689037093726, 82.44886208192144750 ) ) ;
#28302 = CARTESIAN_POINT ( 'NONE',  ( 87.50000000000000000, 155.0000000000000000, 14.49999999999999467 ) ) ;
#28303 = CARTESIAN_POINT ( 'NONE',  ( 32.50000000000000000, 155.0000000000000000, -6.938893903907228378E-15 ) ) ;
#28304 = CARTESIAN_POINT ( 'NONE',  ( 9.736236675707914401, 214.0148392665762458, 4.701137918078565292 ) ) ;
#28305 = CARTESIAN_POINT ( 'NONE',  ( -0.04606493828583551470, -9.175055303659563677, -8.057411785091794343 ) ) ;
#28306 = CARTESIAN_POINT ( 'NONE',  ( 51.37499999726881583, 155.0000000000000000, -15.58253175000000823 ) ) ;
#28307 = EDGE_CURVE ( 'NONE', #29401, #23763, #7521, .T. ) ;
#28308 = CARTESIAN_POINT ( 'NONE',  ( -8.118202686958039038, 201.1607312380087080, 60.20113791807857240 ) ) ;
#28309 = CARTESIAN_POINT ( 'NONE',  ( 86.72499999726882436, 140.1801316387863778, -4.815267126137194431 ) ) ;
#28310 = CARTESIAN_POINT ( 'NONE',  ( 0.000000000000000000, 0.000000000000000000, -8.000000000000000000 ) ) ;
#28311 = CARTESIAN_POINT ( 'NONE',  ( -68.50000000000000000, 215.0000000000000000, 0.000000000000000000 ) ) ;
#28312 = CARTESIAN_POINT ( 'NONE',  ( 53.79999999453763593, 146.4771138417591203, -11.73074641843674470 ) ) ;
#28313 = EDGE_LOOP ( 'NONE', ( #1873, #9362, #31946, #6268 ) ) ;
#28314 = CARTESIAN_POINT ( 'NONE',  ( -9.736236675707914401, 199.9851607334237542, 33.20113791807856529 ) ) ;
#28315 = FACE_OUTER_BOUND ( 'NONE', #32293, .T. ) ;
#28316 = CARTESIAN_POINT ( 'NONE',  ( -3.044812012439970683, 197.4746971517856196, 10.89886208192143613 ) ) ;
#28317 = CARTESIAN_POINT ( 'NONE',  ( 115.4999999999999858, 102.0000000000001990, 91.79869280115065067 ) ) ;
#28318 = VERTEX_POINT ( 'NONE', #33241 ) ;
#28319 = CARTESIAN_POINT ( 'NONE',  ( -10.01549611932653860, 203.7984951890123284, 6.351137918078566535 ) ) ;
#28320 = CARTESIAN_POINT ( 'NONE',  ( -8.062137200540920645, 212.9164362838581894, 75.80113791807858092 ) ) ;
#28321 = EDGE_LOOP ( 'NONE', ( #17633, #9413, #4753 ) ) ;
#28322 = CARTESIAN_POINT ( 'NONE',  ( 6.444103211790928043, 211.7408657792734061, 30.69886208192143684 ) ) ;
#28323 = CARTESIAN_POINT ( 'NONE',  ( 44.71132485994280614, 155.0000000000000000, 15.00000000000001243 ) ) ;
#28324 = EDGE_LOOP ( 'NONE', ( #4460, #10930, #9798, #489, #5236, #5027 ) ) ;
#28325 = CARTESIAN_POINT ( 'NONE',  ( -4.984841277089726574, 200.2242689037092305, 0.05113791807856601229 ) ) ;
#28326 = EDGE_CURVE ( 'NONE', #12982, #3377, #9229, .T. ) ;
#28327 = ADVANCED_FACE ( 'NONE', ( #17397 ), #30515, .T. ) ;
#28328 = CARTESIAN_POINT ( 'NONE',  ( -3.753561863808878130, 218.3979405102790281, 87.09886208192143897 ) ) ;
#28329 = CARTESIAN_POINT ( 'NONE',  ( 40.17499999726881299, 164.1591823560292198, 12.60653300113718167 ) ) ;
#28330 = ORIENTED_EDGE ( 'NONE', *, *, #9297, .F. ) ;
#28331 = CARTESIAN_POINT ( 'NONE',  ( 43.82499999726881157, 168.2552932293087906, 9.630534252274372875 ) ) ;
#28332 = DIRECTION ( 'NONE',  ( 0.000000000000000000, 0.000000000000000000, 1.000000000000000000 ) ) ;
#28333 = CARTESIAN_POINT ( 'NONE',  ( -6.220909254589537696, 198.5229672870051161, 6.051137918078566713 ) ) ;
#28334 = CIRCLE ( 'NONE', #4933, 2.149999999999985256 ) ;
#28335 = CARTESIAN_POINT ( 'NONE',  ( 6.139770520408223575, 215.5359834540460611, 72.54886208192144181 ) ) ;
#28337 = CARTESIAN_POINT ( 'NONE',  ( 45.27499999726880020, 149.9369285172503510, -15.58253175000000823 ) ) ;
#28336 = PRODUCT_DEFINITION ( 'UNKNOWN', '', #28422, #8740 ) ;
#28338 = CARTESIAN_POINT ( 'NONE',  ( -67.50000599999999906, 155.0000000000000000, -17.00000000000000711 ) ) ;
#28339 = CARTESIAN_POINT ( 'NONE',  ( 3.044812012440130555, 197.4746971517856764, 11.60113791807856742 ) ) ;
#28340 = CARTESIAN_POINT ( 'NONE',  ( 117.5000000000000000, 155.0000000000000000, 99.99999999999997158 ) ) ;
#28341 = EDGE_CURVE ( 'NONE', #3832, #20128, #20027, .T. ) ;
#28342 = CARTESIAN_POINT ( 'NONE',  ( 69.00000000000001421, 170.2462022514548323, -7.872454543227099337E-15 ) ) ;
#28343 = CARTESIAN_POINT ( 'NONE',  ( 10.00000000000000711, 206.9523078486586201, 95.00113791807856956 ) ) ;
#28344 = FACE_OUTER_BOUND ( 'NONE', #10145, .T. ) ;
#28345 = CARTESIAN_POINT ( 'NONE',  ( 6.139770520408368348, 198.4640165459539674, 74.45113791807857240 ) ) ;
#28346 = CARTESIAN_POINT ( 'NONE',  ( 57.08867513459483689, 167.7597621252805880, -9.270509831248443078 ) ) ;
#28347 = DIRECTION ( 'NONE',  ( -1.000000000000000000, -0.000000000000000000, -0.000000000000000000 ) ) ;
#28348 = EDGE_CURVE ( 'NONE', #13595, #20519, #17058, .T. ) ;
#28349 = CARTESIAN_POINT ( 'NONE',  ( -3.753561863808878130, 218.3979405102790281, 90.09886208192143897 ) ) ;
#28350 = CARTESIAN_POINT ( 'NONE',  ( 68.42499999726881299, 141.7447067706911810, 9.630534252274376428 ) ) ;
#28351 = ORIENTED_EDGE ( 'NONE', *, *, #2287, .T. ) ;
#28352 = CARTESIAN_POINT ( 'NONE',  ( -58.66522414286995968, 194.9217985566782545, 2.500000000000000444 ) ) ;
#28353 = CARTESIAN_POINT ( 'NONE',  ( 36.89999999453762314, 159.7113355953771077, 14.49999999999999289 ) ) ;
#28354 = CARTESIAN_POINT ( 'NONE',  ( 12.01549611932652972, 210.8513442034534933, 97.85113791807857808 ) ) ;
#28355 = FACE_OUTER_BOUND ( 'NONE', #23619, .T. ) ;
#28356 = ORIENTED_EDGE ( 'NONE', *, *, #19498, .T. ) ;
#28357 = CARTESIAN_POINT ( 'NONE',  ( 8.062137200540822946, 212.9164362838583315, 81.69886208192143329 ) ) ;
#28358 = VECTOR ( 'NONE', #7126, 1000.000000000000000 ) ;
#28359 = CARTESIAN_POINT ( 'NONE',  ( -9.736236675708031640, 214.0148392665760753, 20.79886208192143826 ) ) ;
#28360 = LINE ( 'NONE', #15404, #16984 ) ;
#28361 = CARTESIAN_POINT ( 'NONE',  ( -8.062137200540920645, 212.9164362838581894, 42.80113791807857382 ) ) ;
#28362 = VERTEX_POINT ( 'NONE', #27783 ) ;
#28363 = CARTESIAN_POINT ( 'NONE',  ( 8.118202686958138514, 201.1607312380088501, 97.29886208192144181 ) ) ;
#28364 = DIRECTION ( 'NONE',  ( -1.000000000000000000, -0.000000000000000000, -0.000000000000000000 ) ) ;
#28365 = ORIENTED_EDGE ( 'NONE', *, *, #23511, .F. ) ;
#28366 = CARTESIAN_POINT ( 'NONE',  ( 8.000000000000008882, 207.0476921513415220, 84.99886208192144466 ) ) ;
#28367 = VERTEX_POINT ( 'NONE', #14671 ) ;
#28368 = FACE_OUTER_BOUND ( 'NONE', #31254, .T. ) ;
#28369 = ORIENTED_EDGE ( 'NONE', *, *, #25212, .F. ) ;
#28370 = CARTESIAN_POINT ( 'NONE',  ( 81.11132485994279762, 140.7341522555726669, 4.635254915624211769 ) ) ;
#28371 = CARTESIAN_POINT ( 'NONE',  ( 4.903702542908601636, 200.1653181626581102, 62.45113791807857240 ) ) ;
#28372 =( BOUNDED_SURFACE ( )  B_SPLINE_SURFACE ( 3, 2, ( 
 ( #2153, #22926, #28211 ),
 ( #25651, #13537, #32098 ),
 ( #19148, #26645, #8760 ),
 ( #11159, #29381, #29210 ),
 ( #15924, #26481, #8595 ),
 ( #593, #24255, #19322 ) ),
 .UNSPECIFIED., .F., .F., .T. ) 
 B_SPLINE_SURFACE_WITH_KNOTS ( ( 4, 2, 4 ),
 ( 3, 3 ),
 ( 0.03172058138205611361, 0.03571597378202086281, 0.03971136618198560508 ),
 ( 0.000000000000000000, 1.000000000000000000 ),
 .UNSPECIFIED. ) 
 GEOMETRIC_REPRESENTATION_ITEM ( )  RATIONAL_B_SPLINE_SURFACE ( (
 ( 1.000000000000000000, 0.8047780791350982454, 1.000000000000000000),
 ( 1.000000000000000000, 0.8123796029720318224, 1.000000000000000000),
 ( 1.000000000000000000, 0.8190681660673523323, 1.000000000000000000),
 ( 1.000000000000000000, 0.8192342536572917444, 1.000000000000000000),
 ( 1.000000000000000000, 0.8126124427164184150, 1.000000000000000000),
 ( 1.000000000000000000, 0.8047712715942066941, 1.000000000000000000) ) ) 
 REPRESENTATION_ITEM ( '' )  SURFACE ( )  );
#28373 = CARTESIAN_POINT ( 'NONE',  ( 85.02499999726882152, 149.9369285172503510, -15.58253175000000823 ) ) ;
#28374 = CARTESIAN_POINT ( 'NONE',  ( 115.4999999999999858, 54.13214199290997897, 25.91453920131689870 ) ) ;
#28375 = CARTESIAN_POINT ( 'NONE',  ( 6.444103211791042618, 202.2591342207267644, 92.30113791807858092 ) ) ;
#28376 = CARTESIAN_POINT ( 'NONE',  ( -27.50000000000000355, 0.000000000000000000, 0.000000000000000000 ) ) ;
#28377 = FILL_AREA_STYLE ('',( #28029 ) ) ;
#28378 = CARTESIAN_POINT ( 'NONE',  ( 49.10000000000000142, 168.7903194862797420, 4.480746418436729606 ) ) ;
#28379 = CARTESIAN_POINT ( 'NONE',  ( -8.000000000000008882, 206.9523078486584780, 62.49886208192144466 ) ) ;
#28380 = CARTESIAN_POINT ( 'NONE',  ( 88.07499999726879025, 168.2552932293087906, 9.630534252274372875 ) ) ;
#28381 = CARTESIAN_POINT ( 'NONE',  ( 48.22499999726880304, 149.9369285172503510, 15.58253174999999580 ) ) ;
#28382 = CARTESIAN_POINT ( 'NONE',  ( -0.05014649552810635652, 196.4853777576173002, -0.2488620819214343305 ) ) ;
#28383 = CARTESIAN_POINT ( 'NONE',  ( 79.50000000000000000, 155.0000000000000000, 69.99999999999998579 ) ) ;
#28384 = DIRECTION ( 'NONE',  ( 0.000000000000000000, 0.000000000000000000, -1.000000000000000000 ) ) ;
#28385 = CARTESIAN_POINT ( 'NONE',  ( 59.22499999726880304, 160.0630714827496206, -15.58253175000000823 ) ) ;
#28386 = CARTESIAN_POINT ( 'NONE',  ( 68.87499999726881583, 138.6155565068815463, -3.929120461958505118E-15 ) ) ;
#28387 = CARTESIAN_POINT ( 'NONE',  ( -3.662846001190052991, 218.4274158808045740, 67.10113791807857808 ) ) ;
#28388 = CARTESIAN_POINT ( 'NONE',  ( 46.41132485994281609, 167.7597621252805880, 9.270509831248428867 ) ) ;
#28389 = CARTESIAN_POINT ( 'NONE',  ( 9.680171189290831535, 199.9079932115568852, 14.30113791807856849 ) ) ;
#28390 = CARTESIAN_POINT ( 'NONE',  ( 9.984503880673473830, 203.7031108863295401, 89.15113791807857524 ) ) ;
#28391 = CARTESIAN_POINT ( 'NONE',  ( -12.01549611932659722, 210.8513442034533227, 47.64886208192143613 ) ) ;
#28392 = CARTESIAN_POINT ( 'NONE',  ( 10.01549611932659367, 203.7984951890124421, 55.14886208192143613 ) ) ;
#28393 = CARTESIAN_POINT ( 'NONE',  ( -6.499999999999999112, 2.227636940139124722, -0.2900584647821222717 ) ) ;
#28394 = CARTESIAN_POINT ( 'NONE',  ( 9.736236675707914401, 214.0148392665762458, 97.70113791807858661 ) ) ;
#28395 = CARTESIAN_POINT ( 'NONE',  ( -67.50001199999999812, 163.5195614605670755, 14.75313718340012414 ) ) ;
#28396 = CARTESIAN_POINT ( 'NONE',  ( 6.139770520408368348, 198.4640165459539674, 14.45113791807856352 ) ) ;
#28397 = CARTESIAN_POINT ( 'NONE',  ( 3.044812012439969795, 216.5253028482143520, 69.39886208192143613 ) ) ;
#28398 = ORIENTED_EDGE ( 'NONE', *, *, #12655, .F. ) ;
#28399 = CARTESIAN_POINT ( 'NONE',  ( -3.662846001189865142, 195.5725841191952838, 76.89886208192143613 ) ) ;
#28400 = CARTESIAN_POINT ( 'NONE',  ( 8.118202686958039038, 212.8392687619912635, 94.70113791807857240 ) ) ;
#28401 = ORIENTED_EDGE ( 'NONE', *, *, #16174, .F. ) ;
#28402 = CARTESIAN_POINT ( 'NONE',  ( 77.67499999726879878, 168.2552932293087906, -9.630534252274385310 ) ) ;
#28403 = CARTESIAN_POINT ( 'NONE',  ( 6.500168698208244500, 202.3363017425938324, 55.29886208192144892 ) ) ;
#28404 = VERTEX_POINT ( 'NONE', #30695 ) ;
#28405 = CARTESIAN_POINT ( 'NONE',  ( 69.12499999726881583, 155.0000000000000000, -15.58253175000000823 ) ) ;
#28406 = DIRECTION ( 'NONE',  ( 1.000000000000000000, 0.000000000000000000, 0.000000000000000000 ) ) ;
#28407 = CARTESIAN_POINT ( 'NONE',  ( -4.403473400622099909, -6.117907484625868975, -5.839445138371144960E-15 ) ) ;
#28408 = CIRCLE ( 'NONE', #14237, 15.50000000000001066 ) ;
#28409 = CARTESIAN_POINT ( 'NONE',  ( 63.92499999726880588, 164.1591823560292198, 12.60653300113718167 ) ) ;
#28410 = CARTESIAN_POINT ( 'NONE',  ( -7.500000000000000000, -0.7729939684941458111, -7.026407045654831762 ) ) ;
#28411 = CARTESIAN_POINT ( 'NONE',  ( 10.01549611932659545, 203.7984951890123853, 49.14886208192143613 ) ) ;
#28412 = EDGE_LOOP ( 'NONE', ( #9536, #15855, #8209, #14308 ) ) ;
#28413 = FACE_OUTER_BOUND ( 'NONE', #28731, .T. ) ;
#28414 =( NAMED_UNIT ( * ) SI_UNIT ( $, .STERADIAN. ) SOLID_ANGLE_UNIT ( ) );
#28415 = CARTESIAN_POINT ( 'NONE',  ( 105.0134430565187387, 155.0000000000000000, 31.00000000000000000 ) ) ;
#28416 = CARTESIAN_POINT ( 'NONE',  ( 2.426778023690075337, 214.6231898156240447, 39.39886208192144323 ) ) ;
#28417 = CARTESIAN_POINT ( 'NONE',  ( 10.00000000000000711, 206.9523078486586201, 71.00113791807858377 ) ) ;
#28418 = CARTESIAN_POINT ( 'NONE',  ( 34.71132485994281325, 155.0000000000000000, 15.00000000000001243 ) ) ;
#28419 = EDGE_CURVE ( 'NONE', #697, #5483, #17564, .T. ) ;
#28420 = CARTESIAN_POINT ( 'NONE',  ( -9.984503880673473830, 210.2968891136704315, 51.65113791807855392 ) ) ;
#28421 = CONTEXT_DEPENDENT_SHAPE_REPRESENTATION ( #3544, #31835 ) ;
#28422 = PRODUCT_DEFINITION_FORMATION_WITH_SPECIFIED_SOURCE ( 'ANY', '', #1257, .NOT_KNOWN. ) ;
#28423 = CARTESIAN_POINT ( 'NONE',  ( 8.118202686958039038, 212.8392687619912635, 31.70113791807856884 ) ) ;
#28424 = CARTESIAN_POINT ( 'NONE',  ( -7.984503880673488041, 209.6470497212046098, 12.65113791807856636 ) ) ;
#28425 = DIRECTION ( 'NONE',  ( 0.000000000000000000, 0.000000000000000000, 1.000000000000000000 ) ) ;
#28426 = DIRECTION ( 'NONE',  ( 1.000000000000000000, 0.000000000000000000, 0.000000000000000000 ) ) ;
#28427 = CARTESIAN_POINT ( 'NONE',  ( 38.62499999726880873, 138.6155565068815747, -3.929120461958505118E-15 ) ) ;
#28428 = CARTESIAN_POINT ( 'NONE',  ( 9.736236675707914401, 214.0148392665762458, 37.70113791807857240 ) ) ;
#28429 = CARTESIAN_POINT ( 'NONE',  ( 6.837824896291514243, -3.947820044545437224, -6.564402953523717166 ) ) ;
#28430 = CARTESIAN_POINT ( 'NONE',  ( 0.05014649552810505201, 217.5146222423826714, 82.25113791807858377 ) ) ;
#28431 = CARTESIAN_POINT ( 'NONE',  ( -10.01549611932653860, 203.7984951890123000, 63.35113791807857098 ) ) ;
#28432 = DIRECTION ( 'NONE',  ( -0.000000000000000000, -0.000000000000000000, 1.000000000000000000 ) ) ;
#28433 = CARTESIAN_POINT ( 'NONE',  ( -7.375838497908014268, 196.7627149292498530, 20.04886208192143471 ) ) ;
#28434 = CARTESIAN_POINT ( 'NONE',  ( 8.062137200540822946, 212.9164362838583315, 30.69886208192144039 ) ) ;
#28435 = CARTESIAN_POINT ( 'NONE',  ( 74.19999999453763451, 163.5228861582408797, -11.73074641843674470 ) ) ;
#28436 = CARTESIAN_POINT ( 'NONE',  ( 3.662846001190051659, 195.5725841191953691, 65.60113791807857808 ) ) ;
#28437 = CARTESIAN_POINT ( 'NONE',  ( -6.500168698208129925, 202.3363017425936050, 75.20113791807857240 ) ) ;
#28438 = AXIS2_PLACEMENT_3D ( 'NONE', #23857, #8364, #5787 ) ;
#28439 = CARTESIAN_POINT ( 'NONE',  ( 6.220909254589681581, 198.5229672870052582, 37.44886208192143329 ) ) ;
#28440 = B_SPLINE_CURVE_WITH_KNOTS ( 'NONE', 3,
 ( #16032, #26422, #22141, #1698, #25045, #17201, #9030, #32531, #27427, #11931 ),
 .UNSPECIFIED., .F., .F.,
 ( 4, 2, 2, 2, 4 ),
 ( 0.000000000000000000, 0.003060558710793118489, 0.006121117421586236979, 0.009181676132379355468, 0.01224223484317247396 ),
 .UNSPECIFIED. ) ;
#28441 = DIRECTION ( 'NONE',  ( 0.000000000000000000, 0.000000000000000000, -1.000000000000000000 ) ) ;
#28442 = ORIENTED_EDGE ( 'NONE', *, *, #22427, .F. ) ;
#28443 = CARTESIAN_POINT ( 'NONE',  ( -12.01549611932659722, 210.8513442034533227, 47.64886208192143613 ) ) ;
#28444 = ORIENTED_EDGE ( 'NONE', *, *, #20154, .T. ) ;
#28445 = VERTEX_POINT ( 'NONE', #4447 ) ;
#28446 = CYLINDRICAL_SURFACE ( 'NONE', #30361, 15.00000000000001776 ) ;
#28447 = AXIS2_PLACEMENT_3D ( 'NONE', #6115, #29463, #29301 ) ;
#28448 = CARTESIAN_POINT ( 'NONE',  ( 0.000000000000000000, 0.000000000000000000, 0.000000000000000000 ) ) ;
#28449 = ORIENTED_EDGE ( 'NONE', *, *, #17414, .T. ) ;
#28450 = CARTESIAN_POINT ( 'NONE',  ( 8.000000000000008882, 206.9523078486586485, 38.00113791807857666 ) ) ;
#28451 = DIRECTION ( 'NONE',  ( 1.000000000000000000, -0.000000000000000000, -0.000000000000000000 ) ) ;
#28452 = CARTESIAN_POINT ( 'NONE',  ( -10.01549611932659722, 210.2015048109875011, 20.64886208192143613 ) ) ;
#28453 = CARTESIAN_POINT ( 'NONE',  ( 63.77499999726880731, 169.8198683612136222, -4.815267126137197984 ) ) ;
#28454 = ORIENTED_EDGE ( 'NONE', *, *, #4877, .T. ) ;
#28455 = CARTESIAN_POINT ( 'NONE',  ( 3.750000000000004441, -6.495190528383289141, 0.000000000000000000 ) ) ;
#28456 = AXIS2_PLACEMENT_3D ( 'NONE', #27357, #24807, #9469 ) ;
#28457 = CARTESIAN_POINT ( 'NONE',  ( 5.000000000000000000, -2.342598717236903383, 4.057500000000001883 ) ) ;
#28458 = CARTESIAN_POINT ( 'NONE',  ( 7.984503880673422316, 209.6470497212048372, 3.848862081921434530 ) ) ;
#28459 = AXIS2_PLACEMENT_3D ( 'NONE', #25117, #28015, #25291 ) ;
#28460 = CARTESIAN_POINT ( 'NONE',  ( -0.05014649552810635652, 196.4853777576173002, 38.75113791807856956 ) ) ;
#28461 = DIRECTION ( 'NONE',  ( 0.000000000000000000, 0.000000000000000000, -1.000000000000000000 ) ) ;
#28462 = EDGE_CURVE ( 'NONE', #10127, #22384, #30369, .T. ) ;
#28463 = CARTESIAN_POINT ( 'NONE',  ( 10.00000000000000711, 206.9523078486586201, 26.00113791807856956 ) ) ;
#28464 = CARTESIAN_POINT ( 'NONE',  ( 10.01549611932659367, 203.7984951890124421, 103.1488620819214219 ) ) ;
#28465 = SHAPE_DEFINITION_REPRESENTATION ( #6987, #32622 ) ;
#28466 = CARTESIAN_POINT ( 'NONE',  ( 2.426778023690075337, 214.6231898156240447, 81.39886208192143613 ) ) ;
#28467 = CARTESIAN_POINT ( 'NONE',  ( 85.39999999999999147, 159.7113355953771077, 14.49999999999999289 ) ) ;
#28468 = SURFACE_STYLE_USAGE ( .BOTH. , #22 ) ;
#28469 = CARTESIAN_POINT ( 'NONE',  ( -13.75000000000001954, 23.81569860407205752, -18.00000000000000000 ) ) ;
#28470 = CARTESIAN_POINT ( 'NONE',  ( 7.375838497908181246, 196.7627149292499666, 14.45113791807856707 ) ) ;
#28471 = ADVANCED_FACE ( 'NONE', ( #27611 ), #32897, .T. ) ;
#28472 = CARTESIAN_POINT ( 'NONE',  ( 47.78867513459482552, 155.0000000000000000, 15.00000000000001243 ) ) ;
#28473 = CARTESIAN_POINT ( 'NONE',  ( 50.27499999726880731, 160.0630714827496206, 15.58253174999999402 ) ) ;
#28474 = CARTESIAN_POINT ( 'NONE',  ( -0.05014649552810635652, 196.4853777576173002, 59.75113791807857666 ) ) ;
#28475 = LINE ( 'NONE', #23190, #12682 ) ;
#28476 = EDGE_CURVE ( 'NONE', #16783, #33588, #22336, .T. ) ;
#28477 = CIRCLE ( 'NONE', #4508, 0.4000000000000001887 ) ;
#28478 = CARTESIAN_POINT ( 'NONE',  ( 54.30000000000001137, -88.00000000000000000, -30.00000000000000000 ) ) ;
#28479 = CARTESIAN_POINT ( 'NONE',  ( 8.118202686958138514, 201.1607312380088501, 1.298862081921434486 ) ) ;
#28480 = CARTESIAN_POINT ( 'NONE',  ( 53.29999999453763593, 142.6655632788954620, 8.961492836873471646 ) ) ;
#28481 = EDGE_LOOP ( 'NONE', ( #18550, #17749, #13266, #31095 ) ) ;
#28482 = CARTESIAN_POINT ( 'NONE',  ( -7.375838497908182134, 217.2372850707499765, 39.95113791807856529 ) ) ;
#28483 = CARTESIAN_POINT ( 'NONE',  ( 47.31132485994280756, 140.7341522555726669, -4.635254915624220651 ) ) ;
#28484 = CARTESIAN_POINT ( 'NONE',  ( 8.062137200540822946, 212.9164362838583315, 15.69886208192143506 ) ) ;
#28485 = CARTESIAN_POINT ( 'NONE',  ( 5.000000000000000000, 0.000000000000000000, 0.000000000000000000 ) ) ;
#28486 = VERTEX_POINT ( 'NONE', #15008 ) ;
#28487 = CIRCLE ( 'NONE', #23593, 5.000000000000001776 ) ;
#28488 = CARTESIAN_POINT ( 'NONE',  ( 6.220909254589536808, 215.4770327129947702, 7.551137918078564049 ) ) ;
#28489 = CARTESIAN_POINT ( 'NONE',  ( 3.135527875058820690, 216.4958274776887492, 73.40113791807857524 ) ) ;
#28490 = EDGE_CURVE ( 'NONE', #32873, #4795, #4105, .T. ) ;
#28491 = ORIENTED_EDGE ( 'NONE', *, *, #27251, .F. ) ;
#28492 = CARTESIAN_POINT ( 'NONE',  ( 8.015496119326595448, 204.4483345814782638, 31.14886208192143968 ) ) ;
#28493 = CARTESIAN_POINT ( 'NONE',  ( 10.83124253962819949, -25.50084400951697816, -17.88577775926225399 ) ) ;
#28494 = ORIENTED_EDGE ( 'NONE', *, *, #21554, .T. ) ;
#28495 = CARTESIAN_POINT ( 'NONE',  ( 0.05014649552807626948, 215.4116977939061144, 16.25113791807856600 ) ) ;
#28496 = ADVANCED_FACE ( 'NONE', ( #25397 ), #15111, .F. ) ;
#28497 = CARTESIAN_POINT ( 'NONE',  ( -7.375838497908014268, 196.7627149292498530, 98.04886208192144181 ) ) ;
#28498 = CARTESIAN_POINT ( 'NONE',  ( 41.07499999726881157, 141.7447067706911810, -9.630534252274387086 ) ) ;
#28499 = ORIENTED_EDGE ( 'NONE', *, *, #14980, .F. ) ;
#28500 = CARTESIAN_POINT ( 'NONE',  ( 51.12499999726881583, 155.0000000000000000, -15.58253175000000823 ) ) ;
#28501 = CARTESIAN_POINT ( 'NONE',  ( 32.50000000000000000, 155.0000000000000000, -15.00000000000002487 ) ) ;
#28502 = CARTESIAN_POINT ( 'NONE',  ( 8.062137200540920645, 201.0835637161417822, 11.30113791807856671 ) ) ;
#28503 = CIRCLE ( 'NONE', #2383, 2.150000000000004352 ) ;
#28504 = CARTESIAN_POINT ( 'NONE',  ( 9.984503880673420539, 210.2968891136705167, 81.84886208192143897 ) ) ;
#28505 = CARTESIAN_POINT ( 'NONE',  ( 47.17499999726881299, 145.8408176439707802, -12.60653300113719588 ) ) ;
#28506 = CARTESIAN_POINT ( 'NONE',  ( -67.50001200000001234, 153.8873526018536779, -17.00000000000000711 ) ) ;
#28507 = CARTESIAN_POINT ( 'NONE',  ( -0.05014649552810635652, 196.4853777576173002, 11.75113791807856778 ) ) ;
#28508 = PRODUCT ( 'Heavy-Duty Caliper Body Housing', 'Heavy-Duty Caliper Body Housing', '', ( #8831 ) ) ;
#28509 = PLANE ( 'NONE',  #7250 ) ;
#28510 = EDGE_CURVE ( 'NONE', #26168, #31055, #15785, .T. ) ;
#28511 = AXIS2_PLACEMENT_3D ( 'NONE', #23560, #230, #10624 ) ;
#28512 = CARTESIAN_POINT ( 'NONE',  ( 66.90000000000000568, 168.7903194862797420, -4.480746418436745593 ) ) ;
#28513 = CARTESIAN_POINT ( 'NONE',  ( -8.118202686958039038, 201.1607312380087080, 96.20113791807857240 ) ) ;
#28514 = CARTESIAN_POINT ( 'NONE',  ( 0.000000000000000000, 0.000000000000000000, -6.800000000000000711 ) ) ;
#28515 = CARTESIAN_POINT ( 'NONE',  ( 0.05014649552810505201, 217.5146222423826714, 85.25113791807854113 ) ) ;
#28516 = DIRECTION ( 'NONE',  ( 1.000000000000000000, -0.000000000000000000, -0.000000000000000000 ) ) ;
#28517 = AXIS2_PLACEMENT_3D ( 'NONE', #28783, #13270, #12776 ) ;
#28518 = CARTESIAN_POINT ( 'NONE',  ( -1.474514954580286030E-14, 206.9977241638431167, -6.000000000000014211 ) ) ;
#28519 = CARTESIAN_POINT ( 'NONE',  ( 3.662846001189864698, 218.4274158808046593, 93.39886208192143613 ) ) ;
#28520 = CARTESIAN_POINT ( 'NONE',  ( 70.22499999726879594, 149.9369285172503510, 15.58253174999999580 ) ) ;
#28521 = ORIENTED_EDGE ( 'NONE', *, *, #2302, .T. ) ;
#28522 = CARTESIAN_POINT ( 'NONE',  ( -60.74722861894645831, 194.9849492171461804, 1.107464383744043657 ) ) ;
#28523 = CARTESIAN_POINT ( 'NONE',  ( 37.29999999453762882, 142.6655632788954620, 8.961492836873471646 ) ) ;
#28524 = CARTESIAN_POINT ( 'NONE',  ( 9.736236675707914401, 214.0148392665762458, 100.7011379180785866 ) ) ;
#28525 =( BOUNDED_SURFACE ( )  B_SPLINE_SURFACE ( 3, 2, ( 
 ( #15615, #17497, #33350 ),
 ( #15458, #12394, #10361 ),
 ( #25852, #15283, #22788 ),
 ( #33181, #12899, #2513 ),
 ( #20403, #30796, #2346 ),
 ( #23294, #17840, #25677 ),
 ( #12736, #10187, #20570 ),
 ( #29235, #10683, #3505 ) ),
 .UNSPECIFIED., .F., .F., .T. ) 
 B_SPLINE_SURFACE_WITH_KNOTS ( ( 4, 2, 2, 4 ),
 ( 3, 3 ),
 ( 0.03170918191602133812, 0.03570420671717101924, 0.03770171911774586326, 0.03969923151832070729 ),
 ( 0.000000000000000000, 1.000000000000000000 ),
 .UNSPECIFIED. ) 
 GEOMETRIC_REPRESENTATION_ITEM ( )  RATIONAL_B_SPLINE_SURFACE ( (
 ( 1.000000000000000000, 0.8047781070930550840, 1.000000000000000000),
 ( 1.000000000000000000, 0.8123787894255611874, 1.000000000000000000),
 ( 1.000000000000000000, 0.8190667557154468481, 1.000000000000000000),
 ( 1.000000000000000000, 0.8191933945820784047, 1.000000000000000000),
 ( 1.000000000000000000, 0.8176087340369108114, 1.000000000000000000),
 ( 1.000000000000000000, 0.8122956952719621038, 1.000000000000000000),
 ( 1.000000000000000000, 0.8086308540103167575, 1.000000000000000000),
 ( 1.000000000000000000, 0.8047712493762134711, 1.000000000000000000) ) ) 
 REPRESENTATION_ITEM ( '' )  SURFACE ( )  );
#28526 = EDGE_CURVE ( 'NONE', #31333, #20312, #7159, .T. ) ;
#28527 = DIRECTION ( 'NONE',  ( -1.000000000000000000, 0.000000000000000000, 0.000000000000000000 ) ) ;
#28528 = ORIENTED_EDGE ( 'NONE', *, *, #1607, .T. ) ;
#28529 = CARTESIAN_POINT ( 'NONE',  ( -8.062137200540822946, 201.0835637161416400, 89.19886208192144750 ) ) ;
#28530 = CARTESIAN_POINT ( 'NONE',  ( -12.01549611932659722, 210.8513442034533227, 26.64886208192143968 ) ) ;
#28531 = CARTESIAN_POINT ( 'NONE',  ( 4.506125120515185323, -29.15265225409788030, -1.090893241169181183 ) ) ;
#28532 = CARTESIAN_POINT ( 'NONE',  ( 10.00000000000000711, 206.9523078486586201, 38.00113791807857666 ) ) ;
#28533 = ORIENTED_EDGE ( 'NONE', *, *, #17444, .F. ) ;
#28534 = EDGE_CURVE ( 'NONE', #10769, #7638, #2907, .T. ) ;
#28535 = CARTESIAN_POINT ( 'NONE',  ( 2.426778023690075337, 214.6231898156240447, 3.398862081921434797 ) ) ;
#28536 = CARTESIAN_POINT ( 'NONE',  ( -52.50000000000002132, 0.000000000000000000, 270.4495957273638282 ) ) ;
#28537 =( GEOMETRIC_REPRESENTATION_CONTEXT ( 3 ) GLOBAL_UNCERTAINTY_ASSIGNED_CONTEXT ( ( #10685 ) ) GLOBAL_UNIT_ASSIGNED_CONTEXT ( ( #29632, #26558, #31840 ) ) REPRESENTATION_CONTEXT ( 'NONE', 'WORKASPACE' ) );
#28538 = ORIENTED_EDGE ( 'NONE', *, *, #9725, .F. ) ;
#28539 = CARTESIAN_POINT ( 'NONE',  ( 2.426778023690075337, 214.6231898156240447, 90.39886208192143613 ) ) ;
#28540 = AXIS2_PLACEMENT_3D ( 'NONE', #27548, #25336, #7118 ) ;
#28541 = ADVANCED_FACE ( 'NONE', ( #15180, #5128 ), #18076, .F. ) ;
#28542 = ORIENTED_EDGE ( 'NONE', *, *, #17467, .T. ) ;
#28543 = CARTESIAN_POINT ( 'NONE',  ( -8.000000000000008882, 207.0476921513413515, 30.50113791807856600 ) ) ;
#28544 = CARTESIAN_POINT ( 'NONE',  ( 0.000000000000000000, 0.000000000000000000, -18.00000000000000000 ) ) ;
#28545 = EDGE_LOOP ( 'NONE', ( #941, #7665, #20768, #1066 ) ) ;
#28546 = DIRECTION ( 'NONE',  ( 1.000000000000000000, -0.000000000000000000, -0.000000000000000000 ) ) ;
#28547 = CARTESIAN_POINT ( 'NONE',  ( 81.32499999726880446, 164.1591823560292198, -12.60653300113719766 ) ) ;
#28548 = LINE ( 'NONE', #12864, #6151 ) ;
#28549 = CARTESIAN_POINT ( 'NONE',  ( -8.000000000000008882, 207.0476921513413515, 90.50113791807858377 ) ) ;
#28550 = DIRECTION ( 'NONE',  ( 0.000000000000000000, 0.000000000000000000, -1.000000000000000000 ) ) ;
#28551 = CARTESIAN_POINT ( 'NONE',  ( 0.000000000000000000, 0.000000000000000000, 0.000000000000000000 ) ) ;
#28552 = CARTESIAN_POINT ( 'NONE',  ( 50.40000000000000568, 150.2886644046228639, -14.50000000000000888 ) ) ;
#28553 = CARTESIAN_POINT ( 'NONE',  ( 2.426778023690075337, 214.6231898156240447, 60.39886208192144323 ) ) ;
#28554 = CARTESIAN_POINT ( 'NONE',  ( 27.50000000000000355, -13.28298644054429545, -1.741296657551683280 ) ) ;
#28555 = CARTESIAN_POINT ( 'NONE',  ( 53.02499999726881441, 149.9369285172503510, -15.58253175000000823 ) ) ;
#28556 = CARTESIAN_POINT ( 'NONE',  ( 0.05014649552810506589, 217.5146222423826714, 4.251137918078566003 ) ) ;
#28557 = CARTESIAN_POINT ( 'NONE',  ( 10.00000000000000178, 0.000000000000000000, 0.000000000000000000 ) ) ;
#28558 = CARTESIAN_POINT ( 'NONE',  ( 56.42499999726881299, 141.7447067706911810, 9.630534252274376428 ) ) ;
#28559 = CARTESIAN_POINT ( 'NONE',  ( 68.27499999726879309, 160.0630714827496206, 15.58253174999999402 ) ) ;
#28560 = CARTESIAN_POINT ( 'NONE',  ( -12.00000000000000711, 207.0476921513413515, 63.50113791807856956 ) ) ;
#28561 = CARTESIAN_POINT ( 'NONE',  ( 41.51132485994280330, 146.1832212156128890, -12.13525491562423042 ) ) ;
#28562 = CARTESIAN_POINT ( 'NONE',  ( -12.00000000000000711, 207.0476921513413515, 6.501137918078566891 ) ) ;
#28563 = ADVANCED_FACE ( 'NONE', ( #20635, #23362 ), #15516, .T. ) ;
#28564 = CARTESIAN_POINT ( 'NONE',  ( -10.00000000000000711, 207.0476921513413515, 84.50113791807856956 ) ) ;
#28565 = CARTESIAN_POINT ( 'NONE',  ( -12.01549611932659722, 210.8513442034533227, 50.64886208192143613 ) ) ;
#28566 = CARTESIAN_POINT ( 'NONE',  ( -9.984503880673420539, 203.7031108863293980, 59.34886208192143187 ) ) ;
#28567 = CARTESIAN_POINT ( 'NONE',  ( 3.753561863808689836, 218.3979405102790565, 100.4011379180785895 ) ) ;
#28568 = CARTESIAN_POINT ( 'NONE',  ( -3.135527875058821579, 197.5041725223112223, 8.901137918078566358 ) ) ;
#28569 = EDGE_CURVE ( 'NONE', #2210, #8132, #12417, .T. ) ;
#28570 = CARTESIAN_POINT ( 'NONE',  ( -8.118202686958138514, 212.8392687619910930, 77.79886208192144181 ) ) ;
#28571 = ORIENTED_EDGE ( 'NONE', *, *, #21851, .T. ) ;
#28572 = CARTESIAN_POINT ( 'NONE',  ( 3.753561863808876797, 195.6020594897209719, 79.59886208192143897 ) ) ;
#28573 = CARTESIAN_POINT ( 'NONE',  ( -6.139770520408369237, 215.5359834540460042, 96.95113791807857240 ) ) ;
#28574 = ORIENTED_EDGE ( 'NONE', *, *, #18949, .T. ) ;
#28575 = CARTESIAN_POINT ( 'NONE',  ( 78.97499999726881015, 140.1801316387863778, -4.815267126137194431 ) ) ;
#28576 = CARTESIAN_POINT ( 'NONE',  ( 4.984841277089891776, 200.2242689037093726, 55.44886208192143329 ) ) ;
#28577 = ORIENTED_EDGE ( 'NONE', *, *, #3681, .T. ) ;
#28578 = CARTESIAN_POINT ( 'NONE',  ( 70.72499999726881015, 140.1801316387863778, -4.815267126137194431 ) ) ;
#28579 = FACE_OUTER_BOUND ( 'NONE', #33685, .T. ) ;
#28580 = CARTESIAN_POINT ( 'NONE',  ( -56.01598787314604522, 194.9989914758641305, 0.3258944654411097264 ) ) ;
#28581 = CARTESIAN_POINT ( 'NONE',  ( 60.52499999726881441, 140.1801316387863778, 4.815267126137185549 ) ) ;
#28582 = DIRECTION ( 'NONE',  ( 0.000000000000000000, 0.4999999999999990563, -0.8660254037844391517 ) ) ;
#28583 = CARTESIAN_POINT ( 'NONE',  ( -8.118202686958138514, 212.8392687619910930, 50.79886208192143471 ) ) ;
#28584 = ORIENTED_EDGE ( 'NONE', *, *, #15586, .T. ) ;
#28585 = DIRECTION ( 'NONE',  ( 0.000000000000000000, 0.8660254037844379305, -0.5000000000000013323 ) ) ;
#28586 = SURFACE_SIDE_STYLE ('',( #795 ) ) ;
#28587 = DIRECTION ( 'NONE',  ( 1.000000000000000000, 0.000000000000000000, 0.000000000000000000 ) ) ;
#28588 = CARTESIAN_POINT ( 'NONE',  ( 8.015496119326595448, 204.4483345814782638, 34.14886208192144323 ) ) ;
#28589 = CARTESIAN_POINT ( 'NONE',  ( 9.984503880673470277, 203.7031108863295401, 74.15113791807854682 ) ) ;
#28590 = CARTESIAN_POINT ( 'NONE',  ( -54.30000000000001847, -88.00000000000000000, -20.00000000000000000 ) ) ;
#28591 = CARTESIAN_POINT ( 'NONE',  ( -8.062137200540920645, 212.9164362838581894, 51.80113791807857382 ) ) ;
#28592 = ITEM_DEFINED_TRANSFORMATION ( 'NONE', 'NONE', #31698,  #2404 ) ;
#28593 = CARTESIAN_POINT ( 'NONE',  ( 6.139770520408368348, 198.4640165459539674, 23.45113791807856884 ) ) ;
#28594 = CARTESIAN_POINT ( 'NONE',  ( -2.426778023690262742, 214.6231898156240163, 16.10113791807856742 ) ) ;
#28595 = DIRECTION ( 'NONE',  ( -1.000000000000000000, 0.000000000000000000, 0.000000000000000000 ) ) ;
#28596 = CARTESIAN_POINT ( 'NONE',  ( 36.32499999726881157, 145.8408176439707802, 12.60653300113718345 ) ) ;
#28597 = CARTESIAN_POINT ( 'NONE',  ( 12.00000000000000711, 206.9523078486586485, 35.00113791807857666 ) ) ;
#28598 = CARTESIAN_POINT ( 'NONE',  ( 4.555432764205793461, -5.242992371775935467, -6.208169345099792125 ) ) ;
#28599 = CARTESIAN_POINT ( 'NONE',  ( -9.984503880673473830, 210.2968891136704315, 87.65113791807854682 ) ) ;
#28600 = CARTESIAN_POINT ( 'NONE',  ( -10.00000000000000711, 207.0476921513413515, 57.50113791807856956 ) ) ;
#28601 = CARTESIAN_POINT ( 'NONE',  ( 99.99999999999998579, 5.616230220889761452E-16, -4.171999999999999709 ) ) ;
#28602 = CARTESIAN_POINT ( 'NONE',  ( -12.00000000000000711, 206.9523078486584780, 26.49886208192143400 ) ) ;
#28603 = CARTESIAN_POINT ( 'NONE',  ( -6.220909254589682469, 215.4770327129947134, 32.94886208192144039 ) ) ;
#28604 = CARTESIAN_POINT ( 'NONE',  ( 77.99999999453763166, 155.0000000000000000, -14.50000000000000711 ) ) ;
#28605 = CARTESIAN_POINT ( 'NONE',  ( -11.98450388067348804, 210.9467285061362247, 66.65113791807856103 ) ) ;
#28606 = CARTESIAN_POINT ( 'NONE',  ( 6.500168698208129925, 211.6636982574063381, 88.70113791807857240 ) ) ;
#28607 = CARTESIAN_POINT ( 'NONE',  ( -3.044812012439970683, 197.4746971517856196, 43.89886208192142902 ) ) ;
#28608 = LINE ( 'NONE', #2549, #33572 ) ;
#28609 = EDGE_CURVE ( 'NONE', #12292, #23334, #6754, .T. ) ;
#28610 = VERTEX_POINT ( 'NONE', #31195 ) ;
#28611 = CARTESIAN_POINT ( 'NONE',  ( 7.375838497908012492, 217.2372850707501186, 48.54886208192142050 ) ) ;
#28612 = ORIENTED_EDGE ( 'NONE', *, *, #858, .F. ) ;
#28613 = ORIENTED_EDGE ( 'NONE', *, *, #15135, .T. ) ;
#28614 = CARTESIAN_POINT ( 'NONE',  ( 93.60208470531338776, 155.0000000000000000, 0.000000000000000000 ) ) ;
#28615 = CARTESIAN_POINT ( 'NONE',  ( -7.914984360234579519, 3.818534719232089980, -7.907701344400639876 ) ) ;
#28616 = ORIENTED_EDGE ( 'NONE', *, *, #21858, .F. ) ;
#28617 = CARTESIAN_POINT ( 'NONE',  ( -8.000000000000008882, 207.0476921513413515, 45.50113791807857666 ) ) ;
#28618 = CARTESIAN_POINT ( 'NONE',  ( 82.61132485994282604, 159.8737954434934920, 15.00000000000010836 ) ) ;
#28619 = CARTESIAN_POINT ( 'NONE',  ( -8.062137200540822946, 201.0835637161416400, 20.19886208192143684 ) ) ;
#28620 = CARTESIAN_POINT ( 'NONE',  ( 63.47499999726881015, 160.0630714827496206, -15.58253175000000823 ) ) ;
#28621 = ORIENTED_EDGE ( 'NONE', *, *, #22607, .F. ) ;
#28622 = CARTESIAN_POINT ( 'NONE',  ( -64.50000000000000000, 0.000000000000000000, -20.00000000000000000 ) ) ;
#28623 = CARTESIAN_POINT ( 'NONE',  ( 0.000000000000000000, 0.000000000000000000, 0.000000000000000000 ) ) ;
#28624 = CARTESIAN_POINT ( 'NONE',  ( 2.517493886309087436, 199.4062855549015865, 7.598862081921434530 ) ) ;
#28625 = CARTESIAN_POINT ( 'NONE',  ( 0.05014649552810505201, 217.5146222423826714, 43.25113791807856956 ) ) ;
#28626 = CARTESIAN_POINT ( 'NONE',  ( 87.40513633176574615, 142.1470333418077132, -8.983655774715980868 ) ) ;
#28627 = CARTESIAN_POINT ( 'NONE',  ( 6.139770520408368348, 198.4640165459539674, 29.45113791807856529 ) ) ;
#28628 = CARTESIAN_POINT ( 'NONE',  ( -8.062137200540822946, 201.0835637161416400, 101.1988620819214475 ) ) ;
#28629 = APPLICATION_PROTOCOL_DEFINITION ( 'draft international standard', 'automotive_design', 1998, #18785 ) ;
#28630 = CARTESIAN_POINT ( 'NONE',  ( 8.000000000000008882, 207.0476921513415220, 90.99886208192144466 ) ) ;
#28631 = CARTESIAN_POINT ( 'NONE',  ( 84.39999999999999147, 150.2886644046228639, -14.50000000000000888 ) ) ;
#28632 = CARTESIAN_POINT ( 'NONE',  ( -3.750000000000004885, 6.495190528383289141, 0.000000000000000000 ) ) ;
#28633 = DIRECTION ( 'NONE',  ( 0.8191520442889912434, 1.003171929053524007E-16, -0.5735764363510469366 ) ) ;
#28634 = CARTESIAN_POINT ( 'NONE',  ( 12.00000000000000711, 206.9523078486586485, 14.00113791807856600 ) ) ;
#28635 = CARTESIAN_POINT ( 'NONE',  ( 64.38867513459483405, 140.7341522555726669, -4.635254915624220651 ) ) ;
#28636 = CARTESIAN_POINT ( 'NONE',  ( 60.27499999726880020, 160.0630714827496206, 15.58253174999999402 ) ) ;
#28637 = CARTESIAN_POINT ( 'NONE',  ( -3.135527875058821579, 197.5041725223112223, 56.90113791807857524 ) ) ;
#28638 = FACE_OUTER_BOUND ( 'NONE', #15862, .T. ) ;
#28639 = DIRECTION ( 'NONE',  ( -0.8660254037844382635, 0.5000000000000005551, 0.000000000000000000 ) ) ;
#28640 = DIRECTION ( 'NONE',  ( -0.000000000000000000, -0.000000000000000000, -1.000000000000000000 ) ) ;
#28641 = CARTESIAN_POINT ( 'NONE',  ( 57.79999999453762882, 146.4771138417591203, -11.73074641843674470 ) ) ;
#28642 = VERTEX_POINT ( 'NONE', #25573 ) ;
#28643 = CARTESIAN_POINT ( 'NONE',  ( 12.01549611932652972, 210.8513442034534933, 34.85113791807856387 ) ) ;
#28644 = DIRECTION ( 'NONE',  ( 0.000000000000000000, 0.000000000000000000, -1.000000000000000000 ) ) ;
#28645 = CARTESIAN_POINT ( 'NONE',  ( 8.118202686958138514, 201.1607312380088501, 10.29886208192143471 ) ) ;
#28646 = DIRECTION ( 'NONE',  ( 1.000000000000000000, 0.000000000000000000, 0.000000000000000000 ) ) ;
#28647 = ORIENTED_EDGE ( 'NONE', *, *, #1818, .F. ) ;
#28648 = CARTESIAN_POINT ( 'NONE',  ( -10.00000000000000711, 207.0476921513413515, 69.50113791807856956 ) ) ;
#28649 = EDGE_LOOP ( 'NONE', ( #25412, #31815, #15072, #23728 ) ) ;
#28650 = CARTESIAN_POINT ( 'NONE',  ( -4.984841277089891776, 213.7757310962905990, 35.94886208192144039 ) ) ;
#28651 = ADVANCED_FACE ( 'NONE', ( #28805 ), #24378, .T. ) ;
#28652 = CARTESIAN_POINT ( 'NONE',  ( 79.98867513459481415, 146.1832212156128890, 12.13525491562421976 ) ) ;
#28653 = ORIENTED_EDGE ( 'NONE', *, *, #10168, .F. ) ;
#28654 = CARTESIAN_POINT ( 'NONE',  ( -4.903702542908602524, 213.8346818373418898, 12.95113791807856707 ) ) ;
#28655 = VECTOR ( 'NONE', #6000, 1000.000000000000000 ) ;
#28656 = CARTESIAN_POINT ( 'NONE',  ( 3.662846001189864698, 218.4274158808046593, 99.39886208192146455 ) ) ;
#28657 = CARTESIAN_POINT ( 'NONE',  ( 42.97499999726881015, 140.1801316387863778, -4.815267126137194431 ) ) ;
#28658 = ORIENTED_EDGE ( 'NONE', *, *, #8864, .F. ) ;
#28659 = CARTESIAN_POINT ( 'NONE',  ( 52.62499999726880162, 138.6155565068815463, -3.929120461958505118E-15 ) ) ;
#28660 = DIRECTION ( 'NONE',  ( 0.000000000000000000, 0.000000000000000000, -1.000000000000000000 ) ) ;
#28661 = CARTESIAN_POINT ( 'NONE',  ( -3.135527875058821579, 197.5041725223112223, 8.901137918078566358 ) ) ;
#28662 = CARTESIAN_POINT ( 'NONE',  ( 3.135527875058981895, 197.5041725223112792, 76.59886208192142476 ) ) ;
#28663 = CARTESIAN_POINT ( 'NONE',  ( 53.07499999726880446, 141.7447067706911810, -9.630534252274385310 ) ) ;
#28664 = CARTESIAN_POINT ( 'NONE',  ( -67.50001199999998391, 137.9999999999999432, 1.112647398146386912 ) ) ;
#28665 = CARTESIAN_POINT ( 'NONE',  ( 8.118202686958039038, 212.8392687619912635, 16.70113791807856529 ) ) ;
#28666 = CARTESIAN_POINT ( 'NONE',  ( -58.50000000000002132, 209.9999999999999716, 0.000000000000000000 ) ) ;
#28667 = AXIS2_PLACEMENT_3D ( 'NONE', #30549, #7211, #27989 ) ;
#28668 = CARTESIAN_POINT ( 'NONE',  ( 66.40000000000000568, 150.2886644046228639, -14.50000000000000888 ) ) ;
#28669 = CARTESIAN_POINT ( 'NONE',  ( -10.01549611932653860, 203.7984951890123284, 96.35113791807853545 ) ) ;
#28670 = CARTESIAN_POINT ( 'NONE',  ( 38.08867513459482268, 142.2402378747194405, 9.270509831248432420 ) ) ;
#28671 = CARTESIAN_POINT ( 'NONE',  ( -8.062137200540920645, 212.9164362838581894, 87.80113791807856671 ) ) ;
#28672 = CYLINDRICAL_SURFACE ( 'NONE', #23264, 2.149999999999984812 ) ;
#28673 = CARTESIAN_POINT ( 'NONE',  ( 39.07499999726881157, 141.7447067706911810, -9.630534252274385310 ) ) ;
#28674 = CARTESIAN_POINT ( 'NONE',  ( 9.680171189290716072, 214.0920067884432854, 99.69886208192144750 ) ) ;
#28675 = CARTESIAN_POINT ( 'NONE',  ( 71.12499999726881583, 155.0000000000000000, -15.58253175000000823 ) ) ;
#28676 = ORIENTED_EDGE ( 'NONE', *, *, #7885, .F. ) ;
#28677 = CARTESIAN_POINT ( 'NONE',  ( -59.60884549136632415, 194.9369081818307166, 2.246623501397673639 ) ) ;
#28678 = CARTESIAN_POINT ( 'NONE',  ( 86.17499999726881299, 164.1591823560292198, 12.60653300113718167 ) ) ;
#28679 = CARTESIAN_POINT ( 'NONE',  ( 11.98450388067348271, 203.0532714938637753, 101.1511379180785895 ) ) ;
#28680 = AXIS2_PLACEMENT_3D ( 'NONE', #1105, #13700, #18661 ) ;
#28681 = ADVANCED_FACE ( 'NONE', ( #12621 ), #4961, .F. ) ;
#28682 = CARTESIAN_POINT ( 'NONE',  ( 0.1999999999999987899, 0.000000000000000000, 0.000000000000000000 ) ) ;
#28683 = CONICAL_SURFACE ( 'NONE', #13979, 37.00000000000000711, 0.7853981633974482790 ) ;
#28684 = ORIENTED_EDGE ( 'NONE', *, *, #7715, .F. ) ;
#28685 = CIRCLE ( 'NONE', #23237, 13.00000000000001776 ) ;
#28686 = CARTESIAN_POINT ( 'NONE',  ( 9.984503880673420539, 210.2968891136705736, 87.84886208192142476 ) ) ;
#28687 = CARTESIAN_POINT ( 'NONE',  ( -12.00000000000000711, 206.9523078486584780, 23.49886208192144110 ) ) ;
#28688 = DIRECTION ( 'NONE',  ( 0.000000000000000000, 0.000000000000000000, 1.000000000000000000 ) ) ;
#28689 = CARTESIAN_POINT ( 'NONE',  ( 0.05014649552810505201, 217.5146222423826714, 46.25113791807855534 ) ) ;
#28690 = ORIENTED_EDGE ( 'NONE', *, *, #29071, .F. ) ;
#28691 = CARTESIAN_POINT ( 'NONE',  ( -4.903702542908436435, 200.1653181626580249, 8.048862081921434708 ) ) ;
#28692 = ADVANCED_FACE ( 'NONE', ( #23521 ), #12392, .T. ) ;
#28693 = CIRCLE ( 'NONE', #6353, 16.00000000000000000 ) ;
#28694 = CARTESIAN_POINT ( 'NONE',  ( 73.81132485994281467, 159.8737954434934920, -15.00000000000012434 ) ) ;
#28695 = EDGE_LOOP ( 'NONE', ( #30240, #18013, #6645, #17404 ) ) ;
#28696 = CARTESIAN_POINT ( 'NONE',  ( -7.984503880673422316, 204.3529502787951628, 92.34886208192143897 ) ) ;
#28697 = VERTEX_POINT ( 'NONE', #8027 ) ;
#28698 = CARTESIAN_POINT ( 'NONE',  ( -2.426778023690262742, 214.6231898156240163, 28.10113791807856742 ) ) ;
#28699 = CARTESIAN_POINT ( 'NONE',  ( 117.5000000000000000, 182.4348187808683690, 102.3881375866409513 ) ) ;
#28700 = ORIENTED_EDGE ( 'NONE', *, *, #31044, .T. ) ;
#28701 = ADVANCED_FACE ( 'NONE', ( #15847 ), #7528, .T. ) ;
#28702 = CARTESIAN_POINT ( 'NONE',  ( 35.67499999726880588, 168.2552932293087906, -9.630534252274385310 ) ) ;
#28703 = FACE_OUTER_BOUND ( 'NONE', #28002, .T. ) ;
#28704 = CARTESIAN_POINT ( 'NONE',  ( -2.426778023690262742, 214.6231898156240163, 88.10113791807857808 ) ) ;
#28705 = LINE ( 'NONE', #30765, #2673 ) ;
#28706 = VECTOR ( 'NONE', #6734, 1000.000000000000000 ) ;
#28707 = MECHANICAL_DESIGN_GEOMETRIC_PRESENTATION_REPRESENTATION (  '', ( #30884 ), #11294 ) ;
#28708 = CARTESIAN_POINT ( 'NONE',  ( 46.79999999999999716, 167.3344367211045096, -8.961492836873482304 ) ) ;
#28709 = CARTESIAN_POINT ( 'NONE',  ( -2.426778023690076225, 199.3768101843759553, 67.89886208192143613 ) ) ;
#28710 = PLANE ( 'NONE',  #11302 ) ;
#28711 = ADVANCED_FACE ( 'NONE', ( #28963 ), #24570, .F. ) ;
#28712 =( BOUNDED_CURVE ( )  B_SPLINE_CURVE ( 2, ( #23824, #3210, #13598, #23992, #655, #11056, #21437, #18879, #29273, #5924, #16318 ),
 .UNSPECIFIED., .F., .T. ) 
 B_SPLINE_CURVE_WITH_KNOTS ( ( 3, 2, 2, 2, 2, 3 ),
 ( 0.3392857142857141906, 0.3428571428571427493, 0.3464285714285713080, 0.3499999999999998668, 0.3535714285714284810, 0.3571428571428570398 ),
 .UNSPECIFIED. ) 
 CURVE ( )  GEOMETRIC_REPRESENTATION_ITEM ( )  RATIONAL_B_SPLINE_CURVE ( ( 1.000000000000001554, 0.9510565162951518658, 1.000000000000000000, 0.9510565162951534202, 1.000000000000000000, 0.9510565162951534202, 1.000000000000000000, 0.9510565162951534202, 1.000000000000000000, 0.9510565162951549745, 0.9999999999999984457 ) ) 
 REPRESENTATION_ITEM ( '' )  );
#28713 = EDGE_CURVE ( 'NONE', #32991, #17505, #16171, .T. ) ;
#28714 = AXIS2_PLACEMENT_3D ( 'NONE', #13169, #23563, #15886 ) ;
#28715 = CARTESIAN_POINT ( 'NONE',  ( 48.52499999726880731, 140.1801316387863778, 4.815267126137185549 ) ) ;
#28716 = CARTESIAN_POINT ( 'NONE',  ( 9.984503880673473830, 203.7031108863295401, 5.151137918078566358 ) ) ;
#28717 = DIRECTION ( 'NONE',  ( 0.9366133782696128840, 0.000000000000000000, 0.3503646381220332229 ) ) ;
#28718 = CARTESIAN_POINT ( 'NONE',  ( 66.32499999726881867, 145.8408176439707802, 12.60653300113718345 ) ) ;
#28719 = CARTESIAN_POINT ( 'NONE',  ( 69.17499999726881299, 145.8408176439707802, -12.60653300113719588 ) ) ;
#28720 = CARTESIAN_POINT ( 'NONE',  ( 3.753561863808689836, 218.3979405102790565, 67.40113791807856103 ) ) ;
#28721 = FACE_BOUND ( 'NONE', #20261, .T. ) ;
#28722 = CARTESIAN_POINT ( 'NONE',  ( 7.375838497908181246, 196.7627149292499666, 11.45113791807856529 ) ) ;
#28723 = CARTESIAN_POINT ( 'NONE',  ( 9.984503880673473830, 203.7031108863295401, 92.15113791807854682 ) ) ;
#28724 = DIRECTION ( 'NONE',  ( 1.000000000000000000, -0.000000000000000000, -0.000000000000000000 ) ) ;
#28725 = CARTESIAN_POINT ( 'NONE',  ( 11.98450388067341876, 210.9467285061363953, 48.84886208192143897 ) ) ;
#28726 = CARTESIAN_POINT ( 'NONE',  ( -6.139770520408224463, 198.4640165459539105, 62.04886208192143471 ) ) ;
#28727 = CARTESIAN_POINT ( 'NONE',  ( 9.680171189290831535, 199.9079932115568852, 101.3011379180785951 ) ) ;
#28728 = CARTESIAN_POINT ( 'NONE',  ( -67.50001199999998391, 170.2801603273571800, -7.533570508255905018 ) ) ;
#28729 = CARTESIAN_POINT ( 'NONE',  ( -9.984503880673473830, 210.2968891136704315, 15.65113791807856813 ) ) ;
#28730 = CARTESIAN_POINT ( 'NONE',  ( -6.139770520408224463, 198.4640165459539389, 80.04886208192139918 ) ) ;
#28731 = EDGE_LOOP ( 'NONE', ( #20522, #23701, #30455, #30449 ) ) ;
#28732 = CARTESIAN_POINT ( 'NONE',  ( 7.375838497908012492, 217.2372850707501186, 81.54886208192144181 ) ) ;
#28733 = CIRCLE ( 'NONE', #28177, 0.2000000000000000944 ) ;
#28734 = CARTESIAN_POINT ( 'NONE',  ( 8.062137200540920645, 201.0835637161417822, 101.3011379180785809 ) ) ;
#28735 = VERTEX_POINT ( 'NONE', #26732 ) ;
#28736 = CARTESIAN_POINT ( 'NONE',  ( 0.000000000000000000, 0.000000000000000000, 2.066666666667000385 ) ) ;
#28737 = CARTESIAN_POINT ( 'NONE',  ( -6.500168698208244500, 211.6636982574061676, 65.79886208192144181 ) ) ;
#28738 = ORIENTED_EDGE ( 'NONE', *, *, #13724, .T. ) ;
#28739 = CARTESIAN_POINT ( 'NONE',  ( 75.72499999726881015, 169.8198683612136222, 4.815267126137181997 ) ) ;
#28740 = DIRECTION ( 'NONE',  ( 0.1045284632676459352, 0.000000000000000000, -0.9945218953682740670 ) ) ;
#28741 = CARTESIAN_POINT ( 'NONE',  ( 127.5000000000000000, 231.4735983853260279, 73.43303922622204993 ) ) ;
#28742 = UNCERTAINTY_MEASURE_WITH_UNIT (LENGTH_MEASURE( 1.000000000000000082E-05 ), #21117, 'distance_accuracy_value', 'NONE');
#28743 = CARTESIAN_POINT ( 'NONE',  ( 64.12499999726881583, 155.0000000000000000, 15.58253174999999402 ) ) ;
#28744 = EDGE_CURVE ( 'NONE', #12431, #7668, #29635, .T. ) ;
#28745 = CARTESIAN_POINT ( 'NONE',  ( -7.897827455343210623, -1.533134349199909208, -7.633632140068262295 ) ) ;
#28746 = EDGE_CURVE ( 'NONE', #24999, #26131, #22757, .T. ) ;
#28747 = CARTESIAN_POINT ( 'NONE',  ( 10.00000000000000711, 207.0476921513415220, 51.99886208192143755 ) ) ;
#28748 = VERTEX_POINT ( 'NONE', #24183 ) ;
#28749 = FACE_OUTER_BOUND ( 'NONE', #4378, .T. ) ;
#28750 = DIRECTION ( 'NONE',  ( -1.000000000000000000, -0.000000000000000000, -0.000000000000000000 ) ) ;
#28751 = CARTESIAN_POINT ( 'NONE',  ( 4.984841277089891776, 200.2242689037093726, 31.44886208192143684 ) ) ;
#28752 = CARTESIAN_POINT ( 'NONE',  ( -10.01549611932653860, 203.7984951890123284, 84.35113791807856387 ) ) ;
#28753 = FACE_BOUND ( 'NONE', #10636, .T. ) ;
#28754 = EDGE_CURVE ( 'NONE', #8324, #6680, #26534, .T. ) ;
#28755 = CARTESIAN_POINT ( 'NONE',  ( -9.984503880673473830, 210.2968891136704315, 57.65113791807858235 ) ) ;
#28756 = CIRCLE ( 'NONE', #4253, 31.00000000000000000 ) ;
#28757 = CARTESIAN_POINT ( 'NONE',  ( 8.062137200540920645, 201.0835637161417822, 32.30113791807857382 ) ) ;
#28758 = CARTESIAN_POINT ( 'NONE',  ( -6.500168698208129925, 202.3363017425936050, 12.20113791807856707 ) ) ;
#28759 = CARTESIAN_POINT ( 'NONE',  ( 45.98867513459482126, 146.1832212156128890, 12.13525491562421976 ) ) ;
#28760 = CARTESIAN_POINT ( 'NONE',  ( 115.4999999999999858, 207.9999999999998010, -91.79869280115066488 ) ) ;
#28761 = CARTESIAN_POINT ( 'NONE',  ( 37.22499999726881015, 160.0630714827496206, -15.58253175000000823 ) ) ;
#28762 = CARTESIAN_POINT ( 'NONE',  ( 11.98450388067348271, 203.0532714938637753, 35.15113791807856103 ) ) ;
#28763 = DIRECTION ( 'NONE',  ( -1.000000000000000000, 0.000000000000000000, -0.000000000000000000 ) ) ;
#28764 = EDGE_CURVE ( 'NONE', #17200, #20297, #29296, .T. ) ;
#28765 = CARTESIAN_POINT ( 'NONE',  ( 3.044812012440130555, 197.4746971517856764, 83.60113791807857808 ) ) ;
#28766 = CARTESIAN_POINT ( 'NONE',  ( 0.05014649552810506589, 217.5146222423826714, 55.25113791807857666 ) ) ;
#28767 = AXIS2_PLACEMENT_3D ( 'NONE', #31284, #25656, #7270 ) ;
#28768 = CARTESIAN_POINT ( 'NONE',  ( 9.680171189290716072, 214.0920067884432854, 18.69886208192143684 ) ) ;
#28769 = CARTESIAN_POINT ( 'NONE',  ( 10.00000000000000711, 207.0476921513415220, 24.99886208192143400 ) ) ;
#28770 = CARTESIAN_POINT ( 'NONE',  ( 81.99999999453763166, 155.0000000000000000, -14.50000000000000711 ) ) ;
#28771 = CARTESIAN_POINT ( 'NONE',  ( -7.456977232089304408, 196.8216656703010301, 63.05113791807858092 ) ) ;
#28772 = CARTESIAN_POINT ( 'NONE',  ( -2.426778023690262742, 214.6231898156240163, 91.10113791807859229 ) ) ;
#28773 = CARTESIAN_POINT ( 'NONE',  ( -8.062137200540822946, 201.0835637161416400, 53.19886208192143329 ) ) ;
#28774 = DIRECTION ( 'NONE',  ( -0.000000000000000000, -0.000000000000000000, 1.000000000000000000 ) ) ;
#28776 = EDGE_LOOP ( 'NONE', ( #20017, #21384, #17759, #159, #29813, #18834, #15144 ) ) ;
#28775 = B_SPLINE_CURVE_WITH_KNOTS ( 'NONE', 3,
 ( #15215, #9590, #33104, #24934, #2272, #14532, #30728, #19821, #22883, #7387 ),
 .UNSPECIFIED., .F., .F.,
 ( 4, 2, 2, 2, 4 ),
 ( 0.01606529487141865678, 0.01806591702017409581, 0.02006653916892953138, 0.02406778346644039557, 0.03207027206146212395 ),
 .UNSPECIFIED. ) ;
#28777 = CARTESIAN_POINT ( 'NONE',  ( -9.680171189290716072, 199.9079932115567146, 56.19886208192144039 ) ) ;
#28778 = ORIENTED_EDGE ( 'NONE', *, *, #20637, .F. ) ;
#28779 = VECTOR ( 'NONE', #1067, 1000.000000000000114 ) ;
#28780 = ORIENTED_EDGE ( 'NONE', *, *, #18328, .F. ) ;
#28781 = CARTESIAN_POINT ( 'NONE',  ( 92.60208470531341618, 155.0000000000000000, 0.000000000000000000 ) ) ;
#28782 = CARTESIAN_POINT ( 'NONE',  ( -3.135527875058982783, 216.4958274776886924, 54.09886208192143897 ) ) ;
#28783 = CARTESIAN_POINT ( 'NONE',  ( 125.5000000000000000, 154.9999999999996305, -106.0000000000000142 ) ) ;
#28784 = CARTESIAN_POINT ( 'NONE',  ( -2.426778023690262742, 214.6231898156240163, 43.10113791807857808 ) ) ;
#28785 = CARTESIAN_POINT ( 'NONE',  ( 82.51132485994280330, 163.8167787843871110, 12.13525491562421621 ) ) ;
#28786 = APPLICATION_CONTEXT ( 'automotive_design' ) ;
#28787 = CARTESIAN_POINT ( 'NONE',  ( -8.062137200540822946, 201.0835637161416400, 23.19886208192143684 ) ) ;
#28788 = CARTESIAN_POINT ( 'NONE',  ( 63.37499999726880873, 155.0000000000000000, -15.58253175000000823 ) ) ;
#28790 = EDGE_LOOP ( 'NONE', ( #15110, #13976, #30579, #31204, #31259 ) ) ;
#28789 = AXIS2_PLACEMENT_3D ( 'NONE', #27289, #3946, #26485 ) ;
#28791 = FACE_OUTER_BOUND ( 'NONE', #18931, .T. ) ;
#28792 = SURFACE_STYLE_USAGE ( .BOTH. , #8180 ) ;
#28793 = DIRECTION ( 'NONE',  ( 0.000000000000000000, -0.7071067811865330288, 0.7071067811865621167 ) ) ;
#28794 = CARTESIAN_POINT ( 'NONE',  ( 4.984841277089891776, 200.2242689037093726, 1.448862081921434841 ) ) ;
#28795 = CARTESIAN_POINT ( 'NONE',  ( 9.984503880673470277, 203.7031108863295401, 38.15113791807856813 ) ) ;
#28796 = CARTESIAN_POINT ( 'NONE',  ( 8.118202686958039038, 212.8392687619912635, 31.70113791807856884 ) ) ;
#28797 = CARTESIAN_POINT ( 'NONE',  ( -8.118202686958138514, 212.8392687619910930, 101.7988620819214418 ) ) ;
#28798 = APPLICATION_PROTOCOL_DEFINITION ( 'draft international standard', 'automotive_design', 1998, #15501 ) ;
#28799 = CARTESIAN_POINT ( 'NONE',  ( -6.500168698208244500, 211.6636982574061676, 92.79886208192142760 ) ) ;
#28800 = CARTESIAN_POINT ( 'NONE',  ( 37.92499999726881299, 164.1591823560292198, 12.60653300113718167 ) ) ;
#28801 = FILL_AREA_STYLE_COLOUR ( '', #30700 ) ;
#28802 = DIRECTION ( 'NONE',  ( 0.000000000000000000, 1.000000000000000000, -1.295896757998781966E-15 ) ) ;
#28803 = CARTESIAN_POINT ( 'NONE',  ( -3.662846001190052991, 218.4274158808045740, 13.10113791807856742 ) ) ;
#28804 = AXIS2_PLACEMENT_3D ( 'NONE', #9057, #9561, #27455 ) ;
#28805 = FACE_OUTER_BOUND ( 'NONE', #7630, .T. ) ;
#28806 = CARTESIAN_POINT ( 'NONE',  ( 55.07499999726879736, 141.7447067706911810, -9.630534252274385310 ) ) ;
#28807 = CARTESIAN_POINT ( 'NONE',  ( -10.01549611932653860, 203.7984951890123284, 54.35113791807856387 ) ) ;
#28808 = CARTESIAN_POINT ( 'NONE',  ( -3.044812012440131443, 216.5253028482142952, 31.10113791807856742 ) ) ;
#28809 = CARTESIAN_POINT ( 'NONE',  ( -7.500000000000000000, 4.330127018922191873, -7.422398894150032511 ) ) ;
#28810 = LINE ( 'NONE', #2915, #21143 ) ;
#28811 = CARTESIAN_POINT ( 'NONE',  ( 58.89999999453761603, 159.7113355953771077, 14.49999999999999289 ) ) ;
#28812 = ORIENTED_EDGE ( 'NONE', *, *, #2955, .F. ) ;
#28813 = CARTESIAN_POINT ( 'NONE',  ( -9.680171189290831535, 214.0920067884431148, 42.80113791807857382 ) ) ;
#28814 = CARTESIAN_POINT ( 'NONE',  ( 37.18867513459482410, 169.2658477444273331, -4.635254915624224203 ) ) ;
#28815 = UNCERTAINTY_MEASURE_WITH_UNIT (LENGTH_MEASURE( 1.000000000000000082E-05 ), #20951, 'distance_accuracy_value', 'NONE');
#28816 = CARTESIAN_POINT ( 'NONE',  ( 3.044812012439969795, 216.5253028482143520, 21.39886208192143613 ) ) ;
#28817 = CARTESIAN_POINT ( 'NONE',  ( 71.48867513459484258, 167.7597621252805880, 9.270509831248428867 ) ) ;
#28818 = ORIENTED_EDGE ( 'NONE', *, *, #344, .T. ) ;
#28819 = CARTESIAN_POINT ( 'NONE',  ( -0.05014649552810635652, 196.4853777576173002, 74.75113791807858377 ) ) ;
#28820 = ORIENTED_EDGE ( 'NONE', *, *, #12863, .T. ) ;
#28821 = DIRECTION ( 'NONE',  ( 0.000000000000000000, 0.7071067811865540120, 0.7071067811865411334 ) ) ;
#28822 = ORIENTED_EDGE ( 'NONE', *, *, #8909, .T. ) ;
#28823 = CARTESIAN_POINT ( 'NONE',  ( -8.015496119326531499, 204.4483345814780364, 12.35113791807856565 ) ) ;
#28824 = CIRCLE ( 'NONE', #16698, 11.99999999999998224 ) ;
#28825 = CARTESIAN_POINT ( 'NONE',  ( -9.680171189290716072, 199.9079932115567146, 101.1988620819214475 ) ) ;
#28826 = CARTESIAN_POINT ( 'NONE',  ( 44.97499999726881015, 140.1801316387863778, -4.815267126137194431 ) ) ;
#28827 = ORIENTED_EDGE ( 'NONE', *, *, #6811, .F. ) ;
#28828 = CARTESIAN_POINT ( 'NONE',  ( 53.72499999726881015, 169.8198683612136222, 4.815267126137181997 ) ) ;
#28829 = CARTESIAN_POINT ( 'NONE',  ( 7.500000000000001776, 0.000000000000000000, 0.000000000000000000 ) ) ;
#28830 = CARTESIAN_POINT ( 'NONE',  ( -3.044812012440131443, 216.5253028482142952, 13.10113791807856742 ) ) ;
#28831 = CARTESIAN_POINT ( 'NONE',  ( -8.062137200540822946, 201.0835637161416400, 77.19886208192143329 ) ) ;
#28832 = CARTESIAN_POINT ( 'NONE',  ( 54.67499999726881299, 141.7447067706911810, 9.630534252274376428 ) ) ;
#28833 = FACE_OUTER_BOUND ( 'NONE', #30160, .T. ) ;
#28834 = CARTESIAN_POINT ( 'NONE',  ( 6.220909254589536808, 215.4770327129947702, 10.55113791807856138 ) ) ;
#28835 = DIRECTION ( 'NONE',  ( -1.000000000000000000, -0.000000000000000000, -0.000000000000000000 ) ) ;
#28836 = B_SPLINE_CURVE_WITH_KNOTS ( 'NONE', 3,
 ( #26996, #3657, #1111, #14051, #24447, #17623 ),
 .UNSPECIFIED., .F., .F.,
 ( 4, 2, 4 ),
 ( 0.003841072314098365435, 0.005765657563962188134, 0.007690242813826009965 ),
 .UNSPECIFIED. ) ;
#28837 = CARTESIAN_POINT ( 'NONE',  ( 68.40000000000000568, 150.2886644046228639, -14.50000000000000888 ) ) ;
#28838 = CARTESIAN_POINT ( 'NONE',  ( -6.139770520408369237, 215.5359834540460042, 96.95113791807857240 ) ) ;
#28839 = CARTESIAN_POINT ( 'NONE',  ( 38.38867513459481984, 140.7341522555726669, -4.635254915624220651 ) ) ;
#28840 = CARTESIAN_POINT ( 'NONE',  ( 10.01549611932653860, 210.2015048109876716, 88.85113791807857808 ) ) ;
#28841 = CARTESIAN_POINT ( 'NONE',  ( 3.500000000000004885, 1.693985822988438139, -0.2182856432892083254 ) ) ;
#28842 = CARTESIAN_POINT ( 'NONE',  ( 39.57499999726881157, 164.1591823560292198, -12.60653300113719766 ) ) ;
#28843 = CARTESIAN_POINT ( 'NONE',  ( 9.736236675708031640, 199.9851607334238963, 94.29886208192142760 ) ) ;
#28844 = EDGE_CURVE ( 'NONE', #17702, #8324, #22265, .T. ) ;
#28845 = CARTESIAN_POINT ( 'NONE',  ( 69.52499999726880731, 169.8198683612136222, -4.815267126137197984 ) ) ;
#28846 = VERTEX_POINT ( 'NONE', #845 ) ;
#28847 = CARTESIAN_POINT ( 'NONE',  ( 3.999999999999999112, 4.898587196589411843E-16, -7.974599999999998801 ) ) ;
#28848 = CARTESIAN_POINT ( 'NONE',  ( 42.09999999453762598, 159.7113355953771077, -14.50000000000000888 ) ) ;
#28849 = CARTESIAN_POINT ( 'NONE',  ( -12.00000000000000711, 206.9523078486584780, 5.498862081921433997 ) ) ;
#28850 = CARTESIAN_POINT ( 'NONE',  ( 32.50000000000000000, 155.0000000000000000, -6.938893903907228378E-15 ) ) ;
#28851 = VERTEX_POINT ( 'NONE', #11233 ) ;
#28852 = CARTESIAN_POINT ( 'NONE',  ( -6.139770520408224463, 198.4640165459539105, 95.04886208192144181 ) ) ;
#28853 = CARTESIAN_POINT ( 'NONE',  ( 7.456977232089471386, 196.8216656703012006, 34.44886208192142618 ) ) ;
#28854 = DIRECTION ( 'NONE',  ( 0.000000000000000000, 1.000000000000000000, -1.224646799147353207E-16 ) ) ;
#28855 = CARTESIAN_POINT ( 'NONE',  ( -0.05014649552810635652, 196.4853777576173002, 44.75113791807858377 ) ) ;
#28856 = EDGE_LOOP ( 'NONE', ( #20841, #9487 ) ) ;
#28857 = CARTESIAN_POINT ( 'NONE',  ( 8.000000000000008882, 207.0476921513415220, 0.9988620819214347746 ) ) ;
#28858 = FACE_OUTER_BOUND ( 'NONE', #1577, .T. ) ;
#28859 = EDGE_LOOP ( 'NONE', ( #24660, #22432, #23912, #5304, #428 ) ) ;
#28860 = CARTESIAN_POINT ( 'NONE',  ( 8.000000000000008882, 207.0476921513415220, 93.99886208192144466 ) ) ;
#28861 = CARTESIAN_POINT ( 'NONE',  ( 0.05014649552807626948, 215.4116977939061144, 28.25113791807856245 ) ) ;
#28862 = CARTESIAN_POINT ( 'NONE',  ( 7.500000000000000888, -3.640541674360523228, -0.7158139487964624292 ) ) ;
#28863 = ORIENTED_EDGE ( 'NONE', *, *, #11801, .T. ) ;
#28864 = CARTESIAN_POINT ( 'NONE',  ( 101.3062541159399075, 155.0000000000000000, 0.000000000000000000 ) ) ;
#28865 = CARTESIAN_POINT ( 'NONE',  ( 35.77499999726881441, 169.8198683612136222, -4.815267126137197984 ) ) ;
#28866 = DIRECTION ( 'NONE',  ( -0.000000000000000000, -0.000000000000000000, 1.000000000000000000 ) ) ;
#28867 = CARTESIAN_POINT ( 'NONE',  ( -4.984841277089726574, 200.2242689037092305, 93.05113791807858092 ) ) ;
#28868 = CARTESIAN_POINT ( 'NONE',  ( 0.000000000000000000, 0.000000000000000000, 0.000000000000000000 ) ) ;
#28869 = CARTESIAN_POINT ( 'NONE',  ( 47.89999999999999858, 141.2096805137202580, 4.480746418436733158 ) ) ;
#28870 = CARTESIAN_POINT ( 'NONE',  ( 0.05014649552828262524, 198.5883022060938572, 58.74886208192143755 ) ) ;
#28871 = CARTESIAN_POINT ( 'NONE',  ( 83.91132485994279477, 163.8167787843871110, -12.13525491562423397 ) ) ;
#28872 = EDGE_CURVE ( 'NONE', #747, #2428, #17305, .T. ) ;
#28873 = CIRCLE ( 'NONE', #33235, 100.0000000000000000 ) ;
#28874 = CARTESIAN_POINT ( 'NONE',  ( 48.82499999726880446, 141.7447067706911810, -9.630534252274385310 ) ) ;
#28876 = ORIENTED_EDGE ( 'NONE', *, *, #5778, .F. ) ;
#28875 = CARTESIAN_POINT ( 'NONE',  ( -8.062137200540920645, 212.9164362838581894, 12.80113791807856671 ) ) ;
#28877 = LINE ( 'NONE', #18163, #11922 ) ;
#28878 = AXIS2_PLACEMENT_3D ( 'NONE', #4570, #4055, #1340 ) ;
#28879 = CARTESIAN_POINT ( 'NONE',  ( 60.72499999726881015, 140.1801316387863778, -4.815267126137194431 ) ) ;
#28880 = CARTESIAN_POINT ( 'NONE',  ( 76.17499999726881299, 164.1591823560292198, 12.60653300113718167 ) ) ;
#28881 = CARTESIAN_POINT ( 'NONE',  ( -3.753561863808691168, 195.6020594897209435, 62.90113791807858945 ) ) ;
#28882 = FACE_OUTER_BOUND ( 'NONE', #14018, .T. ) ;
#28883 = CARTESIAN_POINT ( 'NONE',  ( -8.118202686958039038, 201.1607312380087080, 90.20113791807857240 ) ) ;
#28884 = CARTESIAN_POINT ( 'NONE',  ( 35.78867513459482552, 155.0000000000000000, 15.00000000000001243 ) ) ;
#28885 = EDGE_CURVE ( 'NONE', #13926, #31163, #10774, .T. ) ;
#28886 = ORIENTED_EDGE ( 'NONE', *, *, #21018, .F. ) ;
#28887 = CARTESIAN_POINT ( 'NONE',  ( 12.00000000000000711, 207.0476921513415220, 54.99886208192144466 ) ) ;
#28888 = CARTESIAN_POINT ( 'NONE',  ( 10.01549611932659367, 203.7984951890124421, 70.14886208192142192 ) ) ;
#28889 = CARTESIAN_POINT ( 'NONE',  ( -11.98450388067348804, 210.9467285061362247, 96.65113791807858945 ) ) ;
#28890 = DIRECTION ( 'NONE',  ( 0.000000000000000000, 0.000000000000000000, 1.000000000000000000 ) ) ;
#28891 = CARTESIAN_POINT ( 'NONE',  ( 6.139770520408368348, 198.4640165459539674, 11.45113791807856707 ) ) ;
#28892 = CARTESIAN_POINT ( 'NONE',  ( 9.984503880673420539, 210.2968891136705167, 78.84886208192139634 ) ) ;
#28893 = VERTEX_POINT ( 'NONE', #16675 ) ;
#28894 = CARTESIAN_POINT ( 'NONE',  ( -3.044812012440131443, 216.5253028482142952, 97.10113791807857808 ) ) ;
#28895 = EDGE_LOOP ( 'NONE', ( #5839, #12227, #16314 ) ) ;
#28896 = DIRECTION ( 'NONE',  ( -1.000000000000000000, 0.000000000000000000, 0.000000000000000000 ) ) ;
#28897 = CARTESIAN_POINT ( 'NONE',  ( -4.984841277089891776, 213.7757310962905990, 59.94886208192144039 ) ) ;
#28898 = VERTEX_POINT ( 'NONE', #19240 ) ;
#28899 = EDGE_CURVE ( 'NONE', #28445, #13382, #10268, .T. ) ;
#28900 = CARTESIAN_POINT ( 'NONE',  ( 76.52499999726880731, 140.1801316387863778, 4.815267126137185549 ) ) ;
#28901 = LINE ( 'NONE', #11015, #10295 ) ;
#28902 = DIRECTION ( 'NONE',  ( -1.000000000000000000, 0.000000000000000000, 0.000000000000000000 ) ) ;
#28903 = B_SPLINE_CURVE_WITH_KNOTS ( 'NONE', 3,
 ( #13738, #18854, #32133, #29415, #21246, #3190 ),
 .UNSPECIFIED., .F., .F.,
 ( 4, 2, 4 ),
 ( 2.475503369212747145E-07, 0.002222330217055634109, 0.004444412883774346255 ),
 .UNSPECIFIED. ) ;
#28904 = EDGE_CURVE ( 'NONE', #5683, #10401, #25452, .T. ) ;
#28905 = CARTESIAN_POINT ( 'NONE',  ( 72.82499999726879025, 141.7447067706911810, -9.630534252274385310 ) ) ;
#28906 = CARTESIAN_POINT ( 'NONE',  ( -8.000000000000008882, 207.0476921513413515, 60.50113791807857666 ) ) ;
#28907 = PRESENTATION_STYLE_ASSIGNMENT (( #462 ) ) ;
#28908 = FACE_OUTER_BOUND ( 'NONE', #18800, .T. ) ;
#28909 = CARTESIAN_POINT ( 'NONE',  ( 92.70168066101555837, 155.0000000000000000, 0.000000000000000000 ) ) ;
#28910 = CARTESIAN_POINT ( 'NONE',  ( 4.903702542908435547, 213.8346818373419751, 30.54886208192144181 ) ) ;
#28911 = CARTESIAN_POINT ( 'NONE',  ( -6.139770520408369237, 215.5359834540460042, 81.95113791807854398 ) ) ;
#28912 = DIRECTION ( 'NONE',  ( 1.000000000000000000, 0.000000000000000000, 0.000000000000000000 ) ) ;
#28913 = CARTESIAN_POINT ( 'NONE',  ( -8.118202686958039038, 201.1607312380087080, 60.20113791807857240 ) ) ;
#28914 = CARTESIAN_POINT ( 'NONE',  ( -6.220909254589537696, 198.5229672870051161, 27.05113791807856671 ) ) ;
#28915 = CARTESIAN_POINT ( 'NONE',  ( 8.000000000000008882, 206.9523078486586485, 14.00113791807856600 ) ) ;
#28916 = CARTESIAN_POINT ( 'NONE',  ( 87.37499999726880162, 155.0000000000000000, -15.58253175000000823 ) ) ;
#28917 = CARTESIAN_POINT ( 'NONE',  ( 60.08867513459482979, 142.2402378747194405, 9.270509831248432420 ) ) ;
#28918 = CARTESIAN_POINT ( 'NONE',  ( 46.22499999726880304, 149.9369285172503510, 15.58253174999999580 ) ) ;
#28919 = CARTESIAN_POINT ( 'NONE',  ( 3.662846001190051659, 195.5725841191953691, 35.60113791807855677 ) ) ;
#28920 = CARTESIAN_POINT ( 'NONE',  ( 7.914973979435151463, 3.817460047930444134, -7.907502498112419786 ) ) ;
#28921 = CARTESIAN_POINT ( 'NONE',  ( -6.139770520408369237, 215.5359834540460042, 81.95113791807854398 ) ) ;
#28922 = CARTESIAN_POINT ( 'NONE',  ( 0.05014649552810506589, 217.5146222423826714, 61.25113791807856956 ) ) ;
#28923 = CARTESIAN_POINT ( 'NONE',  ( -12.00000000000000711, 206.9523078486584780, 20.49886208192143755 ) ) ;
#28924 = CARTESIAN_POINT ( 'NONE',  ( 3.044812012439969795, 216.5253028482143520, 24.39886208192143613 ) ) ;
#28925 = CIRCLE ( 'NONE', #8257, 27.50000000000000355 ) ;
#28926 = CARTESIAN_POINT ( 'NONE',  ( 82.59999999453762598, 168.7903194862797420, 4.480746418436729606 ) ) ;
#28927 = CARTESIAN_POINT ( 'NONE',  ( -3.662846001190052991, 218.4274158808045740, 67.10113791807857808 ) ) ;
#28928 = CARTESIAN_POINT ( 'NONE',  ( -7.984503880673488041, 209.6470497212046098, 87.65113791807857524 ) ) ;
#28929 = EDGE_CURVE ( 'NONE', #22951, #14728, #9345, .T. ) ;
#28930 = CARTESIAN_POINT ( 'NONE',  ( 3.044812012439969795, 216.5253028482143520, 54.39886208192143613 ) ) ;
#28931 = EDGE_CURVE ( 'NONE', #29153, #7879, #19465, .T. ) ;
#28932 = CARTESIAN_POINT ( 'NONE',  ( 91.60208470531341618, 155.0000000000000000, 0.000000000000000000 ) ) ;
#28933 = EDGE_LOOP ( 'NONE', ( #27337, #28442, #17191 ) ) ;
#28934 = CARTESIAN_POINT ( 'NONE',  ( -12.00000000000000711, 206.9523078486584780, 56.49886208192144466 ) ) ;
#28935 = AXIS2_PLACEMENT_3D ( 'NONE', #9765, #17254, #27477 ) ;
#28936 = ORIENTED_EDGE ( 'NONE', *, *, #3089, .F. ) ;
#28937 = ORIENTED_EDGE ( 'NONE', *, *, #5625, .F. ) ;
#28938 = EDGE_CURVE ( 'NONE', #20128, #32783, #2025, .T. ) ;
#28939 = CARTESIAN_POINT ( 'NONE',  ( 79.17499999726881299, 145.8408176439707802, -12.60653300113719588 ) ) ;
#28940 = CARTESIAN_POINT ( 'NONE',  ( 0.000000000000000000, 0.000000000000000000, -0.4201245229258211977 ) ) ;
#28941 = DIRECTION ( 'NONE',  ( -0.000000000000000000, -0.000000000000000000, 1.000000000000000000 ) ) ;
#28942 = CARTESIAN_POINT ( 'NONE',  ( 2.426778023690261410, 199.3768101843759837, 41.60113791807857808 ) ) ;
#28943 =( BOUNDED_SURFACE ( )  B_SPLINE_SURFACE ( 3, 2, ( 
 ( #6783, #28069, #4393 ),
 ( #4569, #10032, #17169 ),
 ( #12400, #2012, #27896 ),
 ( #9503, #14779, #22617 ),
 ( #19889, #17851, #4732 ),
 ( #15121, #12059, #22797 ) ),
 .UNSPECIFIED., .F., .F., .T. ) 
 B_SPLINE_SURFACE_WITH_KNOTS ( ( 4, 2, 4 ),
 ( 3, 3 ),
 ( 0.003190620565844226857, 0.007281897438794493645, 0.01137317431174476000 ),
 ( 0.000000000000000000, 1.000000000000000000 ),
 .UNSPECIFIED. ) 
 GEOMETRIC_REPRESENTATION_ITEM ( )  RATIONAL_B_SPLINE_SURFACE ( (
 ( 1.000000000000000000, 0.8047731410850399447, 1.000000000000000000),
 ( 1.000000000000000000, 0.8125552299147021929, 1.000000000000000000),
 ( 1.000000000000000000, 0.8191520442902128218, 1.000000000000000000),
 ( 1.000000000000000000, 0.8191520442877616714, 1.000000000000000000),
 ( 1.000000000000000000, 0.8125552299165426096, 1.000000000000000000),
 ( 1.000000000000000000, 0.8047731410850402778, 1.000000000000000000) ) ) 
 REPRESENTATION_ITEM ( '' )  SURFACE ( )  );
#28944 = ADVANCED_FACE ( 'NONE', ( #12413 ), #17358, .T. ) ;
#28945 = FILL_AREA_STYLE ('',( #500 ) ) ;
#28946 = CARTESIAN_POINT ( 'NONE',  ( 6.220909254589681581, 198.5229672870052582, 25.44886208192143684 ) ) ;
#28947 = CARTESIAN_POINT ( 'NONE',  ( 60.87499999726880162, 138.6155565068815747, -3.929120461958505118E-15 ) ) ;
#28948 = ORIENTED_EDGE ( 'NONE', *, *, #23228, .T. ) ;
#28949 = CARTESIAN_POINT ( 'NONE',  ( 62.08867513459483689, 142.2402378747194405, 9.270509831248432420 ) ) ;
#28950 = SURFACE_STYLE_FILL_AREA ( #330 ) ;
#28951 = CARTESIAN_POINT ( 'NONE',  ( -2.621086668468698644, -7.606368536631371136, -7.634085501268427443 ) ) ;
#28952 = CARTESIAN_POINT ( 'NONE',  ( 4.984841277089891776, 200.2242689037093726, 10.44886208192143506 ) ) ;
#28953 = CARTESIAN_POINT ( 'NONE',  ( 8.062137200540920645, 201.0835637161417822, 56.30113791807857382 ) ) ;
#28954 = DIRECTION ( 'NONE',  ( 0.000000000000000000, 0.000000000000000000, -1.000000000000000000 ) ) ;
#28955 = CARTESIAN_POINT ( 'NONE',  ( 6.139770520408368348, 198.4640165459539674, 23.45113791807856884 ) ) ;
#28956 = CARTESIAN_POINT ( 'NONE',  ( 83.37499999726881583, 155.0000000000000000, -15.58253175000000823 ) ) ;
#28957 = SHAPE_DEFINITION_REPRESENTATION ( #21913, #32415 ) ;
#28958 = CARTESIAN_POINT ( 'NONE',  ( -8.015496119326597224, 209.5516654185217362, 92.64886208192143613 ) ) ;
#28959 = AXIS2_PLACEMENT_3D ( 'NONE', #9817, #12197, #20198 ) ;
#28960 = CARTESIAN_POINT ( 'NONE',  ( 38.62499999726880873, 138.6155565068815463, -3.929120461958505118E-15 ) ) ;
#28961 = DIRECTION ( 'NONE',  ( 0.000000000000000000, 2.081668171172168119E-15, -1.000000000000000000 ) ) ;
#28962 = CARTESIAN_POINT ( 'NONE',  ( 11.98450388067348271, 203.0532714938637753, 11.15113791807856636 ) ) ;
#28963 = FACE_OUTER_BOUND ( 'NONE', #25636, .T. ) ;
#28964 = CARTESIAN_POINT ( 'NONE',  ( 57.97499999726881015, 169.8198683612136222, 4.815267126137181997 ) ) ;
#28965 = VECTOR ( 'NONE', #2080, 1000.000000000000000 ) ;
#28966 = CARTESIAN_POINT ( 'NONE',  ( 3.135527875058820690, 216.4958274776887492, 52.40113791807857524 ) ) ;
#28967 = CARTESIAN_POINT ( 'NONE',  ( -9.984503880673475606, 210.2968891136704315, 33.65113791807856813 ) ) ;
#28968 = LINE ( 'NONE', #19074, #11057 ) ;
#28969 = CYLINDRICAL_SURFACE ( 'NONE', #11409, 0.9999999999999953371 ) ;
#28970 = CARTESIAN_POINT ( 'NONE',  ( -0.05014649552828402690, 217.5146222423826714, 3.248862081921434442 ) ) ;
#28971 = CARTESIAN_POINT ( 'NONE',  ( 57.29999999453762882, 142.6655632788954620, 8.961492836873471646 ) ) ;
#28972 = VERTEX_POINT ( 'NONE', #4581 ) ;
#28973 = CARTESIAN_POINT ( 'NONE',  ( 11.98450388067348271, 203.0532714938637753, 35.15113791807856103 ) ) ;
#28974 = FACE_OUTER_BOUND ( 'NONE', #25805, .T. ) ;
#28975 = CARTESIAN_POINT ( 'NONE',  ( 9.984503880673420539, 210.2968891136705167, 24.84886208192143897 ) ) ;
#28976 = ADVANCED_FACE ( 'NONE', ( #22809 ), #14631, .F. ) ;
#28977 = CARTESIAN_POINT ( 'NONE',  ( 72.71132485994280614, 155.0000000000000000, 15.00000000000001243 ) ) ;
#28978 = ORIENTED_EDGE ( 'NONE', *, *, #2624, .F. ) ;
#28979 = AXIS2_PLACEMENT_3D ( 'NONE', #3470, #9552, #753 ) ;
#28980 = CARTESIAN_POINT ( 'NONE',  ( 10.01549611932653860, 210.2015048109876716, 76.85113791807857808 ) ) ;
#28981 = ORIENTED_EDGE ( 'NONE', *, *, #12014, .T. ) ;
#28982 = EDGE_CURVE ( 'NONE', #17237, #28748, #25027, .T. ) ;
#28983 = DIRECTION ( 'NONE',  ( -1.000000000000000000, -0.000000000000000000, -0.000000000000000000 ) ) ;
#28984 = DIRECTION ( 'NONE',  ( 0.000000000000000000, 0.000000000000000000, -1.000000000000000000 ) ) ;
#28985 = ORIENTED_EDGE ( 'NONE', *, *, #6166, .F. ) ;
#28986 = CIRCLE ( 'NONE', #2872, 70.00000000000002842 ) ;
#28987 = CARTESIAN_POINT ( 'NONE',  ( 4.984841277089725686, 213.7757310962907411, 16.55113791807857027 ) ) ;
#28988 = AXIS2_PLACEMENT_3D ( 'NONE', #9792, #17451, #4000 ) ;
#28989 = CARTESIAN_POINT ( 'NONE',  ( 7.456977232089471386, 196.8216656703012006, 97.44886208192143329 ) ) ;
#28990 = CARTESIAN_POINT ( 'NONE',  ( 42.87499999726881583, 138.6155565068815747, -3.929120461958505118E-15 ) ) ;
#28991 = EDGE_LOOP ( 'NONE', ( #16516, #24537, #13468, #88, #24783 ) ) ;
#28992 = CARTESIAN_POINT ( 'NONE',  ( 49.52499999726880731, 169.8198683612136222, -4.815267126137197984 ) ) ;
#28993 = CYLINDRICAL_SURFACE ( 'NONE', #20815, 112.0000000000000426 ) ;
#28994 = CARTESIAN_POINT ( 'NONE',  ( -8.062137200540920645, 212.9164362838581894, 6.801137918078565825 ) ) ;
#28995 = CARTESIAN_POINT ( 'NONE',  ( 0.05014649552828275708, 196.4853777576173002, 85.74886208192140202 ) ) ;
#28996 = CARTESIAN_POINT ( 'NONE',  ( 54.07499999726880446, 168.2552932293087906, 9.630534252274372875 ) ) ;
#28997 = CARTESIAN_POINT ( 'NONE',  ( 0.05014649552810505201, 217.5146222423826714, 25.25113791807856245 ) ) ;
#28998 = FACE_OUTER_BOUND ( 'NONE', #29696, .T. ) ;
#28999 = VECTOR ( 'NONE', #17017, 1000.000000000000000 ) ;
#29000 = CARTESIAN_POINT ( 'NONE',  ( 71.00000000000000000, 170.2462022514548323, -7.872454543227099337E-15 ) ) ;
#29001 = CARTESIAN_POINT ( 'NONE',  ( -3.044812012440131443, 216.5253028482142952, 100.1011379180785781 ) ) ;
#29002 = DIRECTION ( 'NONE',  ( 0.1045284632676459352, 1.217938055844715641E-16, 0.9945218953682740670 ) ) ;
#29003 = CARTESIAN_POINT ( 'NONE',  ( 3.135527875058820690, 216.4958274776887492, 82.40113791807857524 ) ) ;
#29004 = LINE ( 'NONE', #26121, #15654 ) ;
#29005 = CARTESIAN_POINT ( 'NONE',  ( 36.87499999726881583, 138.6155565068815463, -3.929120461958505118E-15 ) ) ;
#29006 = CARTESIAN_POINT ( 'NONE',  ( 9.736236675708031640, 199.9851607334238963, 97.29886208192142760 ) ) ;
#29007 = CARTESIAN_POINT ( 'NONE',  ( 78.62499999726881583, 138.6155565068815463, -3.929120461958505118E-15 ) ) ;
#29008 = ORIENTED_EDGE ( 'NONE', *, *, #17060, .F. ) ;
#29009 = CARTESIAN_POINT ( 'NONE',  ( 48.41132485994280898, 167.7597621252805880, 9.270509831248428867 ) ) ;
#29010 = VECTOR ( 'NONE', #15548, 1000.000000000000000 ) ;
#29011 = CARTESIAN_POINT ( 'NONE',  ( 41.59999999453763309, 141.2096805137202580, -4.480746418436742040 ) ) ;
#29012 = AXIS2_PLACEMENT_3D ( 'NONE', #19474, #27808, #9584 ) ;
#29013 = VECTOR ( 'NONE', #21683, 1000.000000000000000 ) ;
#29014 = CARTESIAN_POINT ( 'NONE',  ( -6.500000000000000000, 3.752776749732564809, -8.000000000000000000 ) ) ;
#29015 = CIRCLE ( 'NONE', #182, 5.250000000000004441 ) ;
#29016 = DIRECTION ( 'NONE',  ( 0.000000000000000000, 0.000000000000000000, -1.000000000000000000 ) ) ;
#29017 = ORIENTED_EDGE ( 'NONE', *, *, #30996, .F. ) ;
#29018 = CARTESIAN_POINT ( 'NONE',  ( 3.135527875058981895, 197.5041725223112792, 94.59886208192143897 ) ) ;
#29019 = CARTESIAN_POINT ( 'NONE',  ( 3.662846001189864698, 218.4274158808046593, 33.39886208192143613 ) ) ;
#29020 = CARTESIAN_POINT ( 'NONE',  ( 91.60208470531341618, 155.0000000000000000, 12.00000000000001066 ) ) ;
#29021 = CARTESIAN_POINT ( 'NONE',  ( -10.00000000000000711, 207.0476921513413515, 42.50113791807856956 ) ) ;
#29022 = ORIENTED_EDGE ( 'NONE', *, *, #11053, .F. ) ;
#29023 = CARTESIAN_POINT ( 'NONE',  ( -0.05014649552828365914, 215.4116977939061144, 3.248862081921435330 ) ) ;
#29024 = CARTESIAN_POINT ( 'NONE',  ( -13.75000000000001243, -23.81569860407206107, 0.000000000000000000 ) ) ;
#29025 = VERTEX_POINT ( 'NONE', #9187 ) ;
#29027 = CARTESIAN_POINT ( 'NONE',  ( -4.984841277089891776, 213.7757310962905990, 92.94886208192144750 ) ) ;
#29026 =( GEOMETRIC_REPRESENTATION_CONTEXT ( 3 ) GLOBAL_UNCERTAINTY_ASSIGNED_CONTEXT ( ( #1240 ) ) GLOBAL_UNIT_ASSIGNED_CONTEXT ( ( #4525, #20372, #20193 ) ) REPRESENTATION_CONTEXT ( 'NONE', 'WORKASPACE' ) );
#29028 = EDGE_CURVE ( 'NONE', #17153, #31012, #11319, .T. ) ;
#29029 =( REPRESENTATION_RELATIONSHIP ('NONE','NONE', #25663, #21975 ) REPRESENTATION_RELATIONSHIP_WITH_TRANSFORMATION ( #31678 )SHAPE_REPRESENTATION_RELATIONSHIP( ) );
#29030 = CARTESIAN_POINT ( 'NONE',  ( -7.984503880673488041, 209.6470497212046098, 33.65113791807856813 ) ) ;
#29031 = LINE ( 'NONE', #23423, #968 ) ;
#29032 = ORIENTED_EDGE ( 'NONE', *, *, #30605, .F. ) ;
#29033 = CARTESIAN_POINT ( 'NONE',  ( 33.52499999726880731, 169.8198683612136222, -4.815267126137197984 ) ) ;
#29034 = AXIS2_PLACEMENT_3D ( 'NONE', #25389, #30687, #12451 ) ;
#29035 = CONICAL_SURFACE ( 'NONE', #18704, 3.499999999999999556, 1.047197551196589638 ) ;
#29036 = CARTESIAN_POINT ( 'NONE',  ( 33.97499999726881725, 169.8198683612136222, 4.815267126137181997 ) ) ;
#29037 = CARTESIAN_POINT ( 'NONE',  ( -6.500000000000000000, 3.752776749732564809, -6.064240316920399110 ) ) ;
#29038 = CARTESIAN_POINT ( 'NONE',  ( 6.444103211791042618, 202.2591342207267644, 86.30113791807858092 ) ) ;
#29039 = CARTESIAN_POINT ( 'NONE',  ( 0.000000000000000000, 0.000000000000000000, 0.000000000000000000 ) ) ;
#29040 = CARTESIAN_POINT ( 'NONE',  ( 57.19999999999999574, 167.3344367211045096, 8.961492836873468093 ) ) ;
#29041 = CARTESIAN_POINT ( 'NONE',  ( -4.903702542908436435, 200.1653181626580249, 74.04886208192142760 ) ) ;
#29042 = DIRECTION ( 'NONE',  ( 0.000000000000000000, 0.000000000000000000, -1.000000000000000000 ) ) ;
#29043 = CARTESIAN_POINT ( 'NONE',  ( 52.42499999726880588, 141.7447067706911810, 9.630534252274376428 ) ) ;
#29044 = CARTESIAN_POINT ( 'NONE',  ( -10.01549611932653860, 203.7984951890123000, 9.351137918078569200 ) ) ;
#29045 = CARTESIAN_POINT ( 'NONE',  ( 125.5000000000000000, 81.56696077377658582, -76.47359838532473475 ) ) ;
#29046 = CARTESIAN_POINT ( 'NONE',  ( 63.02499999726882152, 149.9369285172503510, -15.58253175000000823 ) ) ;
#29047 = CARTESIAN_POINT ( 'NONE',  ( 75.87499999726881583, 171.3844434931184253, -7.942151717890132712E-15 ) ) ;
#29048 = CARTESIAN_POINT ( 'NONE',  ( 3.662846001190051659, 195.5725841191953691, 74.60113791807854966 ) ) ;
#29049 = B_SPLINE_CURVE_WITH_KNOTS ( 'NONE', 3,
 ( #5570, #29703, #31635, #6539, #1093 ),
 .UNSPECIFIED., .F., .F.,
 ( 4, 1, 4 ),
 ( 0.000000000000000000, 0.003752776749732569198, 0.007505553499465138396 ),
 .UNSPECIFIED. ) ;
#29050 = CARTESIAN_POINT ( 'NONE',  ( -6.837824896291515131, -3.947820044545435447, -6.564402953523717166 ) ) ;
#29051 = CARTESIAN_POINT ( 'NONE',  ( 3.135527875058820690, 216.4958274776887492, 94.40113791807857524 ) ) ;
#29052 = CARTESIAN_POINT ( 'NONE',  ( 102.4138169258850581, 155.0000000000000000, 0.000000000000000000 ) ) ;
#29053 = ORIENTED_EDGE ( 'NONE', *, *, #4303, .F. ) ;
#29054 = CARTESIAN_POINT ( 'NONE',  ( -9.736236675708031640, 214.0148392665760753, 65.79886208192144181 ) ) ;
#29055 = CARTESIAN_POINT ( 'NONE',  ( -8.062137200540822946, 201.0835637161416400, 65.19886208192143329 ) ) ;
#29056 = AXIS2_PLACEMENT_3D ( 'NONE', #30861, #26081, #7525 ) ;
#29057 = CARTESIAN_POINT ( 'NONE',  ( -7.456977232089304408, 196.8216656703010301, 102.0511379180785809 ) ) ;
#29058 = CARTESIAN_POINT ( 'NONE',  ( 33.78867513459482552, 155.0000000000000000, 15.00000000000001243 ) ) ;
#29059 = CARTESIAN_POINT ( 'NONE',  ( 8.118202686958039038, 212.8392687619912635, 16.70113791807856529 ) ) ;
#29060 = VECTOR ( 'NONE', #865, 1000.000000000000000 ) ;
#29061 = CARTESIAN_POINT ( 'NONE',  ( 10.01549611932659545, 203.7984951890123853, 76.14886208192143613 ) ) ;
#29062 = ORIENTED_EDGE ( 'NONE', *, *, #32201, .T. ) ;
#29063 = DIRECTION ( 'NONE',  ( 0.000000000000000000, 0.000000000000000000, -1.000000000000000000 ) ) ;
#29064 = ORIENTED_EDGE ( 'NONE', *, *, #31661, .F. ) ;
#29065 = CARTESIAN_POINT ( 'NONE',  ( 8.015496119326595448, 204.4483345814782638, 58.14886208192145034 ) ) ;
#29066 = ORIENTED_EDGE ( 'NONE', *, *, #8695, .F. ) ;
#29067 = EDGE_CURVE ( 'NONE', #19123, #4327, #11737, .T. ) ;
#29068 = CARTESIAN_POINT ( 'NONE',  ( 80.12499999726881583, 155.0000000000000000, 15.58253174999999402 ) ) ;
#29069 = DIRECTION ( 'NONE',  ( 1.000000000000000000, 0.000000000000000000, 0.000000000000000000 ) ) ;
#29070 = DIRECTION ( 'NONE',  ( 0.000000000000000000, 0.000000000000000000, -1.000000000000000000 ) ) ;
#29071 = EDGE_CURVE ( 'NONE', #32773, #9926, #16846, .T. ) ;
#29072 = UNCERTAINTY_MEASURE_WITH_UNIT (LENGTH_MEASURE( 1.000000000000000082E-05 ), #16114, 'distance_accuracy_value', 'NONE');
#29073 = CARTESIAN_POINT ( 'NONE',  ( 67.52499999726880731, 169.8198683612136222, -4.815267126137197984 ) ) ;
#29074 = CARTESIAN_POINT ( 'NONE',  ( -7.984503880673488041, 209.6470497212046098, 63.65113791807855392 ) ) ;
#29075 = FACE_BOUND ( 'NONE', #16356, .T. ) ;
#29076 = DIRECTION ( 'NONE',  ( 1.000000000000000000, 0.000000000000000000, 0.000000000000000000 ) ) ;
#29077 = EDGE_CURVE ( 'NONE', #6985, #21367, #19577, .T. ) ;
#29078 = AXIS2_PLACEMENT_3D ( 'NONE', #304, #10703, #4362 ) ;
#29079 = PRESENTATION_STYLE_ASSIGNMENT (( #23635 ) ) ;
#29080 = DIRECTION ( 'NONE',  ( 0.000000000000000000, 0.000000000000000000, -1.000000000000000000 ) ) ;
#29081 = CARTESIAN_POINT ( 'NONE',  ( 2.426778023690075337, 214.6231898156240447, 48.39886208192144323 ) ) ;
#29082 = CARTESIAN_POINT ( 'NONE',  ( -0.05014649552810635652, 196.4853777576173002, 80.75113791807854113 ) ) ;
#29083 = CARTESIAN_POINT ( 'NONE',  ( 63.78867513459482552, 155.0000000000000000, 15.00000000000001243 ) ) ;
#29084 = CARTESIAN_POINT ( 'NONE',  ( -8.118202686958039038, 201.1607312380087080, 66.20113791807857240 ) ) ;
#29085 = FACE_OUTER_BOUND ( 'NONE', #16607, .T. ) ;
#29086 = CARTESIAN_POINT ( 'NONE',  ( 0.05014649552807626948, 215.4116977939061144, 13.25113791807856423 ) ) ;
#29087 = DIRECTION ( 'NONE',  ( -0.5000000000000034417, 0.000000000000000000, 0.8660254037844367092 ) ) ;
#29088 = CARTESIAN_POINT ( 'NONE',  ( -3.499999999999999556, -3.004629197474309385E-15, 0.000000000000000000 ) ) ;
#29089 = CARTESIAN_POINT ( 'NONE',  ( 41.62499999726880162, 171.3844434931184253, -7.942151717890134290E-15 ) ) ;
#29090 = CARTESIAN_POINT ( 'NONE',  ( 7.375838497908181246, 196.7627149292499666, 47.45113791807857950 ) ) ;
#29091 = CARTESIAN_POINT ( 'NONE',  ( 72.71132485994280614, 155.0000000000000000, 15.00000000000001243 ) ) ;
#29092 = CARTESIAN_POINT ( 'NONE',  ( -6.139770520408369237, 215.5359834540460042, 96.95113791807857240 ) ) ;
#29093 = CARTESIAN_POINT ( 'NONE',  ( 0.05014649552810506589, 217.5146222423826714, 67.25113791807856956 ) ) ;
#29094 = CARTESIAN_POINT ( 'NONE',  ( -0.05014649552828442242, 219.6175466908591716, 24.24886208192144110 ) ) ;
#29095 = CARTESIAN_POINT ( 'NONE',  ( -10.01549611932659545, 210.2015048109875011, 38.64886208192142902 ) ) ;
#29096 = CARTESIAN_POINT ( 'NONE',  ( 79.99999999453763166, 155.0000000000000000, -14.50000000000000711 ) ) ;
#29097 = CARTESIAN_POINT ( 'NONE',  ( -9.680171189290831535, 214.0920067884431148, 78.80113791807858092 ) ) ;
#29098 = CARTESIAN_POINT ( 'NONE',  ( -2.517493886308901807, 199.4062855549015012, 83.90113791807856103 ) ) ;
#29099 = EDGE_CURVE ( 'NONE', #7343, #9970, #3893, .T. ) ;
#29100 = CARTESIAN_POINT ( 'NONE',  ( -6.139770520408224463, 198.4640165459539389, 50.04886208192143471 ) ) ;
#29101 = FACE_OUTER_BOUND ( 'NONE', #28481, .T. ) ;
#29102 = ORIENTED_EDGE ( 'NONE', *, *, #33659, .F. ) ;
#29103 = CARTESIAN_POINT ( 'NONE',  ( 7.456977232089471386, 196.8216656703012006, 49.44886208192144039 ) ) ;
#29104 = ORIENTED_EDGE ( 'NONE', *, *, #22427, .T. ) ;
#29105 = ORIENTED_EDGE ( 'NONE', *, *, #29742, .T. ) ;
#29106 = EDGE_CURVE ( 'NONE', #29143, #18299, #23900, .T. ) ;
#29107 = CARTESIAN_POINT ( 'NONE',  ( 77.77499999726880731, 169.8198683612136222, -4.815267126137197984 ) ) ;
#29108 = DIRECTION ( 'NONE',  ( 1.000000000000000000, 0.000000000000000000, 0.000000000000000000 ) ) ;
#29109 = CARTESIAN_POINT ( 'NONE',  ( 4.984841277089725686, 213.7757310962907411, 55.55113791807858092 ) ) ;
#29110 = CYLINDRICAL_SURFACE ( 'NONE', #27066, 24.99999999999999289 ) ;
#29111 = CARTESIAN_POINT ( 'NONE',  ( -10.01549611932659722, 210.2015048109875011, 29.64886208192143968 ) ) ;
#29112 = CARTESIAN_POINT ( 'NONE',  ( 65.07499999726881867, 141.7447067706911810, -9.630534252274387086 ) ) ;
#29113 = ORIENTED_EDGE ( 'NONE', *, *, #29775, .F. ) ;
#29114 = CARTESIAN_POINT ( 'NONE',  ( 67.88867513459483405, 150.1262045565062238, 14.99999999999987388 ) ) ;
#29115 = EDGE_CURVE ( 'NONE', #2428, #16283, #4233, .T. ) ;
#29116 = CARTESIAN_POINT ( 'NONE',  ( 43.68867513459482410, 159.8737954434936057, 15.00000000000001421 ) ) ;
#29117 = CARTESIAN_POINT ( 'NONE',  ( -6.500168698208244500, 211.6636982574061676, 8.798862081921434708 ) ) ;
#29118 = CARTESIAN_POINT ( 'NONE',  ( 10.00000000000000711, 206.9523078486586201, 53.00113791807857666 ) ) ;
#29119 = CARTESIAN_POINT ( 'NONE',  ( 80.51132485994280330, 163.8167787843871110, 12.13525491562421621 ) ) ;
#29120 = PRODUCT_DEFINITION_SHAPE ( 'NONE', 'NONE',  #33722 ) ;
#29121 = CARTESIAN_POINT ( 'NONE',  ( -10.00000000000000711, 207.0476921513413515, 33.50113791807856956 ) ) ;
#29122 = CARTESIAN_POINT ( 'NONE',  ( 83.47499999726881015, 160.0630714827496206, -15.58253175000000823 ) ) ;
#29123 = ITEM_DEFINED_TRANSFORMATION ( 'NONE', 'NONE', #29507,  #2404 ) ;
#29124 = CARTESIAN_POINT ( 'NONE',  ( -7.984503880673422316, 204.3529502787951628, 89.34886208192143897 ) ) ;
#29125 = CARTESIAN_POINT ( 'NONE',  ( 39.92499999726881299, 164.1591823560292198, 12.60653300113718167 ) ) ;
#29126 = CYLINDRICAL_SURFACE ( 'NONE', #13075, 2.149999999999984812 ) ;
#29127 = CARTESIAN_POINT ( 'NONE',  ( 0.05014649552807549926, 219.6175466908591716, 13.25113791807856423 ) ) ;
#29128 = CARTESIAN_POINT ( 'NONE',  ( 82.18867513459483121, 140.7341522555726669, 4.635254915624211769 ) ) ;
#29129 = CARTESIAN_POINT ( 'NONE',  ( 54.57499999726881157, 145.8408176439707802, 12.60653300113718345 ) ) ;
#29130 = ADVANCED_FACE ( 'NONE', ( #29803 ), #6464, .F. ) ;
#29131 = CARTESIAN_POINT ( 'NONE',  ( 8.062137200540920645, 201.0835637161417822, 62.30113791807858092 ) ) ;
#29132 = CARTESIAN_POINT ( 'NONE',  ( -10.00000000000000711, 207.0476921513413515, 30.50113791807856600 ) ) ;
#29133 = CYLINDRICAL_SURFACE ( 'NONE', #24103, 4.199999999999988631 ) ;
#29134 = DIRECTION ( 'NONE',  ( 0.000000000000000000, -0.9988620819214357738, -0.04769215134144155765 ) ) ;
#29135 = CARTESIAN_POINT ( 'NONE',  ( -3.044812012439970683, 197.4746971517856196, 4.898862081921434353 ) ) ;
#29136 = CARTESIAN_POINT ( 'NONE',  ( 62.69999999453762740, 167.3344367211045096, 8.961492836873468093 ) ) ;
#29137 = ORIENTED_EDGE ( 'NONE', *, *, #27513, .T. ) ;
#29138 = CARTESIAN_POINT ( 'NONE',  ( -12.00000000000000711, 207.0476921513413515, 39.50113791807856245 ) ) ;
#29139 = ADVANCED_FACE ( 'NONE', ( #27406 ), #22780, .T. ) ;
#29140 = CARTESIAN_POINT ( 'NONE',  ( 125.0000000000000000, -24.99999999999995737, 20.00000000000000000 ) ) ;
#29141 = CARTESIAN_POINT ( 'NONE',  ( -10.01549611932659722, 210.2015048109875011, 20.64886208192143613 ) ) ;
#29142 = CARTESIAN_POINT ( 'NONE',  ( 71.71132485994280614, 155.0000000000000000, -15.00000000000002487 ) ) ;
#29143 = VERTEX_POINT ( 'NONE', #20424 ) ;
#29144 = CARTESIAN_POINT ( 'NONE',  ( 8.118202686958039038, 212.8392687619912635, 76.70113791807857240 ) ) ;
#29145 = ORIENTED_EDGE ( 'NONE', *, *, #29910, .F. ) ;
#29146 = DIRECTION ( 'NONE',  ( 0.000000000000000000, 0.000000000000000000, -1.000000000000000000 ) ) ;
#29147 = DIRECTION ( 'NONE',  ( 1.000000000000000000, 0.000000000000000000, 0.000000000000000000 ) ) ;
#29148 = VERTEX_POINT ( 'NONE', #28081 ) ;
#29149 = CARTESIAN_POINT ( 'NONE',  ( 0.05014649552807626948, 215.4116977939061144, 10.25113791807856600 ) ) ;
#29150 = DIRECTION ( 'NONE',  ( 1.000000000000000000, 0.000000000000000000, 0.000000000000000000 ) ) ;
#29151 = CARTESIAN_POINT ( 'NONE',  ( 11.98450388067341876, 210.9467285061363953, 102.8488620819214390 ) ) ;
#29152 = CARTESIAN_POINT ( 'NONE',  ( 46.77499999726881441, 140.1801316387863778, 4.815267126137185549 ) ) ;
#29153 = VERTEX_POINT ( 'NONE', #33536 ) ;
#29154 = CARTESIAN_POINT ( 'NONE',  ( 50.42499999726880588, 141.7447067706911810, 9.630534252274376428 ) ) ;
#29155 = FACE_OUTER_BOUND ( 'NONE', #4431, .T. ) ;
#29156 = CARTESIAN_POINT ( 'NONE',  ( 61.08867513459484400, 167.7597621252805880, -9.270509831248443078 ) ) ;
#29157 = CARTESIAN_POINT ( 'NONE',  ( -10.01549611932659722, 210.2015048109875011, 80.64886208192143613 ) ) ;
#29158 = CARTESIAN_POINT ( 'NONE',  ( 54.97499999726881015, 140.1801316387863778, -4.815267126137194431 ) ) ;
#29159 = CARTESIAN_POINT ( 'NONE',  ( 10.01549611932653860, 210.2015048109876716, 19.85113791807856387 ) ) ;
#29160 = CARTESIAN_POINT ( 'NONE',  ( 7.500000000000000000, 4.330127018922190096, -7.422398894150032511 ) ) ;
#29161 = EDGE_CURVE ( 'NONE', #18299, #23539, #9654, .T. ) ;
#29162 = ADVANCED_FACE ( 'NONE', ( #15638 ), #31321, .F. ) ;
#29163 = CARTESIAN_POINT ( 'NONE',  ( -11.98450388067341876, 203.0532714938636047, 77.34886208192143897 ) ) ;
#29164 = CIRCLE ( 'NONE', #14468, 2.500000000000000000 ) ;
#29165 = CARTESIAN_POINT ( 'NONE',  ( 72.80000000000001137, 167.3344367211045096, -8.961492836873482304 ) ) ;
#29166 = LINE ( 'NONE', #26604, #13271 ) ;
#29167 = DIRECTION ( 'NONE',  ( -1.000000000000000000, -0.000000000000000000, -0.000000000000000000 ) ) ;
#29168 = CARTESIAN_POINT ( 'NONE',  ( 6.220909254589536808, 215.4770327129947702, 85.55113791807858092 ) ) ;
#29169 = CARTESIAN_POINT ( 'NONE',  ( 107.0104235265664556, 155.0000000000000000, 0.000000000000000000 ) ) ;
#29170 = ADVANCED_FACE ( 'NONE', ( #23479 ), #4917, .T. ) ;
#29171 = CARTESIAN_POINT ( 'NONE',  ( 34.97499999726881015, 140.1801316387863778, -4.815267126137194431 ) ) ;
#29172 = PRODUCT_RELATED_PRODUCT_CATEGORY ( 'part', '', ( #1532 ) ) ;
#29173 = EDGE_CURVE ( 'NONE', #28486, #33027, #23148, .T. ) ;
#29174 = CARTESIAN_POINT ( 'NONE',  ( -11.98450388067341876, 203.0532714938636047, 95.34886208192143897 ) ) ;
#29175 = CARTESIAN_POINT ( 'NONE',  ( 79.82499999726881867, 168.2552932293087906, 9.630534252274372875 ) ) ;
#29176 = VERTEX_POINT ( 'NONE', #23316 ) ;
#29177 = CARTESIAN_POINT ( 'NONE',  ( -96.16666666666678509, -63.33333333333321491, 11.66666666666661278 ) ) ;
#29178 = CARTESIAN_POINT ( 'NONE',  ( 40.99999999453763166, 155.0000000000000000, 14.49999999999999467 ) ) ;
#29179 = FACE_OUTER_BOUND ( 'NONE', #1617, .T. ) ;
#29180 = CARTESIAN_POINT ( 'NONE',  ( 3.500000000000004441, -1.692071238847164372, -0.2177329504545181260 ) ) ;
#29181 = ORIENTED_EDGE ( 'NONE', *, *, #4153, .T. ) ;
#29182 = CARTESIAN_POINT ( 'NONE',  ( -3.044812012439970683, 197.4746971517856196, 94.89886208192143613 ) ) ;
#29183 = CARTESIAN_POINT ( 'NONE',  ( -7.456977232089471386, 217.1783343296987709, 29.94886208192143684 ) ) ;
#29184 = DIRECTION ( 'NONE',  ( -0.9945218953682772867, 1.280104479604772081E-17, -0.1045284632676156678 ) ) ;
#29185 = CARTESIAN_POINT ( 'NONE',  ( -3.135527875058821579, 197.5041725223112223, 47.90113791807857524 ) ) ;
#29186 = B_SPLINE_CURVE_WITH_KNOTS ( 'NONE', 3,
 ( #20126, #30520, #22855, #12290, #27962, #7185, #4452, #2075, #33246 ),
 .UNSPECIFIED., .F., .F.,
 ( 4, 2, 1, 2, 4 ),
 ( 0.000000000000000000, 0.002165063509461097064, 0.004330127018922194128, 0.006495190528383290758, 0.008660254037844389990 ),
 .UNSPECIFIED. ) ;
#29187 = EDGE_LOOP ( 'NONE', ( #21343, #21591, #4649, #17971 ) ) ;
#29188 = CARTESIAN_POINT ( 'NONE',  ( 6.220909254589681581, 198.5229672870052582, 103.4488620819214049 ) ) ;
#29189 = CIRCLE ( 'NONE', #3621, 32.10452846326766974 ) ;
#29190 = CLOSED_SHELL ( 'NONE', ( #19453, #2764, #2518, #19590, #5351, #24789, #26566, #15957, #28563, #30222, #7530, #6903, #12843, #18903, #17241, #21055, #26630, #22906, #25630, #30151, #9957, #8107, #7335, #15936, #23523, #11211, #32168, #22274 ) ) ;
#29191 = CARTESIAN_POINT ( 'NONE',  ( -1.452965002680439710, 3.202582148906722992, 2.797749824780954020E-15 ) ) ;
#29192 = ORIENTED_EDGE ( 'NONE', *, *, #11675, .F. ) ;
#29193 = CARTESIAN_POINT ( 'NONE',  ( 4.984841277089891776, 200.2242689037093726, 88.44886208192144750 ) ) ;
#29194 = CARTESIAN_POINT ( 'NONE',  ( -4.984841277089726574, 200.2242689037092305, 27.05113791807857027 ) ) ;
#29195 = DIRECTION ( 'NONE',  ( 1.000000000000000000, 0.000000000000000000, 0.000000000000000000 ) ) ;
#29197 = EDGE_LOOP ( 'NONE', ( #26489, #10631, #23079, #28197 ) ) ;
#29196 = VECTOR ( 'NONE', #10198, 1000.000000000000000 ) ;
#29198 = CARTESIAN_POINT ( 'NONE',  ( 33.72499999726881725, 169.8198683612136222, 4.815267126137181997 ) ) ;
#29199 = CARTESIAN_POINT ( 'NONE',  ( 34.07499999726879736, 168.2552932293087906, 9.630534252274372875 ) ) ;
#29200 = FACE_OUTER_BOUND ( 'NONE', #3943, .T. ) ;
#29201 = CARTESIAN_POINT ( 'NONE',  ( -4.984841277089726574, 200.2242689037092305, 102.0511379180785809 ) ) ;
#29202 = DIRECTION ( 'NONE',  ( 0.000000000000000000, -0.07223725545290975159, -0.9973874768236420385 ) ) ;
#29203 = CARTESIAN_POINT ( 'NONE',  ( 54.90000000000000568, 168.7903194862797420, -4.480746418436745593 ) ) ;
#29204 = CARTESIAN_POINT ( 'NONE',  ( 0.05014649552828262524, 198.5883022060938572, 70.74886208192144466 ) ) ;
#29205 = CARTESIAN_POINT ( 'NONE',  ( 77.18867513459481700, 169.2658477444273331, -4.635254915624224203 ) ) ;
#29206 = AXIS2_PLACEMENT_3D ( 'NONE', #20938, #31330, #5916 ) ;
#29207 = CARTESIAN_POINT ( 'NONE',  ( 55.92499999726881299, 164.1591823560292198, 12.60653300113718167 ) ) ;
#29208 = VECTOR ( 'NONE', #27100, 1000.000000000000000 ) ;
#29209 = CARTESIAN_POINT ( 'NONE',  ( 9.984503880673473830, 203.7031108863295401, 8.151137918078566358 ) ) ;
#29210 = CARTESIAN_POINT ( 'NONE',  ( -6.815701034932152069, -1.328907527188669668, -6.169383458210047522 ) ) ;
#29211 = CARTESIAN_POINT ( 'NONE',  ( 60.62499999726880162, 138.6155565068815747, -3.929120461958505118E-15 ) ) ;
#29212 = CARTESIAN_POINT ( 'NONE',  ( 75.67499999726881299, 168.2552932293087906, -9.630534252274385310 ) ) ;
#29213 = CARTESIAN_POINT ( 'NONE',  ( -3.662846001190052991, 218.4274158808045740, 73.10113791807857808 ) ) ;
#29214 = CARTESIAN_POINT ( 'NONE',  ( 0.3999999999999975797, 7.960204194457795477E-16, -6.500000000000000000 ) ) ;
#29215 = CARTESIAN_POINT ( 'NONE',  ( -6.139770520408368348, 215.5359834540460042, 99.95113791807855819 ) ) ;
#29216 = CARTESIAN_POINT ( 'NONE',  ( -27.50000000000000000, -15.87713240271473225, -18.00000000000000000 ) ) ;
#29217 = VERTEX_POINT ( 'NONE', #15134 ) ;
#29218 = CARTESIAN_POINT ( 'NONE',  ( -12.01549611932659722, 210.8513442034533227, 101.6488620819214361 ) ) ;
#29219 = CARTESIAN_POINT ( 'NONE',  ( 12.01549611932659367, 203.1486557965466773, 64.14886208192143613 ) ) ;
#29220 = CARTESIAN_POINT ( 'NONE',  ( 8.118202686958138514, 201.1607312380088501, 67.29886208192144181 ) ) ;
#29221 = CARTESIAN_POINT ( 'NONE',  ( -0.05014649552807705357, 194.3824533091408000, 101.7511379180785696 ) ) ;
#29222 = CARTESIAN_POINT ( 'NONE',  ( -2.352990130084580066E-16, 8.660254037844390851, -10.00000000000000000 ) ) ;
#29223 = CARTESIAN_POINT ( 'NONE',  ( 0.05014649552810505201, 217.5146222423826714, 25.25113791807856245 ) ) ;
#29224 = CARTESIAN_POINT ( 'NONE',  ( -10.00000000000000711, 206.9523078486584495, 83.49886208192143044 ) ) ;
#29225 = ORIENTED_EDGE ( 'NONE', *, *, #22668, .F. ) ;
#29226 = CARTESIAN_POINT ( 'NONE',  ( 8.062137200540920645, 201.0835637161417822, 98.30113791807858092 ) ) ;
#29227 = ORIENTED_EDGE ( 'NONE', *, *, #8681, .T. ) ;
#29228 = SURFACE_STYLE_FILL_AREA ( #11009 ) ;
#29229 = CARTESIAN_POINT ( 'NONE',  ( 4.903702542908435547, 213.8346818373419751, 57.54886208192142760 ) ) ;
#29230 = VECTOR ( 'NONE', #24880, 1000.000000000000000 ) ;
#29231 = ORIENTED_EDGE ( 'NONE', *, *, #27511, .T. ) ;
#29232 = AXIS2_PLACEMENT_3D ( 'NONE', #7447, #27874, #4551 ) ;
#29233 = CARTESIAN_POINT ( 'NONE',  ( 77.32499999726881867, 164.1591823560292198, -12.60653300113719766 ) ) ;
#29234 = ORIENTED_EDGE ( 'NONE', *, *, #12713, .T. ) ;
#29235 = CARTESIAN_POINT ( 'NONE',  ( 6.500000000000000888, 4.077976443323007238, -6.122137821720842865 ) ) ;
#29236 = VECTOR ( 'NONE', #14951, 1000.000000000000000 ) ;
#29237 = VECTOR ( 'NONE', #9647, 1000.000000000000000 ) ;
#29238 = CARTESIAN_POINT ( 'NONE',  ( 68.32499999726881867, 145.8408176439707802, 12.60653300113718345 ) ) ;
#29239 = CARTESIAN_POINT ( 'NONE',  ( -8.000000000000008882, 207.0476921513413515, 69.50113791807856956 ) ) ;
#29240 = PLANE ( 'NONE',  #27096 ) ;
#29241 = CIRCLE ( 'NONE', #10750, 112.0000000000000711 ) ;
#29242 = DIRECTION ( 'NONE',  ( 1.000000000000000000, 0.000000000000000000, 0.000000000000000000 ) ) ;
#29243 = SURFACE_STYLE_USAGE ( .BOTH. , #28586 ) ;
#29244 = CARTESIAN_POINT ( 'NONE',  ( 35.50000000000000711, 155.0000000000000000, 14.49999999999999467 ) ) ;
#29245 = CARTESIAN_POINT ( 'NONE',  ( 8.000000000000008882, 207.0476921513415220, 39.99886208192145176 ) ) ;
#29246 = CARTESIAN_POINT ( 'NONE',  ( -3.044812012440131443, 216.5253028482142952, 82.10113791807857808 ) ) ;
#29247 = CARTESIAN_POINT ( 'NONE',  ( 3.044812012440130555, 197.4746971517856764, 65.60113791807857808 ) ) ;
#29248 = FACE_BOUND ( 'NONE', #8338, .T. ) ;
#29249 = CARTESIAN_POINT ( 'NONE',  ( -4.984841277089726574, 200.2242689037092305, 24.05113791807857027 ) ) ;
#29250 = CARTESIAN_POINT ( 'NONE',  ( 129.5873785388598947, -2.643999646947195359, 35.00001200000000523 ) ) ;
#29251 = DIRECTION ( 'NONE',  ( 0.000000000000000000, -0.4999999999999995004, 0.8660254037844389297 ) ) ;
#29252 = CARTESIAN_POINT ( 'NONE',  ( 46.72499999726881015, 140.1801316387863778, -4.815267126137194431 ) ) ;
#29253 = CARTESIAN_POINT ( 'NONE',  ( 7.456977232089302632, 217.1783343296989131, 49.55113791807856671 ) ) ;
#29254 = CARTESIAN_POINT ( 'NONE',  ( 7.499999999997997158, -3.157198044624895061, -7.642795354507847527 ) ) ;
#29255 = CARTESIAN_POINT ( 'NONE',  ( -8.118202686958039038, 201.1607312380087080, 99.20113791807858661 ) ) ;
#29256 = EDGE_CURVE ( 'NONE', #23340, #12431, #30995, .T. ) ;
#29257 = CARTESIAN_POINT ( 'NONE',  ( 6.220909254589536808, 215.4770327129947987, 70.55113791807856671 ) ) ;
#29258 = AXIS2_PLACEMENT_3D ( 'NONE', #25119, #20981, #4511 ) ;
#29259 = CARTESIAN_POINT ( 'NONE',  ( -9.736236675708031640, 214.0148392665760753, 32.79886208192143471 ) ) ;
#29260 = CARTESIAN_POINT ( 'NONE',  ( -10.01549611932659545, 210.2015048109875011, 35.64886208192142902 ) ) ;
#29261 = CARTESIAN_POINT ( 'NONE',  ( 77.09999999453762598, 150.2886644046228639, 14.49999999999999645 ) ) ;
#29262 = CARTESIAN_POINT ( 'NONE',  ( 3.662846001190051659, 195.5725841191953691, 74.60113791807854966 ) ) ;
#29263 = CARTESIAN_POINT ( 'NONE',  ( -7.984503880673488041, 209.6470497212046098, 90.65113791807857524 ) ) ;
#29264 = CARTESIAN_POINT ( 'NONE',  ( -8.062137200540822946, 201.0835637161416400, 47.19886208192143329 ) ) ;
#29265 = CARTESIAN_POINT ( 'NONE',  ( 49.48867513459482126, 167.7597621252805880, 9.270509831248428867 ) ) ;
#29266 = CIRCLE ( 'NONE', #27631, 3.047499999999999876 ) ;
#29267 = ORIENTED_EDGE ( 'NONE', *, *, #28082, .F. ) ;
#29268 = CARTESIAN_POINT ( 'NONE',  ( -7.375838497908014268, 196.7627149292498530, 62.04886208192144181 ) ) ;
#29269 = ORIENTED_EDGE ( 'NONE', *, *, #2334, .T. ) ;
#29270 = CARTESIAN_POINT ( 'NONE',  ( 8.000000000000008882, 207.0476921513415220, 33.99886208192143755 ) ) ;
#29271 = ORIENTED_EDGE ( 'NONE', *, *, #15640, .T. ) ;
#29272 = CARTESIAN_POINT ( 'NONE',  ( 74.17499999726881299, 164.1591823560292198, 12.60653300113718167 ) ) ;
#29273 = CARTESIAN_POINT ( 'NONE',  ( 53.51132485994281041, 146.1832212156128890, -12.13525491562423042 ) ) ;
#29274 = DIRECTION ( 'NONE',  ( -1.000000000000000000, -0.000000000000000000, 0.000000000000000000 ) ) ;
#29275 = CARTESIAN_POINT ( 'NONE',  ( -2.517493886308901807, 199.4062855549015012, 53.90113791807858235 ) ) ;
#29276 = AXIS2_PLACEMENT_3D ( 'NONE', #5686, #10486, #18974 ) ;
#29277 = DIRECTION ( 'NONE',  ( 1.000000000000000000, -0.000000000000000000, -0.000000000000000000 ) ) ;
#29278 = AXIS2_PLACEMENT_3D ( 'NONE', #13764, #30280, #14267 ) ;
#29279 = CARTESIAN_POINT ( 'NONE',  ( 3.135527875058981895, 197.5041725223112792, 28.59886208192143897 ) ) ;
#29280 = CARTESIAN_POINT ( 'NONE',  ( 69.97499999726881015, 169.8198683612136222, 4.815267126137181997 ) ) ;
#29281 = VERTEX_POINT ( 'NONE', #7987 ) ;
#29282 = CARTESIAN_POINT ( 'NONE',  ( 40.88867513459481984, 159.8737954434936057, -15.00000000000002665 ) ) ;
#29283 = CARTESIAN_POINT ( 'NONE',  ( 111.1125082318798007, 155.0000000000000000, 32.00000000000002842 ) ) ;
#29284 = CARTESIAN_POINT ( 'NONE',  ( -4.903702542908436435, 200.1653181626580249, 17.04886208192143471 ) ) ;
#29285 = CARTESIAN_POINT ( 'NONE',  ( -3.135527875058821579, 197.5041725223112223, 53.90113791807857524 ) ) ;
#29286 = CARTESIAN_POINT ( 'NONE',  ( 83.38867513459483405, 169.2658477444273331, 4.635254915624208216 ) ) ;
#29287 = CARTESIAN_POINT ( 'NONE',  ( 6.139770520408368348, 198.4640165459539674, 32.45113791807856529 ) ) ;
#29288 = CARTESIAN_POINT ( 'NONE',  ( 86.17499999726881299, 164.1591823560292198, 12.60653300113718167 ) ) ;
#29289 = VECTOR ( 'NONE', #28763, 1000.000000000000000 ) ;
#29290 = APPLICATION_PROTOCOL_DEFINITION ( 'draft international standard', 'automotive_design', 1998, #2680 ) ;
#29291 = CARTESIAN_POINT ( 'NONE',  ( 6.500168698208244500, 202.3363017425938324, 97.29886208192142760 ) ) ;
#29292 = CARTESIAN_POINT ( 'NONE',  ( 36.62499999726881583, 138.6155565068815463, -3.929120461958505118E-15 ) ) ;
#29293 = CARTESIAN_POINT ( 'NONE',  ( 35.71132485994280614, 155.0000000000000000, -15.00000000000002487 ) ) ;
#29294 = CARTESIAN_POINT ( 'NONE',  ( 49.78867513459482552, 155.0000000000000000, 15.00000000000001243 ) ) ;
#29295 = CARTESIAN_POINT ( 'NONE',  ( -12.01549611932652972, 203.1486557965464499, 18.35113791807856387 ) ) ;
#29296 = LINE ( 'NONE', #24014, #18405 ) ;
#29297 = CARTESIAN_POINT ( 'NONE',  ( 54.67499999726881299, 141.7447067706911810, 9.630534252274376428 ) ) ;
#29298 = CARTESIAN_POINT ( 'NONE',  ( 6.139770520408368348, 198.4640165459539674, 65.45113791807857240 ) ) ;
#29299 = ADVANCED_FACE ( 'NONE', ( #26042 ), #2367, .F. ) ;
#29300 = CARTESIAN_POINT ( 'NONE',  ( 3.044812012440130555, 197.4746971517856764, 35.60113791807857098 ) ) ;
#29301 = DIRECTION ( 'NONE',  ( 0.000000000000000000, 0.000000000000000000, 1.000000000000000000 ) ) ;
#29302 = FACE_OUTER_BOUND ( 'NONE', #21133, .T. ) ;
#29303 = CARTESIAN_POINT ( 'NONE',  ( -8.062137200540822946, 201.0835637161416400, 14.19886208192143684 ) ) ;
#29304 = CARTESIAN_POINT ( 'NONE',  ( 57.59999999453763309, 141.2096805137202580, -4.480746418436742040 ) ) ;
#29305 = ORIENTED_EDGE ( 'NONE', *, *, #4127, .T. ) ;
#29306 = CARTESIAN_POINT ( 'NONE',  ( -9.736236675707914401, 199.9851607334237542, 48.20113791807858661 ) ) ;
#29307 = AXIS2_PLACEMENT_3D ( 'NONE', #22029, #11804, #3627 ) ;
#29308 = FACE_OUTER_BOUND ( 'NONE', #23023, .T. ) ;
#29309 = CARTESIAN_POINT ( 'NONE',  ( 9.984503880673420539, 210.2968891136705167, 18.84886208192143542 ) ) ;
#29310 = AXIS2_PLACEMENT_3D ( 'NONE', #18681, #29069, #5721 ) ;
#29311 = CARTESIAN_POINT ( 'NONE',  ( 36.78867513459482552, 155.0000000000000000, -15.00000000000002487 ) ) ;
#29312 = ORIENTED_EDGE ( 'NONE', *, *, #12524, .T. ) ;
#29313 = ADVANCED_FACE ( 'NONE', ( #7652 ), #5420, .T. ) ;
#29314 = AXIS2_PLACEMENT_3D ( 'NONE', #19607, #13648, #3593 ) ;
#29315 = CARTESIAN_POINT ( 'NONE',  ( -9.984503880673473830, 210.2968891136704315, 78.65113791807854682 ) ) ;
#29316 = EDGE_LOOP ( 'NONE', ( #2963, #3002, #25717, #3619 ) ) ;
#29317 = AXIS2_PLACEMENT_3D ( 'NONE', #26090, #31040, #197 ) ;
#29318 = CYLINDRICAL_SURFACE ( 'NONE', #33076, 5.200000000000009948 ) ;
#29319 = LINE ( 'NONE', #24031, #9434 ) ;
#29320 = VERTEX_POINT ( 'NONE', #17865 ) ;
#29321 = CARTESIAN_POINT ( 'NONE',  ( 8.000000000000008882, 206.9523078486586485, 20.00113791807856956 ) ) ;
#29322 = EDGE_CURVE ( 'NONE', #16155, #31786, #30649, .T. ) ;
#29323 = DIRECTION ( 'NONE',  ( 1.000000000000000000, 0.000000000000000000, 0.000000000000000000 ) ) ;
#29324 = CARTESIAN_POINT ( 'NONE',  ( 3.135527875058981895, 197.5041725223112792, 4.598862081921434530 ) ) ;
#29325 = CARTESIAN_POINT ( 'NONE',  ( 47.57499999726881867, 164.1591823560292198, -12.60653300113719766 ) ) ;
#29326 = VERTEX_POINT ( 'NONE', #18371 ) ;
#29327 = CARTESIAN_POINT ( 'NONE',  ( 54.62499999726880162, 138.6155565068815463, -3.929120461958505118E-15 ) ) ;
#29328 = DIRECTION ( 'NONE',  ( -1.000000000000000000, -1.804112415015879378E-16, -0.000000000000000000 ) ) ;
#29329 = CARTESIAN_POINT ( 'NONE',  ( 61.38867513459481984, 169.2658477444273331, 4.635254915624208216 ) ) ;
#29330 = DIRECTION ( 'NONE',  ( -0.000000000000000000, 1.000000000000000000, 1.224646799147353207E-16 ) ) ;
#29331 = AXIS2_PLACEMENT_3D ( 'NONE', #4328, #16764, #14712 ) ;
#29332 = CARTESIAN_POINT ( 'NONE',  ( 3.135527875058981895, 197.5041725223112792, 91.59886208192143897 ) ) ;
#29333 = EDGE_CURVE ( 'NONE', #8954, #15366, #10380, .T. ) ;
#29334 = CARTESIAN_POINT ( 'NONE',  ( 51.47499999726881725, 160.0630714827496206, -15.58253175000000823 ) ) ;
#29335 = CARTESIAN_POINT ( 'NONE',  ( 10.01549611932653860, 210.2015048109876716, 22.85113791807856742 ) ) ;
#29336 = LINE ( 'NONE', #32382, #30097 ) ;
#29337 = CARTESIAN_POINT ( 'NONE',  ( 12.01549611932659367, 203.1486557965466773, 76.14886208192143613 ) ) ;
#29338 = CONICAL_SURFACE ( 'NONE', #32587, 27.50000000000000355, 1.047197551196595411 ) ;
#29339 = CARTESIAN_POINT ( 'NONE',  ( 73.50000000000001421, 155.0000000000000000, 14.49999999999999467 ) ) ;
#29340 = DIRECTION ( 'NONE',  ( -0.000000000000000000, -0.000000000000000000, -1.000000000000000000 ) ) ;
#29341 = DIRECTION ( 'NONE',  ( 0.000000000000000000, 0.000000000000000000, -1.000000000000000000 ) ) ;
#29342 = CARTESIAN_POINT ( 'NONE',  ( 8.062137200540920645, 201.0835637161417822, 98.30113791807858092 ) ) ;
#29343 = CARTESIAN_POINT ( 'NONE',  ( 32.50000000000000000, 155.0000000000000000, -6.938893903907228378E-15 ) ) ;
#29344 = CARTESIAN_POINT ( 'NONE',  ( 38.77499999726881441, 140.1801316387863778, 4.815267126137185549 ) ) ;
#29345 = CARTESIAN_POINT ( 'NONE',  ( -9.984503880673473830, 210.2968891136704315, 33.65113791807856813 ) ) ;
#29346 = CARTESIAN_POINT ( 'NONE',  ( 74.92499999726881299, 145.8408176439707802, -12.60653300113719588 ) ) ;
#29347 = ORIENTED_EDGE ( 'NONE', *, *, #32690, .T. ) ;
#29348 = CARTESIAN_POINT ( 'NONE',  ( 51.78867513459482552, 155.0000000000000000, 15.00000000000001243 ) ) ;
#29349 = CARTESIAN_POINT ( 'NONE',  ( 40.59999999453763309, 168.7903194862797420, 4.480746418436729606 ) ) ;
#29350 = CARTESIAN_POINT ( 'NONE',  ( 9.680171189290831535, 199.9079932115568852, 23.30113791807857027 ) ) ;
#29351 = CARTESIAN_POINT ( 'NONE',  ( -125.0000000000000000, 0.000000000000000000, 35.00000000000000000 ) ) ;
#29352 = CARTESIAN_POINT ( 'NONE',  ( -1.013163106016700565, -8.075304045852661261, -7.231838333420565590 ) ) ;
#29353 = ORIENTED_EDGE ( 'NONE', *, *, #5342, .T. ) ;
#29354 = CARTESIAN_POINT ( 'NONE',  ( -0.05014649552828402690, 217.5146222423826714, 93.24886208192143044 ) ) ;
#29355 = CARTESIAN_POINT ( 'NONE',  ( 12.00000000000000711, 207.0476921513415220, 33.99886208192143044 ) ) ;
#29356 = CARTESIAN_POINT ( 'NONE',  ( -7.894787914004607998, -1.230850257101226302E-13, -7.591390474663425536 ) ) ;
#29357 = CIRCLE ( 'NONE', #17939, 40.00000000000000711 ) ;
#29358 = CARTESIAN_POINT ( 'NONE',  ( 9.984503880673470277, 203.7031108863295401, 47.15113791807857524 ) ) ;
#29359 = ORIENTED_EDGE ( 'NONE', *, *, #30996, .T. ) ;
#29360 = CARTESIAN_POINT ( 'NONE',  ( -4.903702542908436435, 200.1653181626580249, 11.04886208192143648 ) ) ;
#29361 = ADVANCED_FACE ( 'NONE', ( #17694, #25871, #15805, #2198, #2537, #307, #7317, #20753, #12920, #22973 ), #33372, .T. ) ;
#29362 = EDGE_CURVE ( 'NONE', #25118, #860, #3172, .T. ) ;
#29363 = CARTESIAN_POINT ( 'NONE',  ( 50.48867513459482836, 142.2402378747194405, -9.270509831248439525 ) ) ;
#29364 = VERTEX_POINT ( 'NONE', #29091 ) ;
#29365 = CARTESIAN_POINT ( 'NONE',  ( -7.984503880673422316, 204.3529502787951628, 101.3488620819214390 ) ) ;
#29366 = ADVANCED_FACE ( 'NONE', ( #21575 ), #33113, .T. ) ;
#29367 = CARTESIAN_POINT ( 'NONE',  ( -8.015496119326531499, 204.4483345814780364, 39.35113791807857098 ) ) ;
#29368 = DIRECTION ( 'NONE',  ( 0.000000000000000000, 0.7071067811865540120, 0.7071067811865411334 ) ) ;
#29369 = ORIENTED_EDGE ( 'NONE', *, *, #24714, .T. ) ;
#29370 = FACE_OUTER_BOUND ( 'NONE', #18438, .T. ) ;
#29371 = CARTESIAN_POINT ( 'NONE',  ( -9.984503880673420539, 203.7031108863293980, 53.34886208192143897 ) ) ;
#29372 = EDGE_CURVE ( 'NONE', #15657, #6774, #26555, .T. ) ;
#29373 = CARTESIAN_POINT ( 'NONE',  ( 35.07499999726881157, 141.7447067706911810, -9.630534252274385310 ) ) ;
#29374 = CARTESIAN_POINT ( 'NONE',  ( 4.984841277089725686, 213.7757310962907411, 94.55113791807855250 ) ) ;
#29375 = DIRECTION ( 'NONE',  ( 0.000000000000000000, -0.7071067811865536790, -0.7071067811865413555 ) ) ;
#29376 = CARTESIAN_POINT ( 'NONE',  ( 52.90000000000000568, 168.7903194862797420, -4.480746418436745593 ) ) ;
#29377 = CARTESIAN_POINT ( 'NONE',  ( 8.000000000000008882, 207.0476921513415220, 72.99886208192144466 ) ) ;
#29378 = LINE ( 'NONE', #8925, #9102 ) ;
#29379 = CARTESIAN_POINT ( 'NONE',  ( 59.92499999726881299, 164.1591823560292198, 12.60653300113718167 ) ) ;
#29380 = CARTESIAN_POINT ( 'NONE',  ( -3.044812012440131443, 216.5253028482142952, 13.10113791807856742 ) ) ;
#29381 = CARTESIAN_POINT ( 'NONE',  ( -6.500000000000000000, -1.336926445777093964, -6.054363369342815382 ) ) ;
#29382 = CARTESIAN_POINT ( 'NONE',  ( 63.72499999726881015, 169.8198683612136222, 4.815267126137181997 ) ) ;
#29383 = CARTESIAN_POINT ( 'NONE',  ( 74.37499999726881583, 155.0000000000000000, 15.58253174999999402 ) ) ;
#29384 = CARTESIAN_POINT ( 'NONE',  ( -0.05014649552807705357, 194.3824533091408000, 74.75113791807856956 ) ) ;
#29385 = CARTESIAN_POINT ( 'NONE',  ( 6.139770520408367460, 198.4640165459539389, 101.4511379180785866 ) ) ;
#29386 = CARTESIAN_POINT ( 'NONE',  ( 84.68867513459485963, 150.1262045565065364, -15.00000000000013323 ) ) ;
#29387 = EDGE_CURVE ( 'NONE', #7672, #31619, #3352, .T. ) ;
#29388 = VERTEX_POINT ( 'NONE', #8799 ) ;
#29389 = CARTESIAN_POINT ( 'NONE',  ( -7.375838497908014268, 196.7627149292498530, 104.0488620819214560 ) ) ;
#29390 = CARTESIAN_POINT ( 'NONE',  ( -0.05014649552828442242, 219.6175466908591716, 57.24886208192144466 ) ) ;
#29391 = CARTESIAN_POINT ( 'NONE',  ( -8.062137200540822946, 201.0835637161416400, 68.19886208192144750 ) ) ;
#29392 = CARTESIAN_POINT ( 'NONE',  ( -0.05014649552828442242, 219.6175466908591716, 6.248862081921433997 ) ) ;
#29393 = CYLINDRICAL_SURFACE ( 'NONE', #14825, 16.00000000000000000 ) ;
#29394 = CARTESIAN_POINT ( 'NONE',  ( -3.044812012440131443, 216.5253028482142952, 22.10113791807856742 ) ) ;
#29395 = CARTESIAN_POINT ( 'NONE',  ( 6.139770520408223575, 215.5359834540460611, 84.54886208192141339 ) ) ;
#29396 = ORIENTED_EDGE ( 'NONE', *, *, #22026, .F. ) ;
#29397 = FACE_OUTER_BOUND ( 'NONE', #11683, .T. ) ;
#29398 = VERTEX_POINT ( 'NONE', #636 ) ;
#29399 = CARTESIAN_POINT ( 'NONE',  ( 60.63708498984762940, 155.0000000000000000, 6.938893903907228378E-15 ) ) ;
#29400 = CARTESIAN_POINT ( 'NONE',  ( -0.05014649552828365914, 215.4116977939061144, 63.24886208192142334 ) ) ;
#29401 = VERTEX_POINT ( 'NONE', #29419 ) ;
#29402 = CARTESIAN_POINT ( 'NONE',  ( 75.22499999726879594, 160.0630714827496206, -15.58253175000000823 ) ) ;
#29403 = ORIENTED_EDGE ( 'NONE', *, *, #11473, .T. ) ;
#29404 = DIRECTION ( 'NONE',  ( 0.000000000000000000, 0.7071067811865442421, -0.7071067811865506814 ) ) ;
#29405 = CARTESIAN_POINT ( 'NONE',  ( 73.12499999726881583, 155.0000000000000000, -15.58253175000000823 ) ) ;
#29406 = CARTESIAN_POINT ( 'NONE',  ( 4.984841277089725686, 213.7757310962907411, 64.55113791807856671 ) ) ;
#29407 = FILL_AREA_STYLE_COLOUR ( '', #16754 ) ;
#29408 =( NAMED_UNIT ( * ) SI_UNIT ( $, .STERADIAN. ) SOLID_ANGLE_UNIT ( ) );
#29409 = CARTESIAN_POINT ( 'NONE',  ( 33.10000000000000142, 168.7903194862797420, 4.480746418436729606 ) ) ;
#29410 = CARTESIAN_POINT ( 'NONE',  ( 4.984841277089891776, 200.2242689037093726, 43.44886208192144039 ) ) ;
#29411 = CARTESIAN_POINT ( 'NONE',  ( -10.01549611932653860, 203.7984951890123284, 81.35113791807857808 ) ) ;
#29412 = CARTESIAN_POINT ( 'NONE',  ( -6.139770520408369237, 215.5359834540460042, 69.95113791807857240 ) ) ;
#29413 = CYLINDRICAL_SURFACE ( 'NONE', #9927, 5.249999999999991118 ) ;
#29414 = CARTESIAN_POINT ( 'NONE',  ( -2.426778023690262742, 214.6231898156240163, 22.10113791807856742 ) ) ;
#29415 = CARTESIAN_POINT ( 'NONE',  ( 2.452879891156805492, 7.244083172395185954, -0.1007566405101774504 ) ) ;
#29416 = CARTESIAN_POINT ( 'NONE',  ( 6.500000000000000000, 3.752776749732563921, -6.064240316920399110 ) ) ;
#29417 = CARTESIAN_POINT ( 'NONE',  ( 47.72499999726881015, 169.8198683612136222, 4.815267126137181997 ) ) ;
#29418 = CARTESIAN_POINT ( 'NONE',  ( 11.98450388067348271, 203.0532714938637753, 44.15113791807856813 ) ) ;
#29419 = CARTESIAN_POINT ( 'NONE',  ( 125.5000000000000000, 261.0000000000000000, -2.149999999999985256 ) ) ;
#29420 = CARTESIAN_POINT ( 'NONE',  ( 0.05014649552810505201, 217.5146222423826714, 97.25113791807854113 ) ) ;
#29422 = CARTESIAN_POINT ( 'NONE',  ( -6.220909254589537696, 198.5229672870051445, 72.05113791807855250 ) ) ;
#29421 = APPLICATION_CONTEXT ( 'automotive_design' ) ;
#29423 = CARTESIAN_POINT ( 'NONE',  ( -11.98450388067341876, 203.0532714938636047, 35.34886208192142476 ) ) ;
#29424 = CARTESIAN_POINT ( 'NONE',  ( 3.135527875058981895, 197.5041725223112792, 34.59886208192143897 ) ) ;
#29425 = CARTESIAN_POINT ( 'NONE',  ( 84.79999999453762882, 163.5228861582408797, 11.73074641843673049 ) ) ;
#29426 = CARTESIAN_POINT ( 'NONE',  ( -12.01549611932652972, 203.1486557965464499, 78.35113791807857808 ) ) ;
#29427 = CARTESIAN_POINT ( 'NONE',  ( -6.444103211791042618, 211.7408657792732356, 99.80113791807858092 ) ) ;
#29428 = CARTESIAN_POINT ( 'NONE',  ( 10.00000000000000711, 207.0476921513415220, 48.99886208192143044 ) ) ;
#29429 = DIRECTION ( 'NONE',  ( 0.000000000000000000, 0.000000000000000000, -1.000000000000000000 ) ) ;
#29430 = ORIENTED_EDGE ( 'NONE', *, *, #16005, .T. ) ;
#29431 = CARTESIAN_POINT ( 'NONE',  ( 12.00000000000000711, 207.0476921513415220, 57.99886208192143044 ) ) ;
#29432 = CIRCLE ( 'NONE', #75, 7.500000000000015099 ) ;
#29433 = ORIENTED_EDGE ( 'NONE', *, *, #31666, .T. ) ;
#29434 = CARTESIAN_POINT ( 'NONE',  ( -6.500168698208244500, 211.6636982574061676, 29.79886208192143826 ) ) ;
#29435 = ORIENTED_EDGE ( 'NONE', *, *, #14578, .F. ) ;
#29436 = CARTESIAN_POINT ( 'NONE',  ( 78.37499999726883004, 155.0000000000000000, 15.58253174999999402 ) ) ;
#29437 = CARTESIAN_POINT ( 'NONE',  ( 108.1100194822685836, 155.0000000000000000, -13.00000000000003908 ) ) ;
#29438 = DIRECTION ( 'NONE',  ( 0.000000000000000000, 0.7071067811865506814, 0.7071067811865442421 ) ) ;
#29439 = CARTESIAN_POINT ( 'NONE',  ( -4.903702542908602524, 213.8346818373418898, 51.95113791807857240 ) ) ;
#29440 = CARTESIAN_POINT ( 'NONE',  ( 4.000000000000000000, 2.639212418033074492, -1.523750000000004157 ) ) ;
#29441 = EDGE_CURVE ( 'NONE', #17245, #24797, #3688, .T. ) ;
#29442 = CARTESIAN_POINT ( 'NONE',  ( 10.01549611932659545, 203.7984951890123853, 34.14886208192143613 ) ) ;
#29443 = CARTESIAN_POINT ( 'NONE',  ( 71.77499999726882152, 169.8198683612136222, -4.815267126137197984 ) ) ;
#29444 = VERTEX_POINT ( 'NONE', #5906 ) ;
#29445 = CARTESIAN_POINT ( 'NONE',  ( 127.5000000000000000, 78.52640161467553526, 73.43303922622362734 ) ) ;
#29446 = CARTESIAN_POINT ( 'NONE',  ( 5.541103744621880989E-15, 31.75426480542943608, -18.00000000000000000 ) ) ;
#29447 = DIRECTION ( 'NONE',  ( -0.9945218953682772867, 0.000000000000000000, 0.1045284632676156678 ) ) ;
#29448 = CARTESIAN_POINT ( 'NONE',  ( -8.000000000000008882, 206.9523078486584780, 17.49886208192143400 ) ) ;
#29449 = CARTESIAN_POINT ( 'NONE',  ( 9.984503880673470277, 203.7031108863295401, 56.15113791807856103 ) ) ;
#29450 = CARTESIAN_POINT ( 'NONE',  ( 82.78867513459482552, 155.0000000000000000, -15.00000000000002487 ) ) ;
#29451 = CARTESIAN_POINT ( 'NONE',  ( -9.984503880673473830, 210.2968891136704315, 33.65113791807856813 ) ) ;
#29452 = CARTESIAN_POINT ( 'NONE',  ( 83.67499999726884141, 168.2552932293087906, -9.630534252274385310 ) ) ;
#29453 = AXIS2_PLACEMENT_3D ( 'NONE', #22003, #31721, #16716 ) ;
#29454 = CARTESIAN_POINT ( 'NONE',  ( -2.517493886309087880, 214.5937144450984135, 102.0988620819214532 ) ) ;
#29455 = CARTESIAN_POINT ( 'NONE',  ( 39.52499999726881441, 169.8198683612136222, -4.815267126137197984 ) ) ;
#29456 = CARTESIAN_POINT ( 'NONE',  ( -64.50000000000000000, 0.000000000000000000, -20.00000000000000000 ) ) ;
#29457 = FACE_OUTER_BOUND ( 'NONE', #10851, .T. ) ;
#29458 = CARTESIAN_POINT ( 'NONE',  ( -7.375838497908182134, 217.2372850707499765, 21.95113791807856884 ) ) ;
#29459 = CARTESIAN_POINT ( 'NONE',  ( 7.169303301815196150, -4.521054846639319003, -7.349897473155491134 ) ) ;
#29460 = CARTESIAN_POINT ( 'NONE',  ( 63.37499999726880873, 155.0000000000000000, -15.58253175000000823 ) ) ;
#29461 = CARTESIAN_POINT ( 'NONE',  ( 3.044812012440130555, 197.4746971517856764, 65.60113791807857808 ) ) ;
#29462 = CARTESIAN_POINT ( 'NONE',  ( 6.220909254589536808, 215.4770327129947987, 37.55113791807856671 ) ) ;
#29463 = DIRECTION ( 'NONE',  ( 1.000000000000000000, 0.000000000000000000, 0.000000000000000000 ) ) ;
#29464 = CARTESIAN_POINT ( 'NONE',  ( -7.499999999999999112, 1.443375672974061219, -7.063244554130000630 ) ) ;
#29465 = CARTESIAN_POINT ( 'NONE',  ( -11.98450388067341876, 203.0532714938636047, 5.348862081921434530 ) ) ;
#29466 = CARTESIAN_POINT ( 'NONE',  ( 8.062137200540822946, 212.9164362838583315, 6.698862081921435063 ) ) ;
#29467 = CARTESIAN_POINT ( 'NONE',  ( 65.69999999453763451, 142.6655632788954620, -8.961492836873480528 ) ) ;
#29468 = ORIENTED_EDGE ( 'NONE', *, *, #24157, .F. ) ;
#29469 = CARTESIAN_POINT ( 'NONE',  ( -11.98450388067348804, 210.9467285061362247, 48.65113791807857524 ) ) ;
#29470 = EDGE_CURVE ( 'NONE', #2927, #33504, #11035, .T. ) ;
#29471 = CARTESIAN_POINT ( 'NONE',  ( 8.000000000000008882, 206.9523078486586485, 68.00113791807856956 ) ) ;
#29472 = DIRECTION ( 'NONE',  ( 0.000000000000000000, 0.000000000000000000, -1.000000000000000000 ) ) ;
#29473 = CARTESIAN_POINT ( 'NONE',  ( -6.139770520408224463, 198.4640165459539389, 20.04886208192142760 ) ) ;
#29474 = ORIENTED_EDGE ( 'NONE', *, *, #4832, .F. ) ;
#29475 = CARTESIAN_POINT ( 'NONE',  ( 0.05014649552810505201, 217.5146222423826714, 85.25113791807854113 ) ) ;
#29476 = EDGE_LOOP ( 'NONE', ( #20267, #4611, #11585, #12599 ) ) ;
#29477 = LINE ( 'NONE', #5644, #20019 ) ;
#29478 = FACE_OUTER_BOUND ( 'NONE', #12102, .T. ) ;
#29479 = VERTEX_POINT ( 'NONE', #21417 ) ;
#29480 = CARTESIAN_POINT ( 'NONE',  ( 2.426778023690261410, 199.3768101843759837, 20.60113791807856742 ) ) ;
#29481 = CARTESIAN_POINT ( 'NONE',  ( -58.50000000000002132, 194.9217985566782829, 2.500000000000000000 ) ) ;
#29482 = ADVANCED_FACE ( 'NONE', ( #31804 ), #8102, .T. ) ;
#29483 = CARTESIAN_POINT ( 'NONE',  ( 9.984503880673420539, 210.2968891136705167, 3.848862081921433642 ) ) ;
#29484 = CARTESIAN_POINT ( 'NONE',  ( 49.97499999726881725, 169.8198683612136222, 4.815267126137181997 ) ) ;
#29485 = ORIENTED_EDGE ( 'NONE', *, *, #9276, .T. ) ;
#29486 = CARTESIAN_POINT ( 'NONE',  ( 56.62499999726880162, 138.6155565068815463, -3.929120461958505118E-15 ) ) ;
#29487 = DIRECTION ( 'NONE',  ( 0.000000000000000000, 0.000000000000000000, -1.000000000000000000 ) ) ;
#29488 = CARTESIAN_POINT ( 'NONE',  ( 61.28867513459483263, 170.7719333635740497, -7.904646289410545231E-15 ) ) ;
#29489 = CONICAL_SURFACE ( 'NONE', #33295, 3.339999999999998970, 0.9599310885968821427 ) ;
#29490 = DIRECTION ( 'NONE',  ( 0.000000000000000000, 0.000000000000000000, 1.000000000000000000 ) ) ;
#29491 = ADVANCED_FACE ( 'NONE', ( #8155 ), #10460, .F. ) ;
#29492 = CARTESIAN_POINT ( 'NONE',  ( -0.05014649552828403384, 217.5146222423826714, 90.24886208192141623 ) ) ;
#29493 = CARTESIAN_POINT ( 'NONE',  ( 57.27499999726882152, 149.9369285172503510, -15.58253175000000823 ) ) ;
#29494 = CARTESIAN_POINT ( 'NONE',  ( -9.984503880673473830, 210.2968891136704315, 18.65113791807856813 ) ) ;
#29495 = CARTESIAN_POINT ( 'NONE',  ( 73.78867513459483973, 155.0000000000000000, 15.00000000000001243 ) ) ;
#29496 = CARTESIAN_POINT ( 'NONE',  ( 11.98450388067341876, 210.9467285061363953, 81.84886208192142476 ) ) ;
#29497 = EDGE_CURVE ( 'NONE', #613, #22909, #31596, .T. ) ;
#29498 = CARTESIAN_POINT ( 'NONE',  ( 71.39999999999999147, 159.7113355953771077, 14.49999999999999289 ) ) ;
#29499 = DIRECTION ( 'NONE',  ( 0.000000000000000000, -0.5000000000000009992, -0.8660254037844380415 ) ) ;
#29500 = CYLINDRICAL_SURFACE ( 'NONE', #6621, 97.99999999999997158 ) ;
#29501 = CARTESIAN_POINT ( 'NONE',  ( 3.044812012440130555, 197.4746971517856764, 92.60113791807857808 ) ) ;
#29502 = FACE_OUTER_BOUND ( 'NONE', #12731, .T. ) ;
#29503 = CARTESIAN_POINT ( 'NONE',  ( 46.37499999726880873, 155.0000000000000000, 15.58253174999999402 ) ) ;
#29504 = CARTESIAN_POINT ( 'NONE',  ( 10.01549611932653860, 210.2015048109876716, 37.85113791807854966 ) ) ;
#29505 = CARTESIAN_POINT ( 'NONE',  ( 76.02499999726880731, 160.0630714827496206, 15.58253174999999402 ) ) ;
#29506 = ORIENTED_EDGE ( 'NONE', *, *, #27696, .F. ) ;
#29507 = AXIS2_PLACEMENT_3D ( 'NONE', #7934, #31592, #8258 ) ;
#29508 = CARTESIAN_POINT ( 'NONE',  ( 47.91132485994280188, 163.8167787843871110, -12.13525491562423397 ) ) ;
#29509 = CARTESIAN_POINT ( 'NONE',  ( 42.89999999453763024, 159.7113355953771077, 14.49999999999999289 ) ) ;
#29510 = CARTESIAN_POINT ( 'NONE',  ( -0.05014649552807705357, 194.3824533091408000, 17.75113791807856956 ) ) ;
#29511 = EDGE_CURVE ( 'NONE', #32783, #21298, #8839, .T. ) ;
#29512 = FACE_OUTER_BOUND ( 'NONE', #6810, .T. ) ;
#29513 = CARTESIAN_POINT ( 'NONE',  ( -5.174575781537456010, -5.672711317431625488, -7.030005583190790830 ) ) ;
#29514 = ORIENTED_EDGE ( 'NONE', *, *, #6376, .T. ) ;
#29515 = VECTOR ( 'NONE', #2937, 1000.000000000000000 ) ;
#29516 = CARTESIAN_POINT ( 'NONE',  ( 3.753561863808876797, 195.6020594897209719, 28.59886208192143897 ) ) ;
#29517 = CARTESIAN_POINT ( 'NONE',  ( 61.78867513459482552, 155.0000000000000000, 15.00000000000001243 ) ) ;
#29518 = CARTESIAN_POINT ( 'NONE',  ( -3.135527875058821579, 197.5041725223112223, 53.90113791807857524 ) ) ;
#29519 = ADVANCED_FACE ( 'NONE', ( #32976 ), #15700, .F. ) ;
#29520 = ORIENTED_EDGE ( 'NONE', *, *, #16888, .F. ) ;
#29521 = AXIS2_PLACEMENT_3D ( 'NONE', #12210, #28226, #11582 ) ;
#29522 = CARTESIAN_POINT ( 'NONE',  ( -7.984503880673422316, 204.3529502787951628, 14.34886208192143364 ) ) ;
#29523 = PRODUCT_DEFINITION_CONTEXT ( 'detailed design', #24200, 'design' ) ;
#29524 = DIRECTION ( 'NONE',  ( -1.000000000000000000, -0.000000000000000000, -0.000000000000000000 ) ) ;
#29525 = ORIENTED_EDGE ( 'NONE', *, *, #4948, .T. ) ;
#29526 = CARTESIAN_POINT ( 'NONE',  ( -6.444103211790928043, 202.2591342207265939, 101.1988620819214475 ) ) ;
#29527 = EDGE_CURVE ( 'NONE', #26026, #23251, #6756, .T. ) ;
#29528 = CARTESIAN_POINT ( 'NONE',  ( 6.500168698208129925, 211.6636982574063381, 37.70113791807857240 ) ) ;
#29529 = DIRECTION ( 'NONE',  ( 0.000000000000000000, 0.000000000000000000, -1.000000000000000000 ) ) ;
#29530 = VERTEX_POINT ( 'NONE', #8971 ) ;
#29531 = CARTESIAN_POINT ( 'NONE',  ( 40.12499999726880873, 155.0000000000000000, 15.58253174999999402 ) ) ;
#29532 = VECTOR ( 'NONE', #17186, 1000.000000000000000 ) ;
#29533 = CARTESIAN_POINT ( 'NONE',  ( 8.118202686958138514, 201.1607312380088501, 61.29886208192143471 ) ) ;
#29534 = CARTESIAN_POINT ( 'NONE',  ( 40.17499999726881299, 164.1591823560292198, 12.60653300113718167 ) ) ;
#29535 = CARTESIAN_POINT ( 'NONE',  ( 125.5000000000000000, 154.9999999999996305, -106.0000000000000142 ) ) ;
#29536 = CARTESIAN_POINT ( 'NONE',  ( 2.517493886308900919, 214.5937144450984420, 94.40113791807857524 ) ) ;
#29537 = VECTOR ( 'NONE', #32465, 1000.000000000000000 ) ;
#29538 = CARTESIAN_POINT ( 'NONE',  ( 55.00000000000000711, 170.2462022514548323, -7.872454543227099337E-15 ) ) ;
#29539 = CARTESIAN_POINT ( 'NONE',  ( 6.444103211790928043, 211.7408657792734061, 75.69886208192143329 ) ) ;
#29540 = CARTESIAN_POINT ( 'NONE',  ( 77.68867513459484542, 159.8737954434933215, 15.00000000000024336 ) ) ;
#29541 = CIRCLE ( 'NONE', #8343, 2.500000000000000000 ) ;
#29542 = ADVANCED_FACE ( 'NONE', ( #27362 ), #22590, .F. ) ;
#29543 = CONICAL_SURFACE ( 'NONE', #6715, 32.00000000000000000, 0.1047197551197278087 ) ;
#29544 = CARTESIAN_POINT ( 'NONE',  ( 56.92499999726881299, 145.8408176439707802, -12.60653300113719588 ) ) ;
#29545 = CARTESIAN_POINT ( 'NONE',  ( 10.00000000000000711, 206.9523078486586201, 14.00113791807856600 ) ) ;
#29546 = CARTESIAN_POINT ( 'NONE',  ( 37.01132485994280330, 142.2402378747194405, 9.270509831248432420 ) ) ;
#29547 = CARTESIAN_POINT ( 'NONE',  ( 67.92499999726881299, 164.1591823560292198, 12.60653300113718167 ) ) ;
#29548 = CARTESIAN_POINT ( 'NONE',  ( 75.07499999726879025, 141.7447067706911810, -9.630534252274385310 ) ) ;
#29549 = CARTESIAN_POINT ( 'NONE',  ( -0.05014649552807705357, 194.3824533091408000, 77.75113791807856956 ) ) ;
#29550 = EDGE_CURVE ( 'NONE', #24364, #22995, #2090, .T. ) ;
#29551 = CARTESIAN_POINT ( 'NONE',  ( -6.220909254589537696, 198.5229672870051445, 102.0511379180785525 ) ) ;
#29552 = CARTESIAN_POINT ( 'NONE',  ( 53.58867513459482268, 163.8167787843871110, 12.13525491562421621 ) ) ;
#29553 = ORIENTED_EDGE ( 'NONE', *, *, #6380, .T. ) ;
#29554 = CARTESIAN_POINT ( 'NONE',  ( 3.135527875058981895, 197.5041725223112792, 4.598862081921434530 ) ) ;
#29555 = CARTESIAN_POINT ( 'NONE',  ( 9.680171189290716072, 214.0920067884432854, 63.69886208192144039 ) ) ;
#29556 = VECTOR ( 'NONE', #2145, 1000.000000000000000 ) ;
#29557 = CARTESIAN_POINT ( 'NONE',  ( 10.01549611932659367, 203.7984951890124421, 64.14886208192143613 ) ) ;
#29558 = CARTESIAN_POINT ( 'NONE',  ( 7.456977232089471386, 196.8216656703012006, 1.448862081921433953 ) ) ;
#29559 = CARTESIAN_POINT ( 'NONE',  ( 94.70964751525852421, 155.0000000000000000, 32.10452846326766974 ) ) ;
#29560 = CARTESIAN_POINT ( 'NONE',  ( 0.05014649552810505201, 217.5146222423826714, 19.25113791807856600 ) ) ;
#29561 = ADVANCED_FACE ( 'NONE', ( #19697 ), #20037, .T. ) ;
#29562 = CARTESIAN_POINT ( 'NONE',  ( 6.220909254589681581, 198.5229672870052582, 85.44886208192140487 ) ) ;
#29563 = EDGE_LOOP ( 'NONE', ( #6488, #3171, #24357, #15453 ) ) ;
#29564 = CARTESIAN_POINT ( 'NONE',  ( 39.71132485994280614, 155.0000000000000000, -15.00000000000002487 ) ) ;
#29565 = AXIS2_PLACEMENT_3D ( 'NONE', #17260, #32756, #10117 ) ;
#29566 = ORIENTED_EDGE ( 'NONE', *, *, #10125, .F. ) ;
#29567 = DIRECTION ( 'NONE',  ( 1.000000000000000000, 0.000000000000000000, 0.000000000000000000 ) ) ;
#29568 = CARTESIAN_POINT ( 'NONE',  ( -2.426778023690076225, 199.3768101843759553, 73.89886208192143613 ) ) ;
#29569 = TOROIDAL_SURFACE ( 'NONE', #20334, 4.400000000000001243, 0.4000000000000000222 ) ;
#29570 = ORIENTED_EDGE ( 'NONE', *, *, #23741, .F. ) ;
#29571 = CIRCLE ( 'NONE', #2928, 0.4000000000000001887 ) ;
#29572 = CARTESIAN_POINT ( 'NONE',  ( 85.52499999726880731, 169.8198683612136222, -4.815267126137197984 ) ) ;
#29573 = EDGE_LOOP ( 'NONE', ( #16316, #18670, #451, #33549 ) ) ;
#29574 = CARTESIAN_POINT ( 'NONE',  ( -13.75000000000001954, 23.81569860407205752, -18.00000000000000000 ) ) ;
#29575 = CARTESIAN_POINT ( 'NONE',  ( 68.52499999726880731, 140.1801316387863778, 4.815267126137185549 ) ) ;
#29576 = CARTESIAN_POINT ( 'NONE',  ( 8.000000000000008882, 206.9523078486586485, 68.00113791807856956 ) ) ;
#29577 = DIRECTION ( 'NONE',  ( -1.000000000000000000, -0.000000000000000000, -0.000000000000000000 ) ) ;
#29578 = FACE_OUTER_BOUND ( 'NONE', #26537, .T. ) ;
#29579 =( LENGTH_UNIT ( ) NAMED_UNIT ( * ) SI_UNIT ( .MILLI., .METRE. ) );
#29580 = CARTESIAN_POINT ( 'NONE',  ( 33.89999999999999858, 141.2096805137202580, 4.480746418436733158 ) ) ;
#29581 = CARTESIAN_POINT ( 'NONE',  ( -8.015496119326597224, 209.5516654185217362, 41.64886208192143613 ) ) ;
#29582 = CARTESIAN_POINT ( 'NONE',  ( -9.984503880673473830, 210.2968891136704315, 93.65113791807857524 ) ) ;
#29583 = EDGE_CURVE ( 'NONE', #16076, #24063, #32008, .T. ) ;
#29584 = CARTESIAN_POINT ( 'NONE',  ( 10.01549611932653860, 210.2015048109876716, 61.85113791807857098 ) ) ;
#29585 = EDGE_CURVE ( 'NONE', #2221, #29773, #31491, .T. ) ;
#29586 = CARTESIAN_POINT ( 'NONE',  ( 95.59906517536109050, 155.0000000000000000, 0.000000000000000000 ) ) ;
#29587 = CARTESIAN_POINT ( 'NONE',  ( -6.500168698208129925, 202.3363017425936050, 21.20113791807856529 ) ) ;
#29588 = DIRECTION ( 'NONE',  ( -1.000000000000000000, 0.000000000000000000, 0.000000000000000000 ) ) ;
#29589 = AXIS2_PLACEMENT_3D ( 'NONE', #2896, #30854, #28954 ) ;
#29590 = CARTESIAN_POINT ( 'NONE',  ( -5.727634848077285845, 4.575561887448583498, -6.326622577870772979 ) ) ;
#29591 = CARTESIAN_POINT ( 'NONE',  ( 45.52499999726881441, 169.8198683612136222, -4.815267126137197984 ) ) ;
#29592 = CARTESIAN_POINT ( 'NONE',  ( 3.662846001190051659, 195.5725841191953691, 50.60113791807857808 ) ) ;
#29593 = DIRECTION ( 'NONE',  ( 0.000000000000000000, 0.000000000000000000, 1.000000000000000000 ) ) ;
#29594 = PRODUCT_RELATED_PRODUCT_CATEGORY ( 'part', '', ( #22483 ) ) ;
#29595 = CARTESIAN_POINT ( 'NONE',  ( 8.118202686958039038, 212.8392687619912635, 91.70113791807857240 ) ) ;
#29596 = EDGE_CURVE ( 'NONE', #12975, #25011, #17327, .T. ) ;
#29597 = CARTESIAN_POINT ( 'NONE',  ( 6.139770520408367460, 198.4640165459539389, 65.45113791807857240 ) ) ;
#29598 = CARTESIAN_POINT ( 'NONE',  ( -7.375838497908014268, 196.7627149292498530, 35.04886208192143471 ) ) ;
#29599 = CARTESIAN_POINT ( 'NONE',  ( -8.062137200540822946, 201.0835637161416400, 35.19886208192143329 ) ) ;
#29600 = CARTESIAN_POINT ( 'NONE',  ( 88.69999999453763451, 167.3344367211045096, 8.961492836873468093 ) ) ;
#29601 = CARTESIAN_POINT ( 'NONE',  ( 11.98450388067348271, 203.0532714938637753, 77.15113791807857524 ) ) ;
#29602 = CARTESIAN_POINT ( 'NONE',  ( -7.949154985843430055, 215.5765611960900117, 102.9933096652613642 ) ) ;
#29603 =( BOUNDED_CURVE ( )  B_SPLINE_CURVE ( 2, ( #14232, #16950, #1295, #24800, #6225, #17130, #27516, #25124, #6740, #11686, #4174 ),
 .UNSPECIFIED., .F., .T. ) 
 B_SPLINE_CURVE_WITH_KNOTS ( ( 3, 2, 2, 2, 2, 3 ),
 ( 0.6249999999999998890, 0.6285714285714284477, 0.6321428571428570065, 0.6357142857142855652, 0.6392857142857141239, 0.6428571428571427937 ),
 .UNSPECIFIED. ) 
 CURVE ( )  GEOMETRIC_REPRESENTATION_ITEM ( )  RATIONAL_B_SPLINE_CURVE ( ( 1.000000000000001554, 0.9510565162951518658, 1.000000000000000000, 0.9510565162951534202, 1.000000000000000000, 0.9510565162951534202, 1.000000000000000000, 0.9510565162951534202, 1.000000000000000000, 0.9510565162951549745, 0.9999999999999984457 ) ) 
 REPRESENTATION_ITEM ( '' )  );
#29604 = CARTESIAN_POINT ( 'NONE',  ( 3.044812012439969795, 216.5253028482143520, 57.39886208192143613 ) ) ;
#29605 = CARTESIAN_POINT ( 'NONE',  ( 32.50000000000000000, 155.0000000000000000, -6.938893903907228378E-15 ) ) ;
#29606 = EDGE_LOOP ( 'NONE', ( #20255, #23744 ) ) ;
#29607 = CARTESIAN_POINT ( 'NONE',  ( 3.662846001189864698, 218.4274158808046593, 63.39886208192144323 ) ) ;
#29608 =( GEOMETRIC_REPRESENTATION_CONTEXT ( 3 ) GLOBAL_UNCERTAINTY_ASSIGNED_CONTEXT ( ( #16839 ) ) GLOBAL_UNIT_ASSIGNED_CONTEXT ( ( #15120, #20411, #20067 ) ) REPRESENTATION_CONTEXT ( 'NONE', 'WORKASPACE' ) );
#29609 = ORIENTED_EDGE ( 'NONE', *, *, #29, .T. ) ;
#29610 = CARTESIAN_POINT ( 'NONE',  ( 73.07499999726880446, 141.7447067706911810, -9.630534252274385310 ) ) ;
#29611 = CARTESIAN_POINT ( 'NONE',  ( 7.984503880673422316, 209.6470497212048372, 42.84886208192143897 ) ) ;
#29612 = VERTEX_POINT ( 'NONE', #14586 ) ;
#29613 = CARTESIAN_POINT ( 'NONE',  ( 78.27499999726880731, 160.0630714827496206, 15.58253174999999224 ) ) ;
#29614 = DIRECTION ( 'NONE',  ( 1.000000000000000000, -0.000000000000000000, -0.000000000000000000 ) ) ;
#29615 = DIRECTION ( 'NONE',  ( -0.2649168722799616349, 0.9642688156137669830, -0.002168413296787739895 ) ) ;
#29616 = CARTESIAN_POINT ( 'NONE',  ( 2.517493886308900919, 214.5937144450984420, 49.40113791807856813 ) ) ;
#29617 =( NAMED_UNIT ( * ) PLANE_ANGLE_UNIT ( ) SI_UNIT ( $, .RADIAN. ) );
#29618 = CARTESIAN_POINT ( 'NONE',  ( 0.05014649552828275708, 196.4853777576173002, 37.74886208192143755 ) ) ;
#29619 = CARTESIAN_POINT ( 'NONE',  ( 69.27499999726880731, 149.9369285172503510, -15.58253175000000823 ) ) ;
#29620 = ORIENTED_EDGE ( 'NONE', *, *, #21976, .F. ) ;
#29621 = CARTESIAN_POINT ( 'NONE',  ( 61.78867513459482552, 155.0000000000000000, 15.00000000000001243 ) ) ;
#29622 = CARTESIAN_POINT ( 'NONE',  ( 117.5000000000000000, 155.0000000000000000, -98.00000000000000000 ) ) ;
#29623 = CARTESIAN_POINT ( 'NONE',  ( -3.823040241140506157E-16, -8.660254037844397956, -7.564338275809345369 ) ) ;
#29624 = CARTESIAN_POINT ( 'NONE',  ( 2.517493886309087436, 199.4062855549015865, 13.59886208192143719 ) ) ;
#29625 = CARTESIAN_POINT ( 'NONE',  ( -3.044812012440131443, 216.5253028482142952, 52.10113791807857808 ) ) ;
#29626 = CARTESIAN_POINT ( 'NONE',  ( -3.135527875058821579, 197.5041725223112223, 32.90113791807857524 ) ) ;
#29627 = CARTESIAN_POINT ( 'NONE',  ( 85.17499999726882720, 145.8408176439707802, -12.60653300113719588 ) ) ;
#29628 = ITEM_DEFINED_TRANSFORMATION ( 'NONE', 'NONE', #17541,  #2404 ) ;
#29629 =( GEOMETRIC_REPRESENTATION_CONTEXT ( 3 ) GLOBAL_UNCERTAINTY_ASSIGNED_CONTEXT ( ( #3176 ) ) GLOBAL_UNIT_ASSIGNED_CONTEXT ( ( #18194, #33522, #27895 ) ) REPRESENTATION_CONTEXT ( 'NONE', 'WORKASPACE' ) );
#29630 = CARTESIAN_POINT ( 'NONE',  ( -7.984503880673422316, 204.3529502787951628, 98.34886208192145318 ) ) ;
#29631 = CARTESIAN_POINT ( 'NONE',  ( 42.92499999726881299, 145.8408176439707802, -12.60653300113719588 ) ) ;
#29632 =( LENGTH_UNIT ( ) NAMED_UNIT ( * ) SI_UNIT ( .MILLI., .METRE. ) );
#29633 = LINE ( 'NONE', #16011, #27776 ) ;
#29634 = CARTESIAN_POINT ( 'NONE',  ( 7.456977232089302632, 217.1783343296989131, 22.55113791807857027 ) ) ;
#29635 = LINE ( 'NONE', #23846, #22187 ) ;
#29636 = CARTESIAN_POINT ( 'NONE',  ( -10.00000000000000711, 207.0476921513413515, 69.50113791807856956 ) ) ;
#29637 = CARTESIAN_POINT ( 'NONE',  ( 3.135527875058820690, 216.4958274776887492, 43.40113791807856813 ) ) ;
#29638 = CARTESIAN_POINT ( 'NONE',  ( -60.00000000000000000, -7.347880794884118356E-15, 35.00000000000000000 ) ) ;
#29639 = CARTESIAN_POINT ( 'NONE',  ( 77.78867513459483973, 155.0000000000000000, 15.00000000000001243 ) ) ;
#29640 = CARTESIAN_POINT ( 'NONE',  ( 7.375838497908181246, 196.7627149292499666, 101.4511379180785866 ) ) ;
#29641 = CARTESIAN_POINT ( 'NONE',  ( 8.118202686958138514, 201.1607312380088501, 7.298862081921435596 ) ) ;
#29642 = CARTESIAN_POINT ( 'NONE',  ( 66.29999999453762882, 167.3344367211045096, -8.961492836873482304 ) ) ;
#29643 = ORIENTED_EDGE ( 'NONE', *, *, #6565, .F. ) ;
#29644 = CARTESIAN_POINT ( 'NONE',  ( 9.736236675707914401, 214.0148392665762458, 49.70113791807856529 ) ) ;
#29645 = CARTESIAN_POINT ( 'NONE',  ( 8.000000000000008882, 206.9523078486586485, 71.00113791807856956 ) ) ;
#29646 = CARTESIAN_POINT ( 'NONE',  ( 4.931287292257855448, 207.3577873115561943, -9.395021131069748677 ) ) ;
#29647 = CARTESIAN_POINT ( 'NONE',  ( 10.01549611932659545, 203.7984951890123853, 34.14886208192143613 ) ) ;
#29648 = DIRECTION ( 'NONE',  ( 0.000000000000000000, 0.000000000000000000, -1.000000000000000000 ) ) ;
#29649 = ORIENTED_EDGE ( 'NONE', *, *, #26845, .F. ) ;
#29650 = CARTESIAN_POINT ( 'NONE',  ( 8.062137200540920645, 201.0835637161417822, 77.30113791807858092 ) ) ;
#29651 = ORIENTED_EDGE ( 'NONE', *, *, #5182, .F. ) ;
#29652 = DIRECTION ( 'NONE',  ( -1.000000000000000000, 0.000000000000000000, 0.000000000000000000 ) ) ;
#29653 = DIRECTION ( 'NONE',  ( -0.000000000000000000, -0.000000000000000000, -1.000000000000000000 ) ) ;
#29654 = EDGE_LOOP ( 'NONE', ( #12777, #21518, #1161, #3903 ) ) ;
#29655 = CARTESIAN_POINT ( 'NONE',  ( 8.015496119326531499, 209.5516654185219636, 22.85113791807856742 ) ) ;
#29656 = CARTESIAN_POINT ( 'NONE',  ( -59.30608239026425821, 194.9296489543815483, 2.372148111071822996 ) ) ;
#29657 = CARTESIAN_POINT ( 'NONE',  ( -10.00000000000000711, 206.9523078486584495, 5.498862081921434886 ) ) ;
#29658 = CARTESIAN_POINT ( 'NONE',  ( 51.67499999726879878, 168.2552932293087906, -9.630534252274387086 ) ) ;
#29659 = ORIENTED_EDGE ( 'NONE', *, *, #16996, .T. ) ;
#29660 = CARTESIAN_POINT ( 'NONE',  ( 57.92499999726881299, 164.1591823560292198, 12.60653300113718167 ) ) ;
#29661 = CARTESIAN_POINT ( 'NONE',  ( -2.517493886308901807, 199.4062855549015012, 50.90113791807858235 ) ) ;
#29662 = CARTESIAN_POINT ( 'NONE',  ( 61.18867513459481700, 169.2658477444273331, -4.635254915624224203 ) ) ;
#29663 = DIRECTION ( 'NONE',  ( -1.000000000000000000, 0.000000000000000000, 0.000000000000000000 ) ) ;
#29664 = CARTESIAN_POINT ( 'NONE',  ( 3.044812012439969795, 216.5253028482143520, 90.39886208192143613 ) ) ;
#29665 = CARTESIAN_POINT ( 'NONE',  ( 58.87499999726880162, 138.6155565068815463, -3.929120461958505118E-15 ) ) ;
#29666 = CARTESIAN_POINT ( 'NONE',  ( -6.139770520408369237, 215.5359834540460042, 18.95113791807856884 ) ) ;
#29667 = CARTESIAN_POINT ( 'NONE',  ( 2.428571428571428381, 0.000000000000000000, 3.100000000000000533 ) ) ;
#29668 = CARTESIAN_POINT ( 'NONE',  ( -3.753561863808878130, 218.3979405102790281, 81.09886208192143897 ) ) ;
#29669 = CARTESIAN_POINT ( 'NONE',  ( 73.70000000000000284, 146.4771138417591203, 11.73074641843673227 ) ) ;
#29670 = CARTESIAN_POINT ( 'NONE',  ( 40.68867513459483121, 150.1262045565064227, -15.00000000000002665 ) ) ;
#29671 = DIRECTION ( 'NONE',  ( -1.000000000000000000, -0.000000000000000000, -0.000000000000000000 ) ) ;
#29672 = CARTESIAN_POINT ( 'NONE',  ( -6.220909254589537696, 198.5229672870051161, 96.05113791807858092 ) ) ;
#29673 = CARTESIAN_POINT ( 'NONE',  ( 6.815830331203685866, 1.228021141713631082E-13, -6.171384342982610960 ) ) ;
#29674 = CARTESIAN_POINT ( 'NONE',  ( 46.07499999726881157, 168.2552932293087906, 9.630534252274372875 ) ) ;
#29675 = CARTESIAN_POINT ( 'NONE',  ( -6.139770520408369237, 215.5359834540460042, 33.95113791807855108 ) ) ;
#29676 = CARTESIAN_POINT ( 'NONE',  ( 76.22499999726882436, 149.9369285172503510, 15.58253174999999580 ) ) ;
#29677 = ORIENTED_EDGE ( 'NONE', *, *, #8738, .T. ) ;
#29678 = DIRECTION ( 'NONE',  ( 1.000000000000000000, -0.000000000000000000, -0.000000000000000000 ) ) ;
#29679 = CARTESIAN_POINT ( 'NONE',  ( 49.09999999453761887, 150.2886644046228639, 14.49999999999999645 ) ) ;
#29680 = CARTESIAN_POINT ( 'NONE',  ( 12.01549611932652972, 210.8513442034534933, 19.85113791807856387 ) ) ;
#29681 = DIRECTION ( 'NONE',  ( 0.000000000000000000, 0.000000000000000000, -1.000000000000000000 ) ) ;
#29682 = EDGE_CURVE ( 'NONE', #12471, #22574, #24987, .T. ) ;
#29683 = CARTESIAN_POINT ( 'NONE',  ( -52.50000000000002132, 155.0000000000000000, -6.938893903907228378E-15 ) ) ;
#29684 = VERTEX_POINT ( 'NONE', #16802 ) ;
#29685 = CARTESIAN_POINT ( 'NONE',  ( 3.753561863808876797, 195.6020594897209719, 46.59886208192143187 ) ) ;
#29686 = DIRECTION ( 'NONE',  ( 0.000000000000000000, 0.000000000000000000, -1.000000000000000000 ) ) ;
#29687 = CARTESIAN_POINT ( 'NONE',  ( -3.044812012440131443, 216.5253028482142952, 52.10113791807857808 ) ) ;
#29688 = ORIENTED_EDGE ( 'NONE', *, *, #4540, .T. ) ;
#29689 = CARTESIAN_POINT ( 'NONE',  ( -6.500168698208244500, 211.6636982574061676, 17.79886208192143471 ) ) ;
#29690 = CARTESIAN_POINT ( 'NONE',  ( 50.68867513459483121, 150.1262045565064227, -15.00000000000002665 ) ) ;
#29691 = ORIENTED_EDGE ( 'NONE', *, *, #23274, .T. ) ;
#29692 = CARTESIAN_POINT ( 'NONE',  ( -2.426778023690076225, 199.3768101843759553, 97.89886208192146455 ) ) ;
#29693 = DIRECTION ( 'NONE',  ( -1.000000000000000000, 0.000000000000000000, -0.000000000000000000 ) ) ;
#29694 = CARTESIAN_POINT ( 'NONE',  ( 6.500168698208129925, 211.6636982574063381, 43.70113791807857240 ) ) ;
#29695 = CARTESIAN_POINT ( 'NONE',  ( 9.379977934355910207, 208.8253170565643870, -1.014254689207407356 ) ) ;
#29696 = EDGE_LOOP ( 'NONE', ( #27840, #14430 ) ) ;
#29697 = CARTESIAN_POINT ( 'NONE',  ( 39.82499999726880446, 168.2552932293087906, 9.630534252274372875 ) ) ;
#29698 = CARTESIAN_POINT ( 'NONE',  ( 10.01549611932659545, 203.7984951890123853, 64.14886208192145034 ) ) ;
#29699 = CARTESIAN_POINT ( 'NONE',  ( 42.37499999726881583, 155.0000000000000000, 15.58253174999999402 ) ) ;
#29700 = CARTESIAN_POINT ( 'NONE',  ( 115.4999999999999858, 180.9145392013172682, 100.8678580070898931 ) ) ;
#29701 = CARTESIAN_POINT ( 'NONE',  ( 2.517493886308900919, 214.5937144450984420, 97.40113791807858945 ) ) ;
#29702 = CARTESIAN_POINT ( 'NONE',  ( 53.00000000000000711, 170.2462022514548323, -7.872454543227099337E-15 ) ) ;
#29703 = CARTESIAN_POINT ( 'NONE',  ( 5.416666666666667851, 4.378239541354659536, -5.848636054922034866 ) ) ;
#29704 = CARTESIAN_POINT ( 'NONE',  ( -7.984503880673422316, 204.3529502787951628, 77.34886208192143897 ) ) ;
#29705 = CARTESIAN_POINT ( 'NONE',  ( 103.4083388212532810, 155.0000000000000000, 0.000000000000000000 ) ) ;
#29706 = EDGE_CURVE ( 'NONE', #23586, #21724, #17478, .T. ) ;
#29707 = CARTESIAN_POINT ( 'NONE',  ( 1.650000000000000133, 0.000000000000000000, -2.629527361626598836 ) ) ;
#29708 = CARTESIAN_POINT ( 'NONE',  ( 59.12499999726881583, 155.0000000000000000, -15.58253175000000823 ) ) ;
#29710 = ORIENTED_EDGE ( 'NONE', *, *, #26948, .F. ) ;
#29709 = CARTESIAN_POINT ( 'NONE',  ( 9.984503880673473830, 203.7031108863295401, 23.15113791807856813 ) ) ;
#29711 = FACE_OUTER_BOUND ( 'NONE', #2811, .T. ) ;
#29712 = CARTESIAN_POINT ( 'NONE',  ( 82.67499999726879878, 141.7447067706911810, 9.630534252274376428 ) ) ;
#29713 = CARTESIAN_POINT ( 'NONE',  ( -12.00000000000000711, 207.0476921513413515, 81.50113791807856956 ) ) ;
#29714 = CARTESIAN_POINT ( 'NONE',  ( 6.139770520408367460, 198.4640165459539389, 95.45113791807855819 ) ) ;
#29715 = EDGE_CURVE ( 'NONE', #14095, #8954, #23082, .T. ) ;
#29716 = DIRECTION ( 'NONE',  ( 0.000000000000000000, 0.000000000000000000, -1.000000000000000000 ) ) ;
#29717 = AXIS2_PLACEMENT_3D ( 'NONE', #29683, #16729, #2250 ) ;
#29718 = VERTEX_POINT ( 'NONE', #25831 ) ;
#29719 = CARTESIAN_POINT ( 'NONE',  ( -12.05084501415679199, 219.7456114157811271, 104.9910338291041114 ) ) ;
#29720 = CARTESIAN_POINT ( 'NONE',  ( -11.98450388067341876, 203.0532714938636047, 62.34886208192143187 ) ) ;
#29721 = CIRCLE ( 'NONE', #33551, 0.9999999999999947820 ) ;
#29722 = CARTESIAN_POINT ( 'NONE',  ( -3.135527875058982783, 216.4958274776886924, 78.09886208192143897 ) ) ;
#29723 = CARTESIAN_POINT ( 'NONE',  ( 7.375838497908181246, 196.7627149292499666, 101.4511379180785866 ) ) ;
#29724 = CARTESIAN_POINT ( 'NONE',  ( 127.5000000000000000, 155.0000000000000000, -98.00000000000002842 ) ) ;
#29725 = CARTESIAN_POINT ( 'NONE',  ( -10.00000000000000711, 207.0476921513413515, 18.50113791807856956 ) ) ;
#29726 = CARTESIAN_POINT ( 'NONE',  ( -10.01549611932659722, 210.2015048109875011, 92.64886208192143613 ) ) ;
#29728 = ORIENTED_EDGE ( 'NONE', *, *, #5623, .F. ) ;
#29727 = CIRCLE ( 'NONE', #26999, 40.00000000000000711 ) ;
#29729 = EDGE_CURVE ( 'NONE', #7343, #8868, #31539, .T. ) ;
#29730 = CARTESIAN_POINT ( 'NONE',  ( 39.21132485994281325, 139.2280666364260071, -4.041636747397287284E-15 ) ) ;
#29731 = ORIENTED_EDGE ( 'NONE', *, *, #17084, .F. ) ;
#29732 = DIRECTION ( 'NONE',  ( -0.9891821073486148919, -0.1466927349985451545, 0.000000000000000000 ) ) ;
#29733 = CARTESIAN_POINT ( 'NONE',  ( 2.517493886309087436, 199.4062855549015865, 70.59886208192142476 ) ) ;
#29734 = EDGE_LOOP ( 'NONE', ( #12646, #9462 ) ) ;
#29735 = CARTESIAN_POINT ( 'NONE',  ( 83.72499999726882436, 169.8198683612136222, 4.815267126137181997 ) ) ;
#29736 = ORIENTED_EDGE ( 'NONE', *, *, #27889, .T. ) ;
#29737 = DIRECTION ( 'NONE',  ( 0.000000000000000000, 0.000000000000000000, 1.000000000000000000 ) ) ;
#29738 = CARTESIAN_POINT ( 'NONE',  ( 73.42499999726881299, 168.2552932293087906, -9.630534252274385310 ) ) ;
#29739 = EDGE_CURVE ( 'NONE', #576, #28972, #2667, .T. ) ;
#29740 = CARTESIAN_POINT ( 'NONE',  ( -8.000000000000008882, 207.0476921513413515, 72.50113791807856956 ) ) ;
#29741 = CARTESIAN_POINT ( 'NONE',  ( 58.50000000000001421, -88.00000000000000000, 30.00000000000000000 ) ) ;
#29742 = EDGE_CURVE ( 'NONE', #23251, #23990, #25475, .T. ) ;
#29743 = AXIS2_PLACEMENT_3D ( 'NONE', #32734, #27623, #19801 ) ;
#29744 = AXIS2_PLACEMENT_3D ( 'NONE', #22830, #19766, #22146 ) ;
#29745 = CARTESIAN_POINT ( 'NONE',  ( 35.80000000000000426, 142.6655632788954620, 8.961492836873471646 ) ) ;
#29746 = CARTESIAN_POINT ( 'NONE',  ( 8.000000000000008882, 207.0476921513415220, 45.99886208192144466 ) ) ;
#29747 = EDGE_CURVE ( 'NONE', #28109, #6207, #25316, .T. ) ;
#29748 = CARTESIAN_POINT ( 'NONE',  ( 9.984503880673470277, 203.7031108863295401, 89.15113791807857524 ) ) ;
#29749 = CARTESIAN_POINT ( 'NONE',  ( 10.01549611932653860, 210.2015048109876716, 76.85113791807857808 ) ) ;
#29750 = VECTOR ( 'NONE', #24970, 1000.000000000000000 ) ;
#29751 = CARTESIAN_POINT ( 'NONE',  ( 0.000000000000000000, 0.000000000000000000, 0.000000000000000000 ) ) ;
#29752 = DIRECTION ( 'NONE',  ( 0.000000000000000000, 0.000000000000000000, -1.000000000000000000 ) ) ;
#29753 = CARTESIAN_POINT ( 'NONE',  ( 32.50000000000000000, 155.0000000000000000, -15.00000000000002487 ) ) ;
#29754 = CARTESIAN_POINT ( 'NONE',  ( 52.92499999726881299, 145.8408176439707802, -12.60653300113719588 ) ) ;
#29755 = CARTESIAN_POINT ( 'NONE',  ( -12.01549611932652972, 203.1486557965464499, 48.35113791807857098 ) ) ;
#29756 = CARTESIAN_POINT ( 'NONE',  ( 41.11132485994280472, 140.7341522555726669, 4.635254915624211769 ) ) ;
#29757 = CARTESIAN_POINT ( 'NONE',  ( -10.01549611932653860, 203.7984951890123284, 90.35113791807857808 ) ) ;
#29758 = CARTESIAN_POINT ( 'NONE',  ( 3.135527875058820690, 216.4958274776887492, 67.40113791807857524 ) ) ;
#29759 = CARTESIAN_POINT ( 'NONE',  ( -12.00000000000000711, 206.9523078486584780, 29.49886208192143400 ) ) ;
#29760 = CARTESIAN_POINT ( 'NONE',  ( 8.118202686958138514, 201.1607312380088501, 40.29886208192143471 ) ) ;
#29761 = CARTESIAN_POINT ( 'NONE',  ( 87.79999999453764303, 146.4771138417591203, -11.73074641843674470 ) ) ;
#29762 = CARTESIAN_POINT ( 'NONE',  ( 12.00000000000000711, 206.9523078486586485, 74.00113791807856956 ) ) ;
#29763 = AXIS2_PLACEMENT_3D ( 'NONE', #13646, #32208, #11439 ) ;
#29764 = CARTESIAN_POINT ( 'NONE',  ( -2.426778023690262742, 214.6231898156240163, 97.10113791807857808 ) ) ;
#29765 = CARTESIAN_POINT ( 'NONE',  ( 6.220909254589681581, 198.5229672870052582, 61.44886208192141908 ) ) ;
#29766 = CONICAL_SURFACE ( 'NONE', #17243, 7.500000000000001776, 0.8594454914424796144 ) ;
#29767 = LINE ( 'NONE', #8984, #16164 ) ;
#29768 = ORIENTED_EDGE ( 'NONE', *, *, #822, .T. ) ;
#29769 = CARTESIAN_POINT ( 'NONE',  ( -11.98450388067341876, 203.0532714938636047, 59.34886208192144608 ) ) ;
#29770 = ORIENTED_EDGE ( 'NONE', *, *, #1423, .T. ) ;
#29771 = CARTESIAN_POINT ( 'NONE',  ( 74.27499999726880731, 160.0630714827496206, 15.58253174999999402 ) ) ;
#29772 = CARTESIAN_POINT ( 'NONE',  ( 2.426778023690075337, 214.6231898156240447, 45.39886208192144323 ) ) ;
#29773 = VERTEX_POINT ( 'NONE', #10507 ) ;
#29774 = EDGE_CURVE ( 'NONE', #18219, #22743, #18167, .T. ) ;
#29775 = EDGE_CURVE ( 'NONE', #33083, #17200, #27657, .T. ) ;
#29776 = CARTESIAN_POINT ( 'NONE',  ( 80.37499999726881583, 155.0000000000000000, 15.58253174999999402 ) ) ;
#29777 = DIRECTION ( 'NONE',  ( 0.7071067811865454633, -0.000000000000000000, -0.7071067811865495711 ) ) ;
#29778 = CARTESIAN_POINT ( 'NONE',  ( 127.5000000000000000, 229.9533188057739039, -74.95331880577418815 ) ) ;
#29779 = CARTESIAN_POINT ( 'NONE',  ( 7.984503880673485376, 204.3529502787953902, 53.15113791807857524 ) ) ;
#29780 = PRODUCT_DEFINITION ( 'UNKNOWN', '', #24056, #21687 ) ;
#29781 = EDGE_CURVE ( 'NONE', #18640, #31129, #33326, .T. ) ;
#29782 = DIRECTION ( 'NONE',  ( 0.000000000000000000, 0.000000000000000000, 1.000000000000000000 ) ) ;
#29783 = CARTESIAN_POINT ( 'NONE',  ( 0.05014649552828275708, 196.4853777576173002, 28.74886208192144110 ) ) ;
#29784 = CARTESIAN_POINT ( 'NONE',  ( 66.57499999726881867, 145.8408176439707802, 12.60653300113718345 ) ) ;
#29785 = ORIENTED_EDGE ( 'NONE', *, *, #1015, .T. ) ;
#29786 = DIRECTION ( 'NONE',  ( 1.000000000000000000, 0.000000000000000000, 0.000000000000000000 ) ) ;
#29787 = CARTESIAN_POINT ( 'NONE',  ( 52.58867513459482268, 146.1832212156128890, -12.13525491562423042 ) ) ;
#29788 = CARTESIAN_POINT ( 'NONE',  ( 60.00000000000000000, 7.347880794884118356E-15, 35.00000000000000000 ) ) ;
#29789 = CARTESIAN_POINT ( 'NONE',  ( 6.444103211790928043, 211.7408657792734061, 12.69886208192143684 ) ) ;
#29790 = AXIS2_PLACEMENT_3D ( 'NONE', #2011, #22795, #132 ) ;
#29791 = ADVANCED_FACE ( 'NONE', ( #23271 ), #33494, .T. ) ;
#29792 = CARTESIAN_POINT ( 'NONE',  ( -3.044812012440131443, 216.5253028482142952, 58.10113791807857808 ) ) ;
#29793 = CARTESIAN_POINT ( 'NONE',  ( 8.118202686958039038, 212.8392687619912635, 34.70113791807857240 ) ) ;
#29794 = DIRECTION ( 'NONE',  ( 1.224646799147353207E-16, 1.000000000000000000, 0.000000000000000000 ) ) ;
#29795 = AXIS2_PLACEMENT_3D ( 'NONE', #31782, #18835, #4006 ) ;
#29796 = ITEM_DEFINED_TRANSFORMATION ( 'NONE', 'NONE', #24080,  #2404 ) ;
#29797 = AXIS2_PLACEMENT_3D ( 'NONE', #32966, #6744, #17468 ) ;
#29798 = CARTESIAN_POINT ( 'NONE',  ( -6.500168698208129925, 202.3363017425936050, 0.2011379180785659582 ) ) ;
#29799 = CARTESIAN_POINT ( 'NONE',  ( 47.32499999726881867, 164.1591823560292198, -12.60653300113719766 ) ) ;
#29800 = CARTESIAN_POINT ( 'NONE',  ( -6.500000000000000000, 3.752776749732564809, -0.7999999999999969358 ) ) ;
#29801 = DIRECTION ( 'NONE',  ( 0.000000000000000000, 0.000000000000000000, 1.000000000000000000 ) ) ;
#29802 = CARTESIAN_POINT ( 'NONE',  ( -9.736236675707914401, 199.9851607334237542, 15.20113791807857062 ) ) ;
#29803 = FACE_OUTER_BOUND ( 'NONE', #32189, .T. ) ;
#29804 =( BOUNDED_SURFACE ( )  B_SPLINE_SURFACE ( 1, 2, ( 
 ( #31911, #15910, #8253, #26307, #29033, #18310, #29198, #2978, #13357, #8583, #23751, #2650, #5361, #415, #10818, #23917, #10976, #4133, #14525, #27308, #13859, #24925, #9419, #6186, #11975, #1584, #24244, #30035, #29873, #19473, #6532, #22195, #11647, #3969, #16912, #19307, #11807, #32584, #32247, #911, #1086, #24762, #8914, #14368, #24590, #22360, #16745, #3462, #9252, #19646, #22031, #32749, #19814, #32412, #6700, #1416, #17090, #27476, #11309, #16405, #9079, #30207, #26798, #21694, #16577, #32086, #8748, #29697, #26968, #19137, #29531, #3630, #11478, #14023, #6355, #24422, #21856, #27146, #3806, #14195, #1249, #25087, #33267, #20147, #33608, #2439, #17943, #10110, #30892, #27807, #2100, #30543, #20317, #14695, #12647, #23042, #23213, #7381, #20488, #4814, #22707, #7040, #9934, #7206, #17760, #17592, #7556, #28331, #6864, #22876, #2265, #20666, #33095, #14863, #12144, #4989, #25259, #1925, #10287, #1745, #12487, #9764, #17422, #15376, #27983, #28158, #15034, #17253, #32924, #22539, #27640, #15208, #4650, #9583, #30721, #25768, #25426, #25599, #4474, #33438, #12820, #4309, #12311, #19977, #30378, #31711, #18605, #2608, #52, #21315, #12994, #26109, #13483, #3093, #23875, #547, #31225, #31549, #23711, #706, #16039, #31060, #5484, #10939, #28992, #5651, #26268, #8217, #3256, #8383, #18771, #26430, #2936, #29154, #24038, #13319, #5805, #16202, #26591, #13644, #28500, #7719, #372, #11108, #18105, #5153, #20822, #15541, #23388, #10614, #7889, #25933, #10448, #18270, #15707, #28659, #23548, #5318, #2777, #13156, #217, #20989, #31385, #8056, #10776, #18439, #28828, #15873, #21151, #25166, #12224, #8708, #16704, #1045, #1201, #29327, #27728, #4387, #4563, #21988, #1833, #19430, #3590, #21650, #24547, #21814, #32374, #11437, #22612, #9667, #21487, #3766, #17338, #2006, #13983, #29486, #26757, #32999, #6142, #16535, #14950, #16363, #27105, #24380, #32045, #20060, #8869, #9038, #29660, #31871, #13816, #3421, #8536, #29834, #32206, #24209, #14151, #30459, #19267, #6309, #19098, #6948, #11600, #25337, #26932, #14773, #7119, #17500, #27888, #872, #11268, #18932, #5975, #7460, #28581, #18188, #5231, #15618, #12564, #12901, #5067, #15788, #31133, #12396, #20572, #26022, #32588, #20737, #7635, #23297, #18351, #2695, #4899, #10363, #30976, #31304, #12738, #33183, #22956, #7798, #15461, #26179, #13071, #22791, #18018, #23462, #128, #10529, #28409, #20909, #28743, #7967, #15285, #5403, #25854, #9846, #23127, #20228, #30628, #7297, #2515, #17676, #28063, #4725, #15115, #25510, #2179, #33352, #10025, #20405, #30799, #17843, #28243, #25680, #2348, #33515, #10191, #16112, #3011, #16615, #23629, #952, #21232, #10686, #29073, #26350, #13899, #291, #13392, #3337, #23791, #21068, #29238, #26507, #29575, #32121, #24279, #6055, #26843, #460, #31788, #3177, #16286, #31470, #8621, #19017, #19180, #13722, #16447, #792, #18683, #10859, #5889, #13568, #24121, #23958, #3506, #11350, #2848, #18843, #31952, #13233, #5723, #31627, #8137, #21732, #8296, #620, #6227, #18521, #8455, #11019, #21399, #8785, #26675, #11181, #21559, #28905, #5561, #15953, #29405, #27517, #6569, #29738, #19683, #4351, #24801, #4014, #24633, #24971, #16952, #20023, #27187, #11688, #25126, #27688, #14570, #32295, #6404, #17301, #8956, #22070, #9464, #32793, #19851, #30248, #3842, #14735, #1789, #4175, #24462, #12189, #30424, #16786, #22578, #32963, #1124, #6908, #6741, #30077, #17131, #9626, #22238, #1624, #12015, #29916, #22401, #7082, #9122, #11517, #32453, #27011, #19520, #3672, #32628, #14065, #11853, #27348, #19345, #21898, #14234, #14408, #1457, #1297, #9289, #22918, #14911, #22753, #2144, #30762, #12862, #4521, #12529, #28202, #20189, #25302, #31099, #10148, #90, #7419, #4861, #1966, #28547, #12357, #2308, #17638, #13034, #15249, #33146, #30935, #25471, #9980, #2651, #20700, #9809, #23254, #20367, #30588, #20529, #15578, #7253, #4689, #17981, #7599, #33479, #28024, #15075, #17805, #25642, #33310, #12694, #23427, #25978, #33648, #7760, #23090, #10328, #10490, #18152, #28373, #5193, #20870, #17464, #5030, #15420, #31269, #25817, #2480, #27848, #26310, #21194, #5851, #26802, #8099, #7930, #23918, #260, #8585, #21524, #23753, #583, #31589, #10977, #5362, #13683, #5521, #8254, #18981, #10820, #913, #16408 ),
 ( #11312, #2813, #3140, #417, #18482, #6017, #29036, #29199, #16078, #18311, #10655, #13195, #21697, #8420, #18643, #21029, #21355, #29373, #5689, #26470, #15912, #16250, #13526, #28702, #28865, #2979, #3466, #13861, #26636, #23595, #31429, #31913, #13358, #31752, #24081, #750, #11149, #24246, #18806, #3298, #15750, #26145, #17097, #32088, #6535, #24930, #19650, #6705, #27311, #9256, #4314, #11979, #24593, #30040, #16915, #17257, #32417, #19139, #14529, #27481, #3973, #30212, #25091, #14374, #22364, #32590, #4137, #1589, #29534, #8751, #24765, #32753, #6191, #9424, #21859, #14699, #3632, #11651, #32250, #12148, #16579, #6869, #16748, #26970, #1254, #8919, #19818, #14026, #19310, #27645, #29699, #24425, #1420, #22034, #1749, #1089, #11480, #6357, #27150, #3808, #11812, #9082, #22200, #14197, #19478, #29878, #5157, #23049, #25774, #20493, #4654, #22711, #25604, #22880, #33443, #2105, #12491, #15212, #19982, #28337, #20150, #33271, #33612, #25430, #15545, #31065, #25937, #1929, #14867, #33100, #10291, #20670, #10114, #30383, #7723, #2612, #12316, #18109, #28505, #7044, #2445, #2269, #12651, #30896, #4993, #17765, #7561, #17947, #9939, #15380, #12825, #15038, #17427, #7210, #23216, #17597, #22544, #28162, #32928, #7385, #20323, #25264, #9587, #9768, #27988, #30725, #27811, #4478, #4819, #30548, #18274, #31390, #26272, #8387, #56, #8060, #23716, #15712, #20826, #26597, #5656, #29334, #2941, #377, #10452, #24043, #31231, #31553, #13161, #8542, #10780, #7893, #26434, #20993, #5489, #31876, #16208, #28663, #18775, #15878, #5322, #16043, #11114, #26113, #223, #13487, #3099, #28996, #2781, #10619, #13324, #21156, #18444, #28832, #18937, #21492, #29158, #3261, #8221, #5811, #5980, #13650, #18610, #711, #16369, #12998, #23552, #23880, #26763, #551, #21319, #23392, #10944, #31715, #1379, #22326, #3595, #3426, #19435, #29493, #4096, #17047, #19272, #29839, #11767, #26937, #19775, #8714, #16709, #13989, #17213, #24214, #1547, #21821, #11274, #29665, #24385, #14486, #877, #1051, #3930, #11442, #21655, #6499, #27111, #30171, #32714, #24886, #6660, #27443, #32211, #32380, #3773, #16877, #32051, #9220, #19609, #6829, #14328, #11945, #22157, #6315, #8875, #27272, #14157, #24723, #24553, #9381, #13822, #19104, #32545, #30001, #6147, #1210, #11605, #16541, #21995, #9043, #25223, #17901, #12109, #4617, #12273, #30337, #33404, #7170, #20279, #17555, #27601, #19939, #32887, #4269, #30685, #20113, #7003, #12449, #10076, #14999, #27947, #14826, #7348, #30505, #14662, #27772, #22665, #7517, #20454, #17728, #17389, #4437, #30852, #1888, #33054, #2227, #15170, #12610, #23007, #9722, #28114, #22838, #25056, #25563, #1710, #33230, #28295, #4775, #4949, #9896, #22500, #9547, #25387, #2060, #1490, #32486, #9491, #24663, #11382, #6772, #19711, #29943, #22433, #17331, #6599, #14605, #24826, #11885, #27542, #21761, #24315, #16981, #25000, #985, #4207, #24490, #22270, #27377, #27721, #9320, #32151, #9154, #17156, #32655, #30108, #19549, #1651, #30275, #12046, #16818, #32825, #4043, #19879, #1326, #8811, #6941, #4381, #14433, #19211, #29610, #6258, #16644, #27044, #3707, #14096, #1152, #11544, #21929, #32322, #8988, #19375, #29771, #6437, #27214, #3870, #14262, #11714, #22099, #12893, #33175, #22605, #7288, #4555, #25848, #12217, #14943, #15279, #25330, #32992, #7452, #28056, #7791, #10356, #2509, #18011, #5061, #1997, #10017, #4716, #28236, #9660, #20564, #30968, #31127, #25673, #28402, #12732, #30620, #12387, #17834, #15108, #2342, #25502, #15454, #23289, #14764, #30791, #10181, #28575, #17668, #22784, #20053, #33682, #9840, #20221, #18182, #30452, #20398, #2172, #12557, #20730, #22949, #23121, #33345, #25157, #7113, #17493, #1824, #33508, #4892, #27879, #7628, #7109, #31517, #19232, #8347, #32007, #27064, #18736, #3224, #21612, #8830, #23839, #23678, #5940, #16007, #24336, #3557, #5770, #16331, #13611, #13947, #28956, #29122, #6102, #29452, #16499, #26898, #513, #24176, #26723, #3727, #8671, #337, #31837, #1007, #11227, #19064, #18893, #838, #29627, #11403, #16163, #21780, #8502, #6276, #24006, #10737, #32170, #16668, #29288, #21119, #8187, #3385, #18571, #5615, #26399, #3057, #13445, #10906, #13780, #21283, #31677, #26554, #669, #11072, #21453, #27397, #14281, #28380, #1168, #12701, #32506 ) ),
 .UNSPECIFIED., .F., .F., .T. ) 
 B_SPLINE_SURFACE_WITH_KNOTS ( ( 2, 2 ),
 ( 3, 2, 2, 2, 2, 2, 2, 2, 2, 2, 2, 2, 2, 2, 2, 2, 2, 2, 2, 2, 2, 2, 2, 2, 2, 2, 2, 2, 2, 2, 2, 2, 2, 2, 2, 2, 2, 2, 2, 2, 2, 2, 2, 2, 2, 2, 2, 2, 2, 2, 2, 2, 2, 2, 2, 2, 2, 2, 2, 2, 2, 2, 2, 2, 2, 2, 2, 2, 2, 2, 2, 2, 2, 2, 2, 2, 2, 2, 2, 2, 2, 2, 2, 2, 2, 2, 2, 2, 2, 2, 2, 2, 2, 2, 2, 2, 2, 2, 2, 2, 2, 2, 2, 2, 2, 2, 2, 2, 2, 2, 2, 2, 2, 2, 2, 2, 2, 2, 2, 2, 2, 2, 2, 2, 2, 2, 2, 2, 2, 2, 2, 2, 2, 2, 2, 2, 2, 2, 2, 2, 2, 2, 2, 2, 2, 2, 2, 2, 2, 2, 2, 2, 2, 2, 2, 2, 2, 2, 2, 2, 2, 2, 2, 2, 2, 2, 2, 2, 2, 2, 2, 2, 2, 2, 2, 2, 2, 2, 2, 2, 2, 2, 2, 2, 2, 2, 2, 2, 2, 2, 2, 2, 2, 2, 2, 2, 2, 2, 2, 2, 2, 2, 2, 2, 2, 2, 2, 2, 2, 2, 2, 2, 2, 2, 2, 2, 2, 2, 2, 2, 2, 2, 2, 2, 2, 2, 2, 2, 2, 2, 2, 2, 2, 2, 2, 2, 2, 2, 2, 2, 2, 2, 2, 2, 2, 2, 2, 2, 2, 2, 2, 2, 2, 2, 2, 2, 2, 2, 2, 2, 2, 2, 2, 2, 2, 2, 2, 2, 2, 2, 2, 2, 2, 2, 2, 3 ),
 ( 0.000000000000000000, 1.000000000000000000 ),
 ( 0.000000000000000000, 0.003571428571428571317, 0.007142857142857142634, 0.01071428571428571438, 0.01428571428571428527, 0.01785714285714285615, 0.02142857142857142877, 0.02500000000000000139, 0.02857142857142857054, 0.03214285714285713969, 0.03571428571428571230, 0.03928571428571428492, 0.04285714285714285754, 0.04642857142857143016, 0.05000000000000000278, 0.05357142857142856845, 0.05714285714285714107, 0.06071428571428571369, 0.06428571428571427937, 0.06785714285714285199, 0.07142857142857142461, 0.07499999999999999722, 0.07857142857142856984, 0.08214285714285714246, 0.08571428571428571508, 0.08928571428571428770, 0.09285714285714286031, 0.09642857142857143293, 0.1000000000000000056, 0.1035714285714285782, 0.1071428571428571369, 0.1107142857142857095, 0.1142857142857142821, 0.1178571428571428548, 0.1214285714285714274, 0.1250000000000000000, 0.1285714285714285587, 0.1321428571428571452, 0.1357142857142857040, 0.1392857142857142905, 0.1428571428571428492, 0.1464285714285714357, 0.1499999999999999944, 0.1535714285714285809, 0.1571428571428571397, 0.1607142857142857262, 0.1642857142857142849, 0.1678571428571428437, 0.1714285714285714302, 0.1749999999999999889, 0.1785714285714285754, 0.1821428571428571341, 0.1857142857142857206, 0.1892857142857142794, 0.1928571428571428659, 0.1964285714285714246, 0.2000000000000000111, 0.2035714285714285698, 0.2071428571428571563, 0.2107142857142857151, 0.2142857142857142738, 0.2178571428571428603, 0.2214285714285714191, 0.2250000000000000056, 0.2285714285714285643, 0.2321428571428571508, 0.2357142857142857095, 0.2392857142857142960, 0.2428571428571428548, 0.2464285714285714413, 0.2500000000000000000, 0.2535714285714285587, 0.2571428571428571175, 0.2607142857142857317, 0.2642857142857142905, 0.2678571428571428492, 0.2714285714285714080, 0.2750000000000000222, 0.2785714285714285809, 0.2821428571428571397, 0.2857142857142856984, 0.2892857142857143127, 0.2928571428571428714, 0.2964285714285714302, 0.2999999999999999889, 0.3035714285714285476, 0.3071428571428571619, 0.3107142857142857206, 0.3142857142857142794, 0.3178571428571428381, 0.3214285714285714524, 0.3250000000000000111, 0.3285714285714285698, 0.3321428571428571286, 0.3357142857142856873, 0.3392857142857143016, 0.3428571428571428603, 0.3464285714285714191, 0.3499999999999999778, 0.3535714285714285920, 0.3571428571428571508, 0.3607142857142857095, 0.3642857142857142683, 0.3678571428571428825, 0.3714285714285714413, 0.3750000000000000000, 0.3785714285714285587, 0.3821428571428571175, 0.3857142857142857317, 0.3892857142857142905, 0.3928571428571428492, 0.3964285714285714080, 0.4000000000000000222, 0.4035714285714285809, 0.4071428571428571397, 0.4107142857142856984, 0.4142857142857143127, 0.4178571428571428714, 0.4214285714285714302, 0.4249999999999999889, 0.4285714285714285476, 0.4321428571428571619, 0.4357142857142857206, 0.4392857142857142794, 0.4428571428571428381, 0.4464285714285714524, 0.4500000000000000111, 0.4535714285714285698, 0.4571428571428571286, 0.4607142857142856873, 0.4642857142857143016, 0.4678571428571428603, 0.4714285714285714191, 0.4749999999999999778, 0.4785714285714285920, 0.4821428571428571508, 0.4857142857142857095, 0.4892857142857142683, 0.4928571428571428825, 0.4964285714285714413, 0.5000000000000000000, 0.5035714285714285587, 0.5071428571428571175, 0.5107142857142856762, 0.5142857142857142350, 0.5178571428571429047, 0.5214285714285714635, 0.5250000000000000222, 0.5285714285714285809, 0.5321428571428571397, 0.5357142857142856984, 0.5392857142857142572, 0.5428571428571428159, 0.5464285714285713746, 0.5500000000000000444, 0.5535714285714286031, 0.5571428571428571619, 0.5607142857142857206, 0.5642857142857142794, 0.5678571428571428381, 0.5714285714285713969, 0.5749999999999999556, 0.5785714285714286254, 0.5821428571428571841, 0.5857142857142857428, 0.5892857142857143016, 0.5928571428571428603, 0.5964285714285714191, 0.5999999999999999778, 0.6035714285714285365, 0.6071428571428570953, 0.6107142857142857650, 0.6142857142857143238, 0.6178571428571428825, 0.6214285714285714413, 0.6250000000000000000, 0.6285714285714285587, 0.6321428571428571175, 0.6357142857142856762, 0.6392857142857142350, 0.6428571428571429047, 0.6464285714285714635, 0.6500000000000000222, 0.6535714285714285809, 0.6571428571428571397, 0.6607142857142856984, 0.6642857142857142572, 0.6678571428571428159, 0.6714285714285713746, 0.6750000000000000444, 0.6785714285714286031, 0.6821428571428571619, 0.6857142857142857206, 0.6892857142857142794, 0.6928571428571428381, 0.6964285714285713969, 0.6999999999999999556, 0.7035714285714286254, 0.7071428571428571841, 0.7107142857142857428, 0.7142857142857143016, 0.7178571428571428603, 0.7214285714285714191, 0.7249999999999999778, 0.7285714285714285365, 0.7321428571428570953, 0.7357142857142857650, 0.7392857142857143238, 0.7428571428571428825, 0.7464285714285714413, 0.7500000000000000000, 0.7535714285714285587, 0.7571428571428571175, 0.7607142857142856762, 0.7642857142857142350, 0.7678571428571429047, 0.7714285714285714635, 0.7750000000000000222, 0.7785714285714285809, 0.7821428571428571397, 0.7857142857142856984, 0.7892857142857142572, 0.7928571428571428159, 0.7964285714285713746, 0.8000000000000000444, 0.8035714285714286031, 0.8071428571428571619, 0.8107142857142857206, 0.8142857142857142794, 0.8178571428571428381, 0.8214285714285713969, 0.8249999999999999556, 0.8285714285714286254, 0.8321428571428571841, 0.8357142857142857428, 0.8392857142857143016, 0.8428571428571428603, 0.8464285714285714191, 0.8499999999999999778, 0.8535714285714285365, 0.8571428571428570953, 0.8607142857142857650, 0.8642857142857143238, 0.8678571428571428825, 0.8714285714285714413, 0.8750000000000000000, 0.8785714285714285587, 0.8821428571428571175, 0.8857142857142856762, 0.8892857142857142350, 0.8928571428571429047, 0.8964285714285714635, 0.9000000000000000222, 0.9035714285714285809, 0.9071428571428571397, 0.9107142857142856984, 0.9142857142857142572, 0.9178571428571428159, 0.9214285714285713746, 0.9250000000000000444, 0.9285714285714286031, 0.9321428571428571619, 0.9357142857142857206, 0.9392857142857142794, 0.9428571428571428381, 0.9464285714285713969, 0.9499999999999999556, 0.9535714285714286254, 0.9571428571428571841, 0.9607142857142857428, 0.9642857142857143016, 0.9678571428571428603, 0.9714285714285714191, 0.9749999999999999778, 0.9785714285714285365, 0.9821428571428570953 ),
 .UNSPECIFIED. ) 
 GEOMETRIC_REPRESENTATION_ITEM ( )  RATIONAL_B_SPLINE_SURFACE ( (
 ( 1.000000000000000000, 0.9510565162951535312, 1.000000000000000000, 0.9510565162951535312, 1.000000000000000000, 0.9510565162951535312, 1.000000000000000000, 0.9510565162951535312, 1.000000000000000000, 0.9510565162951535312, 1.000000000000000000, 0.9510565162951535312, 1.000000000000000000, 0.9510565162951535312, 1.000000000000000000, 0.9510565162951535312, 1.000000000000000000, 0.9510565162951535312, 1.000000000000000000, 0.9510565162951535312, 1.000000000000000000, 0.9510565162951535312, 1.000000000000000000, 0.9510565162951535312, 1.000000000000000000, 0.9510565162951535312, 1.000000000000000000, 0.9510565162951535312, 1.000000000000000000, 0.9510565162951535312, 1.000000000000000000, 0.9510565162951535312, 1.000000000000000000, 0.9510565162951535312, 1.000000000000000000, 0.9510565162951535312, 1.000000000000000000, 0.9510565162951535312, 1.000000000000000000, 0.9510565162951535312, 1.000000000000000000, 0.9510565162951535312, 1.000000000000000000, 0.9510565162951535312, 1.000000000000000000, 0.9510565162951535312, 1.000000000000000000, 0.9510565162951535312, 1.000000000000000000, 0.9510565162951535312, 1.000000000000000000, 0.9510565162951535312, 1.000000000000000000, 0.9510565162951535312, 1.000000000000000000, 0.9510565162951535312, 1.000000000000000000, 0.9510565162951535312, 1.000000000000000000, 0.9510565162951535312, 1.000000000000000000, 0.9510565162951535312, 1.000000000000000000, 0.9510565162951535312, 1.000000000000000000, 0.9510565162951535312, 1.000000000000000000, 0.9510565162951535312, 1.000000000000000000, 0.9510565162951535312, 1.000000000000000000, 0.9510565162951535312, 1.000000000000000000, 0.9510565162951535312, 1.000000000000000000, 0.9510565162951535312, 1.000000000000000000, 0.9510565162951535312, 1.000000000000000000, 0.9510565162951535312, 1.000000000000000000, 0.9510565162951535312, 1.000000000000000000, 0.9510565162951535312, 1.000000000000000000, 0.9510565162951535312, 1.000000000000000000, 0.9510565162951535312, 1.000000000000000000, 0.9510565162951535312, 1.000000000000000000, 0.9510565162951535312, 1.000000000000000000, 0.9510565162951535312, 1.000000000000000000, 0.9510565162951535312, 1.000000000000000000, 0.9510565162951535312, 1.000000000000000000, 0.9510565162951535312, 1.000000000000000000, 0.9510565162951535312, 1.000000000000000000, 0.9510565162951535312, 1.000000000000000000, 0.9510565162951535312, 1.000000000000000000, 0.9510565162951535312, 1.000000000000000000, 0.9510565162951535312, 1.000000000000000000, 0.9510565162951535312, 1.000000000000000000, 0.9510565162951535312, 1.000000000000000000, 0.9510565162951535312, 1.000000000000000000, 0.9510565162951535312, 1.000000000000000000, 0.9510565162951535312, 1.000000000000000000, 0.9510565162951535312, 1.000000000000000000, 0.9510565162951535312, 1.000000000000000000, 0.9510565162951535312, 1.000000000000000000, 0.9510565162951535312, 1.000000000000000000, 0.9510565162951535312, 1.000000000000000000, 0.9510565162951535312, 1.000000000000000000, 0.9510565162951535312, 1.000000000000000000, 0.9510565162951535312, 1.000000000000000000, 0.9510565162951535312, 1.000000000000000000, 0.9510565162951535312, 1.000000000000000000, 0.9510565162951535312, 1.000000000000000000, 0.9510565162951535312, 1.000000000000000000, 0.9510565162951535312, 1.000000000000000000, 0.9510565162951535312, 1.000000000000000000, 0.9510565162951535312, 1.000000000000000000, 0.9510565162951535312, 1.000000000000000000, 0.9510565162951535312, 1.000000000000000000, 0.9510565162951535312, 1.000000000000000000, 0.9510565162951535312, 1.000000000000000000, 0.9510565162951535312, 1.000000000000000000, 0.9510565162951535312, 1.000000000000000000, 0.9510565162951535312, 1.000000000000000000, 0.9510565162951535312, 1.000000000000000000, 0.9510565162951535312, 1.000000000000000000, 0.9510565162951535312, 1.000000000000000000, 0.9510565162951535312, 1.000000000000000000, 0.9510565162951535312, 1.000000000000000000, 0.9510565162951535312, 1.000000000000000000, 0.9510565162951535312, 1.000000000000000000, 0.9510565162951535312, 1.000000000000000000, 0.9510565162951535312, 1.000000000000000000, 0.9510565162951535312, 1.000000000000000000, 0.9510565162951535312, 1.000000000000000000, 0.9510565162951535312, 1.000000000000000000, 0.9510565162951535312, 1.000000000000000000, 0.9510565162951535312, 1.000000000000000000, 0.9510565162951535312, 1.000000000000000000, 0.9510565162951535312, 1.000000000000000000, 0.9510565162951535312, 1.000000000000000000, 0.9510565162951535312, 1.000000000000000000, 0.9510565162951535312, 1.000000000000000000, 0.9510565162951535312, 1.000000000000000000, 0.9510565162951535312, 1.000000000000000000, 0.9510565162951535312, 1.000000000000000000, 0.9510565162951535312, 1.000000000000000000, 0.9510565162951535312, 1.000000000000000000, 0.9510565162951535312, 1.000000000000000000, 0.9510565162951535312, 1.000000000000000000, 0.9510565162951535312, 1.000000000000000000, 0.9510565162951535312, 1.000000000000000000, 0.9510565162951535312, 1.000000000000000000, 0.9510565162951535312, 1.000000000000000000, 0.9510565162951535312, 1.000000000000000000, 0.9510565162951535312, 1.000000000000000000, 0.9510565162951535312, 1.000000000000000000, 0.9510565162951535312, 1.000000000000000000, 0.9510565162951535312, 1.000000000000000000, 0.9510565162951535312, 1.000000000000000000, 0.9510565162951535312, 1.000000000000000000, 0.9510565162951535312, 1.000000000000000000, 0.9510565162951535312, 1.000000000000000000, 0.9510565162951535312, 1.000000000000000000, 0.9510565162951535312, 1.000000000000000000, 0.9510565162951535312, 1.000000000000000000, 0.9510565162951535312, 1.000000000000000000, 0.9510565162951535312, 1.000000000000000000, 0.9510565162951535312, 1.000000000000000000, 0.9510565162951535312, 1.000000000000000000, 0.9510565162951535312, 1.000000000000000000, 0.9510565162951535312, 1.000000000000000000, 0.9510565162951535312, 1.000000000000000000, 0.9510565162951535312, 1.000000000000000000, 0.9510565162951535312, 1.000000000000000000, 0.9510565162951535312, 1.000000000000000000, 0.9510565162951535312, 1.000000000000000000, 0.9510565162951535312, 1.000000000000000000, 0.9510565162951535312, 1.000000000000000000, 0.9510565162951535312, 1.000000000000000000, 0.9510565162951535312, 1.000000000000000000, 0.9510565162951535312, 1.000000000000000000, 0.9510565162951535312, 1.000000000000000000, 0.9510565162951535312, 1.000000000000000000, 0.9510565162951535312, 1.000000000000000000, 0.9510565162951535312, 1.000000000000000000, 0.9510565162951535312, 1.000000000000000000, 0.9510565162951535312, 1.000000000000000000, 0.9510565162951535312, 1.000000000000000000, 0.9510565162951535312, 1.000000000000000000, 0.9510565162951535312, 1.000000000000000000, 0.9510565162951535312, 1.000000000000000000, 0.9510565162951535312, 1.000000000000000000, 0.9510565162951535312, 1.000000000000000000, 0.9510565162951535312, 1.000000000000000000, 0.9510565162951535312, 1.000000000000000000, 0.9510565162951535312, 1.000000000000000000, 0.9510565162951535312, 1.000000000000000000, 0.9510565162951535312, 1.000000000000000000, 0.9510565162951535312, 1.000000000000000000, 0.9510565162951535312, 1.000000000000000000, 0.9510565162951535312, 1.000000000000000000, 0.9510565162951535312, 1.000000000000000000, 0.9510565162951535312, 1.000000000000000000, 0.9510565162951535312, 1.000000000000000000, 0.9510565162951535312, 1.000000000000000000, 0.9510565162951535312, 1.000000000000000000, 0.9510565162951535312, 1.000000000000000000, 0.9510565162951535312, 1.000000000000000000, 0.9510565162951535312, 1.000000000000000000, 0.9510565162951535312, 1.000000000000000000, 0.9510565162951535312, 1.000000000000000000, 0.9510565162951535312, 1.000000000000000000, 0.9510565162951535312, 1.000000000000000000, 0.9510565162951535312, 1.000000000000000000, 0.9510565162951535312, 1.000000000000000000, 0.9510565162951535312, 1.000000000000000000, 0.9510565162951535312, 1.000000000000000000, 0.9510565162951535312, 1.000000000000000000, 0.9510565162951535312, 1.000000000000000000, 0.9510565162951535312, 1.000000000000000000, 0.9510565162951535312, 1.000000000000000000, 0.9510565162951535312, 1.000000000000000000, 0.9510565162951535312, 1.000000000000000000, 0.9510565162951535312, 1.000000000000000000, 0.9510565162951535312, 1.000000000000000000, 0.9510565162951535312, 1.000000000000000000, 0.9510565162951535312, 1.000000000000000000, 0.9510565162951535312, 1.000000000000000000, 0.9510565162951535312, 1.000000000000000000, 0.9510565162951535312, 1.000000000000000000, 0.9510565162951535312, 1.000000000000000000, 0.9510565162951535312, 1.000000000000000000, 0.9510565162951535312, 1.000000000000000000, 0.9510565162951535312, 1.000000000000000000, 0.9510565162951535312, 1.000000000000000000, 0.9510565162951535312, 1.000000000000000000, 0.9510565162951535312, 1.000000000000000000, 0.9510565162951535312, 1.000000000000000000, 0.9510565162951535312, 1.000000000000000000, 0.9510565162951535312, 1.000000000000000000, 0.9510565162951535312, 1.000000000000000000, 0.9510565162951535312, 1.000000000000000000, 0.9510565162951535312, 1.000000000000000000, 0.9510565162951535312, 1.000000000000000000, 0.9510565162951535312, 1.000000000000000000, 0.9510565162951535312, 1.000000000000000000, 0.9510565162951535312, 1.000000000000000000, 0.9510565162951535312, 1.000000000000000000, 0.9510565162951535312, 1.000000000000000000, 0.9510565162951535312, 1.000000000000000000, 0.9510565162951535312, 1.000000000000000000, 0.9510565162951535312, 1.000000000000000000, 0.9510565162951535312, 1.000000000000000000, 0.9510565162951535312, 1.000000000000000000, 0.9510565162951535312, 1.000000000000000000, 0.9510565162951535312, 1.000000000000000000, 0.9510565162951535312, 1.000000000000000000, 0.9510565162951535312, 1.000000000000000000, 0.9510565162951535312, 1.000000000000000000, 0.9510565162951535312, 1.000000000000000000, 0.9510565162951535312, 1.000000000000000000, 0.9510565162951535312, 1.000000000000000000, 0.9510565162951535312, 1.000000000000000000, 0.9510565162951535312, 1.000000000000000000, 0.9510565162951535312, 1.000000000000000000, 0.9510565162951535312, 1.000000000000000000, 0.9510565162951535312, 1.000000000000000000, 0.9510565162951535312, 1.000000000000000000, 0.9510565162951535312, 1.000000000000000000, 0.9510565162951535312, 1.000000000000000000, 0.9510565162951535312, 1.000000000000000000, 0.9510565162951535312, 1.000000000000000000, 0.9510565162951535312, 1.000000000000000000, 0.9510565162951535312, 1.000000000000000000, 0.9510565162951535312, 1.000000000000000000, 0.9510565162951535312, 1.000000000000000000, 0.9510565162951535312, 1.000000000000000000, 0.9510565162951535312, 1.000000000000000000, 0.9510565162951535312, 1.000000000000000000, 0.9510565162951535312, 1.000000000000000000, 0.9510565162951535312, 1.000000000000000000, 0.9510565162951535312, 1.000000000000000000, 0.9510565162951535312, 1.000000000000000000, 0.9510565162951535312, 1.000000000000000000, 0.9510565162951535312, 1.000000000000000000, 0.9510565162951535312, 1.000000000000000000, 0.9510565162951535312, 1.000000000000000000, 0.9510565162951535312, 1.000000000000000000, 0.9510565162951535312, 1.000000000000000000, 0.9510565162951535312, 1.000000000000000000, 0.9510565162951535312, 1.000000000000000000, 0.9510565162951535312, 1.000000000000000000, 0.9510565162951535312, 1.000000000000000000, 0.9510565162951535312, 1.000000000000000000, 0.9510565162951535312, 1.000000000000000000, 0.9510565162951535312, 1.000000000000000000, 0.9510565162951535312, 1.000000000000000000, 0.9510565162951535312, 1.000000000000000000, 0.9510565162951535312, 1.000000000000000000, 0.9510565162951535312, 1.000000000000000000, 0.9510565162951535312, 1.000000000000000000, 0.9510565162951535312, 1.000000000000000000, 0.9510565162951535312, 1.000000000000000000, 0.9510565162951535312, 1.000000000000000000, 0.9510565162951535312, 1.000000000000000000, 0.9510565162951535312, 1.000000000000000000, 0.9510565162951535312, 1.000000000000000000, 0.9510565162951535312, 1.000000000000000000, 0.9510565162951535312, 1.000000000000000000, 0.9510565162951535312, 1.000000000000000000, 0.9510565162951535312, 1.000000000000000000, 0.9510565162951535312, 1.000000000000000000, 0.9510565162951535312, 1.000000000000000000, 0.9510565162951535312, 1.000000000000000000, 0.9510565162951535312, 1.000000000000000000, 0.9510565162951535312, 1.000000000000000000),
 ( 1.000000000000000000, 0.9510565162951535312, 1.000000000000000000, 0.9510565162951535312, 1.000000000000000000, 0.9510565162951535312, 1.000000000000000000, 0.9510565162951535312, 1.000000000000000000, 0.9510565162951535312, 1.000000000000000000, 0.9510565162951535312, 1.000000000000000000, 0.9510565162951535312, 1.000000000000000000, 0.9510565162951535312, 1.000000000000000000, 0.9510565162951535312, 1.000000000000000000, 0.9510565162951535312, 1.000000000000000000, 0.9510565162951535312, 1.000000000000000000, 0.9510565162951535312, 1.000000000000000000, 0.9510565162951535312, 1.000000000000000000, 0.9510565162951535312, 1.000000000000000000, 0.9510565162951535312, 1.000000000000000000, 0.9510565162951535312, 1.000000000000000000, 0.9510565162951535312, 1.000000000000000000, 0.9510565162951535312, 1.000000000000000000, 0.9510565162951535312, 1.000000000000000000, 0.9510565162951535312, 1.000000000000000000, 0.9510565162951535312, 1.000000000000000000, 0.9510565162951535312, 1.000000000000000000, 0.9510565162951535312, 1.000000000000000000, 0.9510565162951535312, 1.000000000000000000, 0.9510565162951535312, 1.000000000000000000, 0.9510565162951535312, 1.000000000000000000, 0.9510565162951535312, 1.000000000000000000, 0.9510565162951535312, 1.000000000000000000, 0.9510565162951535312, 1.000000000000000000, 0.9510565162951535312, 1.000000000000000000, 0.9510565162951535312, 1.000000000000000000, 0.9510565162951535312, 1.000000000000000000, 0.9510565162951535312, 1.000000000000000000, 0.9510565162951535312, 1.000000000000000000, 0.9510565162951535312, 1.000000000000000000, 0.9510565162951535312, 1.000000000000000000, 0.9510565162951535312, 1.000000000000000000, 0.9510565162951535312, 1.000000000000000000, 0.9510565162951535312, 1.000000000000000000, 0.9510565162951535312, 1.000000000000000000, 0.9510565162951535312, 1.000000000000000000, 0.9510565162951535312, 1.000000000000000000, 0.9510565162951535312, 1.000000000000000000, 0.9510565162951535312, 1.000000000000000000, 0.9510565162951535312, 1.000000000000000000, 0.9510565162951535312, 1.000000000000000000, 0.9510565162951535312, 1.000000000000000000, 0.9510565162951535312, 1.000000000000000000, 0.9510565162951535312, 1.000000000000000000, 0.9510565162951535312, 1.000000000000000000, 0.9510565162951535312, 1.000000000000000000, 0.9510565162951535312, 1.000000000000000000, 0.9510565162951535312, 1.000000000000000000, 0.9510565162951535312, 1.000000000000000000, 0.9510565162951535312, 1.000000000000000000, 0.9510565162951535312, 1.000000000000000000, 0.9510565162951535312, 1.000000000000000000, 0.9510565162951535312, 1.000000000000000000, 0.9510565162951535312, 1.000000000000000000, 0.9510565162951535312, 1.000000000000000000, 0.9510565162951535312, 1.000000000000000000, 0.9510565162951535312, 1.000000000000000000, 0.9510565162951535312, 1.000000000000000000, 0.9510565162951535312, 1.000000000000000000, 0.9510565162951535312, 1.000000000000000000, 0.9510565162951535312, 1.000000000000000000, 0.9510565162951535312, 1.000000000000000000, 0.9510565162951535312, 1.000000000000000000, 0.9510565162951535312, 1.000000000000000000, 0.9510565162951535312, 1.000000000000000000, 0.9510565162951535312, 1.000000000000000000, 0.9510565162951535312, 1.000000000000000000, 0.9510565162951535312, 1.000000000000000000, 0.9510565162951535312, 1.000000000000000000, 0.9510565162951535312, 1.000000000000000000, 0.9510565162951535312, 1.000000000000000000, 0.9510565162951535312, 1.000000000000000000, 0.9510565162951535312, 1.000000000000000000, 0.9510565162951535312, 1.000000000000000000, 0.9510565162951535312, 1.000000000000000000, 0.9510565162951535312, 1.000000000000000000, 0.9510565162951535312, 1.000000000000000000, 0.9510565162951535312, 1.000000000000000000, 0.9510565162951535312, 1.000000000000000000, 0.9510565162951535312, 1.000000000000000000, 0.9510565162951535312, 1.000000000000000000, 0.9510565162951535312, 1.000000000000000000, 0.9510565162951535312, 1.000000000000000000, 0.9510565162951535312, 1.000000000000000000, 0.9510565162951535312, 1.000000000000000000, 0.9510565162951535312, 1.000000000000000000, 0.9510565162951535312, 1.000000000000000000, 0.9510565162951535312, 1.000000000000000000, 0.9510565162951535312, 1.000000000000000000, 0.9510565162951535312, 1.000000000000000000, 0.9510565162951535312, 1.000000000000000000, 0.9510565162951535312, 1.000000000000000000, 0.9510565162951535312, 1.000000000000000000, 0.9510565162951535312, 1.000000000000000000, 0.9510565162951535312, 1.000000000000000000, 0.9510565162951535312, 1.000000000000000000, 0.9510565162951535312, 1.000000000000000000, 0.9510565162951535312, 1.000000000000000000, 0.9510565162951535312, 1.000000000000000000, 0.9510565162951535312, 1.000000000000000000, 0.9510565162951535312, 1.000000000000000000, 0.9510565162951535312, 1.000000000000000000, 0.9510565162951535312, 1.000000000000000000, 0.9510565162951535312, 1.000000000000000000, 0.9510565162951535312, 1.000000000000000000, 0.9510565162951535312, 1.000000000000000000, 0.9510565162951535312, 1.000000000000000000, 0.9510565162951535312, 1.000000000000000000, 0.9510565162951535312, 1.000000000000000000, 0.9510565162951535312, 1.000000000000000000, 0.9510565162951535312, 1.000000000000000000, 0.9510565162951535312, 1.000000000000000000, 0.9510565162951535312, 1.000000000000000000, 0.9510565162951535312, 1.000000000000000000, 0.9510565162951535312, 1.000000000000000000, 0.9510565162951535312, 1.000000000000000000, 0.9510565162951535312, 1.000000000000000000, 0.9510565162951535312, 1.000000000000000000, 0.9510565162951535312, 1.000000000000000000, 0.9510565162951535312, 1.000000000000000000, 0.9510565162951535312, 1.000000000000000000, 0.9510565162951535312, 1.000000000000000000, 0.9510565162951535312, 1.000000000000000000, 0.9510565162951535312, 1.000000000000000000, 0.9510565162951535312, 1.000000000000000000, 0.9510565162951535312, 1.000000000000000000, 0.9510565162951535312, 1.000000000000000000, 0.9510565162951535312, 1.000000000000000000, 0.9510565162951535312, 1.000000000000000000, 0.9510565162951535312, 1.000000000000000000, 0.9510565162951535312, 1.000000000000000000, 0.9510565162951535312, 1.000000000000000000, 0.9510565162951535312, 1.000000000000000000, 0.9510565162951535312, 1.000000000000000000, 0.9510565162951535312, 1.000000000000000000, 0.9510565162951535312, 1.000000000000000000, 0.9510565162951535312, 1.000000000000000000, 0.9510565162951535312, 1.000000000000000000, 0.9510565162951535312, 1.000000000000000000, 0.9510565162951535312, 1.000000000000000000, 0.9510565162951535312, 1.000000000000000000, 0.9510565162951535312, 1.000000000000000000, 0.9510565162951535312, 1.000000000000000000, 0.9510565162951535312, 1.000000000000000000, 0.9510565162951535312, 1.000000000000000000, 0.9510565162951535312, 1.000000000000000000, 0.9510565162951535312, 1.000000000000000000, 0.9510565162951535312, 1.000000000000000000, 0.9510565162951535312, 1.000000000000000000, 0.9510565162951535312, 1.000000000000000000, 0.9510565162951535312, 1.000000000000000000, 0.9510565162951535312, 1.000000000000000000, 0.9510565162951535312, 1.000000000000000000, 0.9510565162951535312, 1.000000000000000000, 0.9510565162951535312, 1.000000000000000000, 0.9510565162951535312, 1.000000000000000000, 0.9510565162951535312, 1.000000000000000000, 0.9510565162951535312, 1.000000000000000000, 0.9510565162951535312, 1.000000000000000000, 0.9510565162951535312, 1.000000000000000000, 0.9510565162951535312, 1.000000000000000000, 0.9510565162951535312, 1.000000000000000000, 0.9510565162951535312, 1.000000000000000000, 0.9510565162951535312, 1.000000000000000000, 0.9510565162951535312, 1.000000000000000000, 0.9510565162951535312, 1.000000000000000000, 0.9510565162951535312, 1.000000000000000000, 0.9510565162951535312, 1.000000000000000000, 0.9510565162951535312, 1.000000000000000000, 0.9510565162951535312, 1.000000000000000000, 0.9510565162951535312, 1.000000000000000000, 0.9510565162951535312, 1.000000000000000000, 0.9510565162951535312, 1.000000000000000000, 0.9510565162951535312, 1.000000000000000000, 0.9510565162951535312, 1.000000000000000000, 0.9510565162951535312, 1.000000000000000000, 0.9510565162951535312, 1.000000000000000000, 0.9510565162951535312, 1.000000000000000000, 0.9510565162951535312, 1.000000000000000000, 0.9510565162951535312, 1.000000000000000000, 0.9510565162951535312, 1.000000000000000000, 0.9510565162951535312, 1.000000000000000000, 0.9510565162951535312, 1.000000000000000000, 0.9510565162951535312, 1.000000000000000000, 0.9510565162951535312, 1.000000000000000000, 0.9510565162951535312, 1.000000000000000000, 0.9510565162951535312, 1.000000000000000000, 0.9510565162951535312, 1.000000000000000000, 0.9510565162951535312, 1.000000000000000000, 0.9510565162951535312, 1.000000000000000000, 0.9510565162951535312, 1.000000000000000000, 0.9510565162951535312, 1.000000000000000000, 0.9510565162951535312, 1.000000000000000000, 0.9510565162951535312, 1.000000000000000000, 0.9510565162951535312, 1.000000000000000000, 0.9510565162951535312, 1.000000000000000000, 0.9510565162951535312, 1.000000000000000000, 0.9510565162951535312, 1.000000000000000000, 0.9510565162951535312, 1.000000000000000000, 0.9510565162951535312, 1.000000000000000000, 0.9510565162951535312, 1.000000000000000000, 0.9510565162951535312, 1.000000000000000000, 0.9510565162951535312, 1.000000000000000000, 0.9510565162951535312, 1.000000000000000000, 0.9510565162951535312, 1.000000000000000000, 0.9510565162951535312, 1.000000000000000000, 0.9510565162951535312, 1.000000000000000000, 0.9510565162951535312, 1.000000000000000000, 0.9510565162951535312, 1.000000000000000000, 0.9510565162951535312, 1.000000000000000000, 0.9510565162951535312, 1.000000000000000000, 0.9510565162951535312, 1.000000000000000000, 0.9510565162951535312, 1.000000000000000000, 0.9510565162951535312, 1.000000000000000000, 0.9510565162951535312, 1.000000000000000000, 0.9510565162951535312, 1.000000000000000000, 0.9510565162951535312, 1.000000000000000000, 0.9510565162951535312, 1.000000000000000000, 0.9510565162951535312, 1.000000000000000000, 0.9510565162951535312, 1.000000000000000000, 0.9510565162951535312, 1.000000000000000000, 0.9510565162951535312, 1.000000000000000000, 0.9510565162951535312, 1.000000000000000000, 0.9510565162951535312, 1.000000000000000000, 0.9510565162951535312, 1.000000000000000000, 0.9510565162951535312, 1.000000000000000000, 0.9510565162951535312, 1.000000000000000000, 0.9510565162951535312, 1.000000000000000000, 0.9510565162951535312, 1.000000000000000000, 0.9510565162951535312, 1.000000000000000000, 0.9510565162951535312, 1.000000000000000000, 0.9510565162951535312, 1.000000000000000000, 0.9510565162951535312, 1.000000000000000000, 0.9510565162951535312, 1.000000000000000000, 0.9510565162951535312, 1.000000000000000000, 0.9510565162951535312, 1.000000000000000000, 0.9510565162951535312, 1.000000000000000000, 0.9510565162951535312, 1.000000000000000000, 0.9510565162951535312, 1.000000000000000000, 0.9510565162951535312, 1.000000000000000000, 0.9510565162951535312, 1.000000000000000000, 0.9510565162951535312, 1.000000000000000000, 0.9510565162951535312, 1.000000000000000000, 0.9510565162951535312, 1.000000000000000000, 0.9510565162951535312, 1.000000000000000000, 0.9510565162951535312, 1.000000000000000000, 0.9510565162951535312, 1.000000000000000000, 0.9510565162951535312, 1.000000000000000000, 0.9510565162951535312, 1.000000000000000000, 0.9510565162951535312, 1.000000000000000000, 0.9510565162951535312, 1.000000000000000000, 0.9510565162951535312, 1.000000000000000000, 0.9510565162951535312, 1.000000000000000000, 0.9510565162951535312, 1.000000000000000000, 0.9510565162951535312, 1.000000000000000000, 0.9510565162951535312, 1.000000000000000000, 0.9510565162951535312, 1.000000000000000000, 0.9510565162951535312, 1.000000000000000000, 0.9510565162951535312, 1.000000000000000000, 0.9510565162951535312, 1.000000000000000000, 0.9510565162951535312, 1.000000000000000000, 0.9510565162951535312, 1.000000000000000000, 0.9510565162951535312, 1.000000000000000000, 0.9510565162951535312, 1.000000000000000000, 0.9510565162951535312, 1.000000000000000000, 0.9510565162951535312, 1.000000000000000000, 0.9510565162951535312, 1.000000000000000000, 0.9510565162951535312, 1.000000000000000000, 0.9510565162951535312, 1.000000000000000000, 0.9510565162951535312, 1.000000000000000000) ) ) 
 REPRESENTATION_ITEM ( '' )  SURFACE ( )  );
#29805 = CARTESIAN_POINT ( 'NONE',  ( 0.05014649552810505201, 217.5146222423826714, 70.25113791807858377 ) ) ;
#29806 = CARTESIAN_POINT ( 'NONE',  ( -10.01549611932653860, 203.7984951890123000, 36.35113791807857098 ) ) ;
#29807 = AXIS2_PLACEMENT_3D ( 'NONE', #24691, #1852, #32679 ) ;
#29808 = DIRECTION ( 'NONE',  ( 0.000000000000000000, 0.000000000000000000, 1.000000000000000000 ) ) ;
#29809 = DIRECTION ( 'NONE',  ( 0.000000000000000000, 1.224646799147353207E-16, 1.000000000000000000 ) ) ;
#29810 = CARTESIAN_POINT ( 'NONE',  ( -9.680171189290716072, 199.9079932115567146, 8.198862081921433287 ) ) ;
#29811 = CARTESIAN_POINT ( 'NONE',  ( 3.044812012439969795, 216.5253028482143520, 12.39886208192143435 ) ) ;
#29812 = CARTESIAN_POINT ( 'NONE',  ( 69.69999999453762030, 142.6655632788954620, -8.961492836873480528 ) ) ;
#29813 = ORIENTED_EDGE ( 'NONE', *, *, #17958, .T. ) ;
#29814 = CARTESIAN_POINT ( 'NONE',  ( -0.05014649552807705357, 194.3824533091408000, 50.75113791807857666 ) ) ;
#29815 = CARTESIAN_POINT ( 'NONE',  ( -4.984841277089726574, 200.2242689037092305, 72.05113791807858092 ) ) ;
#29816 = CARTESIAN_POINT ( 'NONE',  ( 6.139770520408223575, 215.5359834540460611, 33.54886208192143471 ) ) ;
#29817 = CARTESIAN_POINT ( 'NONE',  ( 3.528928113779637776, -5.468125903023631551, -5.911160594572010107E-15 ) ) ;
#29818 = EDGE_LOOP ( 'NONE', ( #12802, #32321, #11165, #4202 ) ) ;
#29819 = CARTESIAN_POINT ( 'NONE',  ( 10.00000000000000711, 206.9523078486586201, 95.00113791807856956 ) ) ;
#29820 = CIRCLE ( 'NONE', #12403, 24.99999999999999289 ) ;
#29821 = EDGE_LOOP ( 'NONE', ( #29954, #15190, #4847, #12384, #18593 ) ) ;
#29822 = PRODUCT ( 'hex thin nut chamfered gradeab_iso_ISO - 4035 - M36 - N', 'hex thin nut chamfered gradeab_iso_ISO - 4035 - M36 - N', '', ( #31352 ) ) ;
#29823 = TOROIDAL_SURFACE ( 'NONE', #12407, 4.999999999999993783, 1.000000000000000222 ) ;
#29824 = CARTESIAN_POINT ( 'NONE',  ( 0.000000000000000000, 0.000000000000000000, 0.000000000000000000 ) ) ;
#29825 = CIRCLE ( 'NONE', #15128, 2.149999999999985256 ) ;
#29826 = DIRECTION ( 'NONE',  ( -1.000000000000000000, -0.000000000000000000, -0.000000000000000000 ) ) ;
#29827 = VERTEX_POINT ( 'NONE', #7437 ) ;
#29828 = CARTESIAN_POINT ( 'NONE',  ( 4.984841277089725686, 213.7757310962907411, 25.55113791807857027 ) ) ;
#29829 = CARTESIAN_POINT ( 'NONE',  ( 0.000000000000000000, 0.000000000000000000, -7.554475477074173106 ) ) ;
#29830 = CARTESIAN_POINT ( 'NONE',  ( 10.00000000000000711, 207.0476921513415220, 0.9988620819214343305 ) ) ;
#29831 = CARTESIAN_POINT ( 'NONE',  ( 52.57499999726881157, 145.8408176439707802, 12.60653300113718345 ) ) ;
#29833 = ORIENTED_EDGE ( 'NONE', *, *, #10224, .F. ) ;
#29832 = AXIS2_PLACEMENT_3D ( 'NONE', #22084, #9138, #14749 ) ;
#29834 = CARTESIAN_POINT ( 'NONE',  ( 58.42499999726879878, 141.7447067706911810, 9.630534252274376428 ) ) ;
#29835 = CARTESIAN_POINT ( 'NONE',  ( 2.426778023690261410, 199.3768101843759837, 47.60113791807857808 ) ) ;
#29836 = DIRECTION ( 'NONE',  ( 0.000000000000000000, 0.000000000000000000, -1.000000000000000000 ) ) ;
#29837 = CARTESIAN_POINT ( 'NONE',  ( -60.00000000000000000, -7.347880794884118356E-15, -20.00000000000000355 ) ) ;
#29838 = CARTESIAN_POINT ( 'NONE',  ( 3.135527875058981895, 197.5041725223112792, 94.59886208192143897 ) ) ;
#29839 = CARTESIAN_POINT ( 'NONE',  ( 57.67499999726880588, 168.2552932293087906, -9.630534252274385310 ) ) ;
#29840 = CARTESIAN_POINT ( 'NONE',  ( 3.044812012440130555, 197.4746971517856764, 29.60113791807856742 ) ) ;
#29841 = CARTESIAN_POINT ( 'NONE',  ( 46.88867513459483405, 159.8737954434937478, -14.99999999999993072 ) ) ;
#29842 = CARTESIAN_POINT ( 'NONE',  ( -9.736236675708031640, 214.0148392665760753, 77.79886208192142760 ) ) ;
#29843 = CARTESIAN_POINT ( 'NONE',  ( 83.10000000000000853, 168.7903194862797420, 4.480746418436729606 ) ) ;
#29844 = CARTESIAN_POINT ( 'NONE',  ( -7.703920929261754758, -4.447860822324869901, -7.917989418073284824 ) ) ;
#29845 = CARTESIAN_POINT ( 'NONE',  ( 130.2499999999999716, 2.997323040913146538E-14, 35.00000599999999906 ) ) ;
#29846 = CARTESIAN_POINT ( 'NONE',  ( 3.044812012440130555, 197.4746971517856764, 98.60113791807857808 ) ) ;
#29847 = AXIS2_PLACEMENT_3D ( 'NONE', #6352, #3804, #11476 ) ;
#29848 = DIRECTION ( 'NONE',  ( 1.000000000000000000, 0.000000000000000000, 0.000000000000000000 ) ) ;
#29849 = CARTESIAN_POINT ( 'NONE',  ( 44.37499999726881583, 155.0000000000000000, 15.58253174999999402 ) ) ;
#29850 = CARTESIAN_POINT ( 'NONE',  ( -8.118202686958039038, 201.1607312380087080, 33.20113791807857240 ) ) ;
#29851 = AXIS2_PLACEMENT_3D ( 'NONE', #28061, #33513, #26020 ) ;
#29852 = CARTESIAN_POINT ( 'NONE',  ( 84.72499999726882436, 140.1801316387863778, -4.815267126137194431 ) ) ;
#29853 = ORIENTED_EDGE ( 'NONE', *, *, #21658, .T. ) ;
#29854 = FACE_OUTER_BOUND ( 'NONE', #5273, .T. ) ;
#29855 = CARTESIAN_POINT ( 'NONE',  ( 49.61132485994281893, 150.1262045565064227, -15.00000000000002665 ) ) ;
#29856 = CARTESIAN_POINT ( 'NONE',  ( 49.49999999453763166, 139.7537977485451393, -4.138211985947621020E-15 ) ) ;
#29857 = CARTESIAN_POINT ( 'NONE',  ( 3.662846001190051659, 195.5725841191953691, 23.60113791807857098 ) ) ;
#29858 = DIRECTION ( 'NONE',  ( -1.000000000000000000, -0.000000000000000000, -0.000000000000000000 ) ) ;
#29859 = CARTESIAN_POINT ( 'NONE',  ( 125.5000000000000000, 155.0000000000000000, 100.0000000000000284 ) ) ;
#29860 = ORIENTED_EDGE ( 'NONE', *, *, #12023, .F. ) ;
#29861 = CARTESIAN_POINT ( 'NONE',  ( -9.680171189290716072, 199.9079932115567146, 47.19886208192143329 ) ) ;
#29862 = FACE_OUTER_BOUND ( 'NONE', #3364, .T. ) ;
#29863 = CARTESIAN_POINT ( 'NONE',  ( 8.062137200540920645, 201.0835637161417822, 47.30113791807857382 ) ) ;
#29864 = CARTESIAN_POINT ( 'NONE',  ( -2.517493886309087880, 214.5937144450984135, 9.098862081921435419 ) ) ;
#29865 = PRODUCT_DEFINITION_CONTEXT ( 'detailed design', #14847, 'design' ) ;
#29866 = VERTEX_POINT ( 'NONE', #7944 ) ;
#29867 = CARTESIAN_POINT ( 'NONE',  ( -4.984841277089891776, 213.7757310962905990, 95.94886208192144750 ) ) ;
#29868 = AXIS2_PLACEMENT_3D ( 'NONE', #8430, #31924, #23764 ) ;
#29869 = DIRECTION ( 'NONE',  ( -0.000000000000000000, -0.000000000000000000, 1.000000000000000000 ) ) ;
#29870 = CARTESIAN_POINT ( 'NONE',  ( -2.517493886308901807, 199.4062855549015012, 38.90113791807856813 ) ) ;
#29871 = CARTESIAN_POINT ( 'NONE',  ( 33.37499999726880873, 155.0000000000000000, -15.58253175000000823 ) ) ;
#29872 = ORIENTED_EDGE ( 'NONE', *, *, #30113, .T. ) ;
#29873 = CARTESIAN_POINT ( 'NONE',  ( 35.92499999726880588, 164.1591823560292198, 12.60653300113718167 ) ) ;
#29874 = CARTESIAN_POINT ( 'NONE',  ( 39.48867513459482126, 167.7597621252805880, 9.270509831248428867 ) ) ;
#29875 = CIRCLE ( 'NONE', #21767, 2.149999999999974598 ) ;
#29876 = ADVANCED_FACE ( 'NONE', ( #3141 ), #11313, .T. ) ;
#29877 = CARTESIAN_POINT ( 'NONE',  ( -6.139770520408224463, 198.4640165459539389, 65.04886208192144181 ) ) ;
#29878 = CARTESIAN_POINT ( 'NONE',  ( 43.87499999726880162, 171.3844434931184253, -7.942151717890132712E-15 ) ) ;
#29879 = CARTESIAN_POINT ( 'NONE',  ( -18.00000000000000000, 2.204364238465235428E-15, 3.252606517456513302E-15 ) ) ;
#29880 = CARTESIAN_POINT ( 'NONE',  ( 4.903702542908601636, 200.1653181626581102, 98.45113791807858661 ) ) ;
#29881 = ADVANCED_FACE ( 'NONE', ( #25484, #28040, #28721, #2323, #22931, #12710, #5377, #23106, #30949, #4701 ), #1981, .T. ) ;
#29882 = APPLICATION_CONTEXT ( 'automotive_design' ) ;
#29883 = AXIS2_PLACEMENT_3D ( 'NONE', #12614, #10080, #20458 ) ;
#29884 = CARTESIAN_POINT ( 'NONE',  ( 63.70000000000000995, 146.4771138417591203, 11.73074641843673227 ) ) ;
#29885 = DIRECTION ( 'NONE',  ( 0.000000000000000000, 0.000000000000000000, 1.000000000000000000 ) ) ;
#29886 = CARTESIAN_POINT ( 'NONE',  ( 2.426778023690075337, 214.6231898156240447, 78.39886208192143613 ) ) ;
#29887 = CARTESIAN_POINT ( 'NONE',  ( 77.38867513459481984, 169.2658477444273331, 4.635254915624208216 ) ) ;
#29888 = CARTESIAN_POINT ( 'NONE',  ( -2.000000000000000000, 0.000000000000000000, -2.874600000000001376 ) ) ;
#29889 = CARTESIAN_POINT ( 'NONE',  ( 58.52499999726881441, 140.1801316387863778, 4.815267126137185549 ) ) ;
#29891 = ORIENTED_EDGE ( 'NONE', *, *, #4540, .F. ) ;
#29890 = CARTESIAN_POINT ( 'NONE',  ( -3.135527875058821579, 197.5041725223112223, 23.90113791807856813 ) ) ;
#29892 = DIRECTION ( 'NONE',  ( 1.000000000000000000, 0.000000000000000000, 0.000000000000000000 ) ) ;
#29893 = CARTESIAN_POINT ( 'NONE',  ( 83.77499999726880731, 169.8198683612136222, -4.815267126137197984 ) ) ;
#29894 = CARTESIAN_POINT ( 'NONE',  ( 3.753561863808689836, 218.3979405102790565, 85.40113791807856103 ) ) ;
#29895 = AXIS2_PLACEMENT_3D ( 'NONE', #8559, #5670, #15891 ) ;
#29896 = CARTESIAN_POINT ( 'NONE',  ( 58.50000000000001421, -88.00000000000000000, -20.00000000000000000 ) ) ;
#29897 = DIRECTION ( 'NONE',  ( -1.000000000000000000, 0.000000000000000000, 0.000000000000000000 ) ) ;
#29898 = ORIENTED_EDGE ( 'NONE', *, *, #14125, .T. ) ;
#29899 = CARTESIAN_POINT ( 'NONE',  ( -9.680171189290716072, 199.9079932115567146, 74.19886208192143329 ) ) ;
#29900 = CARTESIAN_POINT ( 'NONE',  ( -6.220909254589682469, 215.4770327129947134, 80.94886208192143329 ) ) ;
#29901 = CARTESIAN_POINT ( 'NONE',  ( 9.736236675708031640, 199.9851607334238963, 13.29886208192143826 ) ) ;
#29902 = CARTESIAN_POINT ( 'NONE',  ( -67.50001199999999812, 159.4078036646551482, -16.45628302766012752 ) ) ;
#29903 = CARTESIAN_POINT ( 'NONE',  ( -6.139770520408369237, 215.5359834540460042, 18.95113791807856884 ) ) ;
#29904 = CARTESIAN_POINT ( 'NONE',  ( -3.135527875058982783, 216.4958274776886924, 93.09886208192145318 ) ) ;
#29905 = ORIENTED_EDGE ( 'NONE', *, *, #14985, .F. ) ;
#29906 = LINE ( 'NONE', #24270, #24090 ) ;
#29907 = ORIENTED_EDGE ( 'NONE', *, *, #26337, .F. ) ;
#29908 = DIRECTION ( 'NONE',  ( 1.000000000000000000, -4.625929269271484928E-16, 0.000000000000000000 ) ) ;
#29909 = CARTESIAN_POINT ( 'NONE',  ( 2.426778023690075337, 214.6231898156240447, 69.39886208192143613 ) ) ;
#29910 = EDGE_CURVE ( 'NONE', #25081, #4510, #4875, .T. ) ;
#29911 = ORIENTED_EDGE ( 'NONE', *, *, #14742, .F. ) ;
#29912 = CARTESIAN_POINT ( 'NONE',  ( 85.62499999726880162, 171.3844434931184253, -7.942151717890134290E-15 ) ) ;
#29913 = ORIENTED_EDGE ( 'NONE', *, *, #21677, .F. ) ;
#29914 = CARTESIAN_POINT ( 'NONE',  ( 92.60208470531341618, 155.0000000000000000, 31.00000000000000000 ) ) ;
#29915 = AXIS2_PLACEMENT_3D ( 'NONE', #22128, #9521, #17187 ) ;
#29916 = CARTESIAN_POINT ( 'NONE',  ( 77.62499999726880162, 171.3844434931184253, -7.942151717890132712E-15 ) ) ;
#29917 = CARTESIAN_POINT ( 'NONE',  ( 54.78867513459483263, 155.0000000000000000, -15.00000000000002487 ) ) ;
#29918 = CARTESIAN_POINT ( 'NONE',  ( -2.517493886308901807, 199.4062855549015012, 71.90113791807856103 ) ) ;
#29919 = CARTESIAN_POINT ( 'NONE',  ( 6.500000000000000000, -3.752776749732574135, -8.000000000000000000 ) ) ;
#29920 = ADVANCED_FACE ( 'NONE', ( #2495 ), #10822, .T. ) ;
#29921 = CARTESIAN_POINT ( 'NONE',  ( 37.50000000000000000, 155.0000000000000000, 14.49999999999999467 ) ) ;
#29922 = CARTESIAN_POINT ( 'NONE',  ( 4.984841277089891776, 200.2242689037093726, 49.44886208192144750 ) ) ;
#29923 = ADVANCED_FACE ( 'NONE', ( #20714 ), #15164, .T. ) ;
#29924 = CARTESIAN_POINT ( 'NONE',  ( 10.00000000000000711, 206.9523078486586201, 71.00113791807858377 ) ) ;
#29925 = EDGE_CURVE ( 'NONE', #17208, #16362, #11906, .T. ) ;
#29926 = LINE ( 'NONE', #24981, #29537 ) ;
#29927 = LINE ( 'NONE', #6580, #9354 ) ;
#29928 = CARTESIAN_POINT ( 'NONE',  ( 49.82499999726881157, 168.2552932293087906, 9.630534252274372875 ) ) ;
#29929 = CARTESIAN_POINT ( 'NONE',  ( 11.98450388067348271, 203.0532714938637753, 56.15113791807857524 ) ) ;
#29930 = DIRECTION ( 'NONE',  ( -0.8191520442889872466, 0.000000000000000000, -0.5735764363510525987 ) ) ;
#29931 = CARTESIAN_POINT ( 'NONE',  ( -9.680171189290831535, 214.0920067884431148, 0.8011379180785656029 ) ) ;
#29932 = CARTESIAN_POINT ( 'NONE',  ( -10.01549611932653860, 203.7984951890123000, 78.35113791807857808 ) ) ;
#29933 = CARTESIAN_POINT ( 'NONE',  ( 7.456977232089471386, 196.8216656703012006, 34.44886208192142618 ) ) ;
#29934 = CARTESIAN_POINT ( 'NONE',  ( -9.984503880673420539, 203.7031108863293980, 47.34886208192143187 ) ) ;
#29935 = CARTESIAN_POINT ( 'NONE',  ( 85.39999999453762314, 141.2096805137202580, 4.480746418436733158 ) ) ;
#29936 = CARTESIAN_POINT ( 'NONE',  ( -12.00000000000000711, 207.0476921513413515, 90.50113791807858377 ) ) ;
#29937 = CARTESIAN_POINT ( 'NONE',  ( 4.984841277089725686, 213.7757310962907411, 100.5511379180785809 ) ) ;
#29938 = EDGE_CURVE ( 'NONE', #3719, #18876, #9334, .T. ) ;
#29939 = CARTESIAN_POINT ( 'NONE',  ( -6.139770520408224463, 198.4640165459539389, 56.04886208192142050 ) ) ;
#29940 = ORIENTED_EDGE ( 'NONE', *, *, #22229, .F. ) ;
#29941 = CARTESIAN_POINT ( 'NONE',  ( 0.05014649552828288198, 194.3824533091408000, 61.74886208192143755 ) ) ;
#29942 = ORIENTED_EDGE ( 'NONE', *, *, #18720, .F. ) ;
#29943 = CARTESIAN_POINT ( 'NONE',  ( 69.27499999726880731, 149.9369285172503510, -15.58253175000000823 ) ) ;
#29944 = CARTESIAN_POINT ( 'NONE',  ( -4.903702542908436435, 200.1653181626580249, 38.04886208192144892 ) ) ;
#29945 = EDGE_CURVE ( 'NONE', #8526, #18434, #700, .T. ) ;
#29946 = ORIENTED_EDGE ( 'NONE', *, *, #8334, .F. ) ;
#29947 = CARTESIAN_POINT ( 'NONE',  ( 81.77499999726880731, 169.8198683612136222, -4.815267126137197984 ) ) ;
#29948 = CARTESIAN_POINT ( 'NONE',  ( -9.000000000000001776, 206.9999999999998863, 103.5000000000000426 ) ) ;
#29949 = CARTESIAN_POINT ( 'NONE',  ( -6.837824896291515131, -3.947820044545435447, -6.564402953523717166 ) ) ;
#29950 = CARTESIAN_POINT ( 'NONE',  ( -4.903702542908602524, 213.8346818373418898, 60.95113791807857240 ) ) ;
#29951 = CARTESIAN_POINT ( 'NONE',  ( -3.942127870247283283, 206.4478425060960376, -5.603442290337207865 ) ) ;
#29952 = CARTESIAN_POINT ( 'NONE',  ( 3.135527875058981895, 197.5041725223112792, 46.59886208192143187 ) ) ;
#29953 = CARTESIAN_POINT ( 'NONE',  ( 66.97499999726881015, 140.1801316387863778, -4.815267126137194431 ) ) ;
#29954 = ORIENTED_EDGE ( 'NONE', *, *, #20985, .T. ) ;
#29955 = CARTESIAN_POINT ( 'NONE',  ( 32.50000000000000000, 155.0000000000000000, -15.00000000000002487 ) ) ;
#29956 =( NAMED_UNIT ( * ) SI_UNIT ( $, .STERADIAN. ) SOLID_ANGLE_UNIT ( ) );
#29957 = CARTESIAN_POINT ( 'NONE',  ( -125.0000000000000000, -25.00000000000000000, 35.00000000000000000 ) ) ;
#29958 = DIRECTION ( 'NONE',  ( 1.000000000000000000, 0.000000000000000000, 0.000000000000000000 ) ) ;
#29959 = CARTESIAN_POINT ( 'NONE',  ( 8.000000000000008882, 207.0476921513415220, 18.99886208192143400 ) ) ;
#29960 = CARTESIAN_POINT ( 'NONE',  ( -6.139770520408369237, 215.5359834540460042, 63.95113791807857950 ) ) ;
#29961 = CARTESIAN_POINT ( 'NONE',  ( -6.139770520408369237, 215.5359834540460042, 48.95113791807855108 ) ) ;
#29962 = CARTESIAN_POINT ( 'NONE',  ( 70.71132485994280614, 155.0000000000000000, 15.00000000000001243 ) ) ;
#29963 = CARTESIAN_POINT ( 'NONE',  ( 3.135527875058820690, 216.4958274776887492, 22.40113791807856458 ) ) ;
#29964 = CARTESIAN_POINT ( 'NONE',  ( 8.015496119326595448, 204.4483345814782638, 103.1488620819214361 ) ) ;
#29965 = CARTESIAN_POINT ( 'NONE',  ( 45.32499999726881157, 164.1591823560292198, -12.60653300113719766 ) ) ;
#29966 = DIRECTION ( 'NONE',  ( 0.000000000000000000, 0.000000000000000000, 1.000000000000000000 ) ) ;
#29967 = CARTESIAN_POINT ( 'NONE',  ( 87.49999999999998579, 159.6603719825695862, -14.83369040333126954 ) ) ;
#29968 = CARTESIAN_POINT ( 'NONE',  ( -7.456977232089304408, 196.8216656703010301, 24.05113791807857027 ) ) ;
#29969 = CARTESIAN_POINT ( 'NONE',  ( -63.50000000000004263, 215.0000000000000000, 2.500000000000000000 ) ) ;
#29970 = EDGE_CURVE ( 'NONE', #7334, #25250, #26649, .T. ) ;
#29971 = CARTESIAN_POINT ( 'NONE',  ( 10.00000000000000711, 206.9523078486586201, 77.00113791807858377 ) ) ;
#29972 = CARTESIAN_POINT ( 'NONE',  ( -8.118202686958039038, 201.1607312380087080, 36.20113791807857240 ) ) ;
#29973 = CARTESIAN_POINT ( 'NONE',  ( 76.48867513459482836, 142.2402378747194405, -9.270509831248439525 ) ) ;
#29974 = CARTESIAN_POINT ( 'NONE',  ( -3.499999999999997780, -2.020725942163714262, -2.587392608830344720 ) ) ;
#29975 = CARTESIAN_POINT ( 'NONE',  ( -9.736236675708031640, 214.0148392665760753, 8.798862081921434708 ) ) ;
#29976 = CARTESIAN_POINT ( 'NONE',  ( -9.984503880673420539, 203.7031108863293980, 23.34886208192143187 ) ) ;
#29977 = VECTOR ( 'NONE', #23471, 1000.000000000000000 ) ;
#29978 = CARTESIAN_POINT ( 'NONE',  ( 63.79999999453762882, 146.4771138417591203, -11.73074641843674470 ) ) ;
#29979 = ORIENTED_EDGE ( 'NONE', *, *, #24757, .F. ) ;
#29980 = CARTESIAN_POINT ( 'NONE',  ( -9.680171189290831535, 214.0920067884431148, 45.80113791807856671 ) ) ;
#29981 = CARTESIAN_POINT ( 'NONE',  ( 8.015496119326531499, 209.5516654185219636, 73.85113791807857808 ) ) ;
#29982 = EDGE_CURVE ( 'NONE', #1081, #18384, #5703, .T. ) ;
#29983 = CARTESIAN_POINT ( 'NONE',  ( 6.139770520408223575, 215.5359834540460611, 27.54886208192142760 ) ) ;
#29984 = CARTESIAN_POINT ( 'NONE',  ( 76.31132485994280046, 169.2658477444273331, 4.635254915624208216 ) ) ;
#29985 = ORIENTED_EDGE ( 'NONE', *, *, #18552, .T. ) ;
#29986 = CARTESIAN_POINT ( 'NONE',  ( -6.139770520408369237, 215.5359834540460042, 93.95113791807854398 ) ) ;
#29987 = EDGE_CURVE ( 'NONE', #20097, #29320, #16253, .T. ) ;
#29988 = ORIENTED_EDGE ( 'NONE', *, *, #6328, .T. ) ;
#29989 = CARTESIAN_POINT ( 'NONE',  ( 32.50000000000000000, 155.0000000000000000, -6.938893903907228378E-15 ) ) ;
#29990 = CARTESIAN_POINT ( 'NONE',  ( -54.79999999999999716, -6.711064459327494323E-15, 270.4495957273638282 ) ) ;
#29991 = ORIENTED_EDGE ( 'NONE', *, *, #28028, .T. ) ;
#29992 = CARTESIAN_POINT ( 'NONE',  ( 8.000000000000008882, 206.9523078486586485, 23.00113791807856600 ) ) ;
#29993 = CARTESIAN_POINT ( 'NONE',  ( 85.31132485994280046, 140.7341522555726669, -4.635254915624220651 ) ) ;
#29994 = CARTESIAN_POINT ( 'NONE',  ( -3.044812012439970683, 197.4746971517856196, 4.898862081921434353 ) ) ;
#29995 = CARTESIAN_POINT ( 'NONE',  ( 53.27499999726881441, 149.9369285172503510, -15.58253175000000823 ) ) ;
#29996 = EDGE_LOOP ( 'NONE', ( #27618, #27941, #26136, #17378 ) ) ;
#29997 = CARTESIAN_POINT ( 'NONE',  ( 8.000000000000008882, 206.9523078486586485, 50.00113791807856956 ) ) ;
#29998 = CARTESIAN_POINT ( 'NONE',  ( 2.000000000000000000, 1.329782007511006725, 0.7677499999999987113 ) ) ;
#29999 = CARTESIAN_POINT ( 'NONE',  ( 57.21132485994281325, 139.2280666364260071, -4.041636747397287284E-15 ) ) ;
#30000 = CARTESIAN_POINT ( 'NONE',  ( 9.984503880673420539, 210.2968891136705167, 87.84886208192141055 ) ) ;
#30001 = CARTESIAN_POINT ( 'NONE',  ( 62.47499999726881725, 149.9369285172503510, 15.58253174999999580 ) ) ;
#30002 = CARTESIAN_POINT ( 'NONE',  ( 0.05014649552810505201, 217.5146222423826714, 31.25113791807857311 ) ) ;
#30003 = CARTESIAN_POINT ( 'NONE',  ( -27.50000000000000000, 0.000000000000000000, -18.00000000000000000 ) ) ;
#30004 = CARTESIAN_POINT ( 'NONE',  ( 10.01549611932653860, 210.2015048109876716, 16.85113791807856032 ) ) ;
#30005 = DIRECTION ( 'NONE',  ( 1.000000000000000000, 0.000000000000000000, 0.000000000000000000 ) ) ;
#30006 = CARTESIAN_POINT ( 'NONE',  ( 78.20000000000001705, 142.6655632788954620, -8.961492836873480528 ) ) ;
#30007 = DIRECTION ( 'NONE',  ( 1.000000000000000000, 2.312964634635740985E-16, -0.000000000000000000 ) ) ;
#30008 = CARTESIAN_POINT ( 'NONE',  ( -6.220909254589537696, 198.5229672870051161, 90.05113791807858092 ) ) ;
#30009 = DIRECTION ( 'NONE',  ( -0.8660254037844382635, -0.5000000000000006661, 0.000000000000000000 ) ) ;
#30010 = CARTESIAN_POINT ( 'NONE',  ( 43.07499999726881157, 141.7447067706911810, -9.630534252274385310 ) ) ;
#30011 = CARTESIAN_POINT ( 'NONE',  ( 8.062137200540920645, 201.0835637161417822, 35.30113791807857382 ) ) ;
#30012 = EDGE_CURVE ( 'NONE', #22486, #19088, #4834, .T. ) ;
#30013 = CARTESIAN_POINT ( 'NONE',  ( 82.82499999726881867, 141.7447067706911810, -9.630534252274385310 ) ) ;
#30014 = CARTESIAN_POINT ( 'NONE',  ( 90.49452189536829394, 155.0000000000000000, 32.10452846326766974 ) ) ;
#30015 = DIRECTION ( 'NONE',  ( 0.000000000000000000, -0.5000000000000008882, -0.8660254037844381525 ) ) ;
#30016 = CARTESIAN_POINT ( 'NONE',  ( 47.29999999453762172, 142.6655632788954620, 8.961492836873471646 ) ) ;
#30017 = VERTEX_POINT ( 'NONE', #19451 ) ;
#30018 = CARTESIAN_POINT ( 'NONE',  ( -3.662846001190052991, 218.4274158808045740, 19.10113791807856742 ) ) ;
#30019 = ADVANCED_FACE ( 'NONE', ( #13697 ), #23935, .T. ) ;
#30020 = CARTESIAN_POINT ( 'NONE',  ( 2.466666666666999408, 0.000000000000000000, 3.099999999999998757 ) ) ;
#30021 = CARTESIAN_POINT ( 'NONE',  ( 109.0104235265664272, 155.0000000000000000, 11.99999999999998224 ) ) ;
#30022 = EDGE_LOOP ( 'NONE', ( #6943, #32488, #22140, #15901, #27211 ) ) ;
#30023 = AXIS2_PLACEMENT_3D ( 'NONE', #1717, #24733, #33239 ) ;
#30024 = CARTESIAN_POINT ( 'NONE',  ( -9.680171189290716072, 199.9079932115567146, 38.19886208192142618 ) ) ;
#30025 = CARTESIAN_POINT ( 'NONE',  ( 99.30625411593993590, 155.0000000000000000, 0.000000000000000000 ) ) ;
#30026 = CARTESIAN_POINT ( 'NONE',  ( -10.01549611932653860, 203.7984951890123284, 60.35113791807857808 ) ) ;
#30027 = CARTESIAN_POINT ( 'NONE',  ( -8.000000000000008882, 206.9523078486584780, 14.49886208192143577 ) ) ;
#30028 = CARTESIAN_POINT ( 'NONE',  ( 1.500000000000001332, 0.000000000000000000, 0.000000000000000000 ) ) ;
#30029 = EDGE_LOOP ( 'NONE', ( #6389, #11963, #17159, #28647, #17328 ) ) ;
#30030 = CARTESIAN_POINT ( 'NONE',  ( -4.984841277089891776, 213.7757310962905990, 98.94886208192143329 ) ) ;
#30031 = DIRECTION ( 'NONE',  ( 1.000000000000000000, -0.000000000000000000, -0.000000000000000000 ) ) ;
#30032 = CARTESIAN_POINT ( 'NONE',  ( 4.903702542908601636, 200.1653181626581102, 38.45113791807856529 ) ) ;
#30033 = CARTESIAN_POINT ( 'NONE',  ( 34.17499999726881299, 164.1591823560292198, 12.60653300113718167 ) ) ;
#30034 = ORIENTED_EDGE ( 'NONE', *, *, #26651, .T. ) ;
#30035 = CARTESIAN_POINT ( 'NONE',  ( 35.82499999726880446, 168.2552932293087906, 9.630534252274372875 ) ) ;
#30036 = DIRECTION ( 'NONE',  ( 0.000000000000000000, -1.000000000000000000, 0.000000000000000000 ) ) ;
#30037 = CARTESIAN_POINT ( 'NONE',  ( -8.062137200540920645, 212.9164362838581894, 0.8011379180785658249 ) ) ;
#30038 = SHAPE_REPRESENTATION ( 'pad arm right_right', ( #2404 ), #31228 ) ;
#30039 = CARTESIAN_POINT ( 'NONE',  ( 3.044812012439969795, 216.5253028482143520, 66.39886208192143613 ) ) ;
#30040 = CARTESIAN_POINT ( 'NONE',  ( 38.67499999726879878, 141.7447067706911810, 9.630534252274376428 ) ) ;
#30041 = DIRECTION ( 'NONE',  ( 0.000000000000000000, 0.000000000000000000, 1.000000000000000000 ) ) ;
#30042 = CARTESIAN_POINT ( 'NONE',  ( 6.139770520408368348, 198.4640165459539674, 5.451137918078567068 ) ) ;
#30043 = CARTESIAN_POINT ( 'NONE',  ( 62.60000000000000142, 159.7113355953771077, -14.50000000000000888 ) ) ;
#30044 = DIRECTION ( 'NONE',  ( 0.000000000000000000, 0.000000000000000000, 1.000000000000000000 ) ) ;
#30045 = CARTESIAN_POINT ( 'NONE',  ( 2.517493886309087436, 199.4062855549015865, 85.59886208192143897 ) ) ;
#30046 = CARTESIAN_POINT ( 'NONE',  ( 0.2779000157839532359, 8.820699686765054892, -7.928862157988302961 ) ) ;
#30047 = CARTESIAN_POINT ( 'NONE',  ( 32.50000000000000000, 155.0000000000000000, 15.00000000000001243 ) ) ;
#30048 = CARTESIAN_POINT ( 'NONE',  ( 65.62499999726880162, 171.3844434931184253, -7.942151717890132712E-15 ) ) ;
#30050 = ORIENTED_EDGE ( 'NONE', *, *, #24542, .F. ) ;
#30049 = CARTESIAN_POINT ( 'NONE',  ( -8.062137200540920645, 212.9164362838581894, 24.80113791807857027 ) ) ;
#30051 = CARTESIAN_POINT ( 'NONE',  ( -64.50000000000000000, 0.000000000000000000, 20.00000000000000000 ) ) ;
#30052 = CONICAL_SURFACE ( 'NONE', #21339, 7.500000000000001776, 0.8594454914424796144 ) ;
#30053 = CARTESIAN_POINT ( 'NONE',  ( 80.47499999726881015, 149.9369285172503510, 15.58253174999999580 ) ) ;
#30054 = CARTESIAN_POINT ( 'NONE',  ( -3.753561863808691168, 195.6020594897209435, 89.90113791807857524 ) ) ;
#30055 = VECTOR ( 'NONE', #20390, 1000.000000000000000 ) ;
#30056 = CYLINDRICAL_SURFACE ( 'NONE', #16470, 2.149999999999984812 ) ;
#30057 = ADVANCED_FACE ( 'NONE', ( #21372 ), #4292, .F. ) ;
#30058 = ORIENTED_EDGE ( 'NONE', *, *, #13922, .T. ) ;
#30059 = CARTESIAN_POINT ( 'NONE',  ( -12.01549611932659722, 210.8513442034533227, 71.64886208192143613 ) ) ;
#30060 = CARTESIAN_POINT ( 'NONE',  ( -0.05014649552828402690, 217.5146222423826714, 75.24886208192144466 ) ) ;
#30061 = CARTESIAN_POINT ( 'NONE',  ( 12.01549611932659367, 203.1486557965466773, 16.14886208192143613 ) ) ;
#30062 = LINE ( 'NONE', #1953, #15372 ) ;
#30063 = CARTESIAN_POINT ( 'NONE',  ( 3.135527875058820690, 216.4958274776887492, 28.40113791807856813 ) ) ;
#30064 = CARTESIAN_POINT ( 'NONE',  ( 9.379977934355910207, 208.8253170565643870, -1.014254689207407356 ) ) ;
#30065 = CARTESIAN_POINT ( 'NONE',  ( -9.984503880673420539, 203.7031108863293980, 86.34886208192143897 ) ) ;
#30066 = AXIS2_PLACEMENT_3D ( 'NONE', #30343, #17392, #27777 ) ;
#30067 = CARTESIAN_POINT ( 'NONE',  ( 39.51132485994280330, 146.1832212156128890, -12.13525491562423042 ) ) ;
#30068 = ORIENTED_EDGE ( 'NONE', *, *, #18266, .T. ) ;
#30069 = DIRECTION ( 'NONE',  ( -0.1461455375466716444, 0.9854922318508084755, -0.08629335326029916042 ) ) ;
#30070 = CARTESIAN_POINT ( 'NONE',  ( -7.984503880673422316, 204.3529502787951628, 71.34886208192142476 ) ) ;
#30071 = ORIENTED_EDGE ( 'NONE', *, *, #26240, .T. ) ;
#30072 = CARTESIAN_POINT ( 'NONE',  ( 87.12499999726880162, 155.0000000000000000, -15.58253175000000823 ) ) ;
#30073 = VERTEX_POINT ( 'NONE', #18820 ) ;
#30074 = CARTESIAN_POINT ( 'NONE',  ( 32.50000000000000000, 155.0000000000000000, -15.00000000000002487 ) ) ;
#30075 = CIRCLE ( 'NONE', #7226, 32.00000000000005684 ) ;
#30076 = CONICAL_SURFACE ( 'NONE', #9979, 10.39117206796836079, 1.221730476396047926 ) ;
#30077 = CARTESIAN_POINT ( 'NONE',  ( 77.02499999726880731, 149.9369285172503510, -15.58253175000000823 ) ) ;
#30078 = DIRECTION ( 'NONE',  ( -1.000000000000000000, 0.000000000000000000, 0.000000000000000000 ) ) ;
#30079 = CARTESIAN_POINT ( 'NONE',  ( -2.517493886308901807, 199.4062855549015012, 80.90113791807858945 ) ) ;
#30080 = CARTESIAN_POINT ( 'NONE',  ( 87.50000000000004263, 170.1307320771869627, -3.377640367381898212 ) ) ;
#30081 = CARTESIAN_POINT ( 'NONE',  ( 44.60000000000000142, 159.7113355953771077, -14.50000000000000888 ) ) ;
#30082 = CARTESIAN_POINT ( 'NONE',  ( -2.517493886309087880, 214.5937144450984135, 54.09886208192143897 ) ) ;
#30083 = CIRCLE ( 'NONE', #14306, 1.535500000000000087 ) ;
#30084 = CARTESIAN_POINT ( 'NONE',  ( 77.50000000000000000, 155.0000000000000000, -6.938893903907228378E-15 ) ) ;
#30085 = DIRECTION ( 'NONE',  ( 1.000000000000000000, 0.000000000000000000, 0.000000000000000000 ) ) ;
#30086 = DIRECTION ( 'NONE',  ( 1.000000000000000000, 0.000000000000000000, 0.000000000000000000 ) ) ;
#30087 = CARTESIAN_POINT ( 'NONE',  ( 48.92499999726881299, 145.8408176439707802, -12.60653300113719588 ) ) ;
#30088 = CARTESIAN_POINT ( 'NONE',  ( 62.77499999726882152, 140.1801316387863778, 4.815267126137185549 ) ) ;
#30089 = CARTESIAN_POINT ( 'NONE',  ( 12.00000000000000711, 206.9523078486586485, 56.00113791807856956 ) ) ;
#30090 = DIRECTION ( 'NONE',  ( 1.000000000000000000, 0.000000000000000000, 0.000000000000000000 ) ) ;
#30091 = PRODUCT ( 'socket head cap screw_iso_ISO 4762 M8 x 70 - 28N', 'socket head cap screw_iso_ISO 4762 M8 x 70 - 28N', '', ( #7686 ) ) ;
#30092 = CARTESIAN_POINT ( 'NONE',  ( 0.05014649552807549926, 219.6175466908591716, 4.251137918078565114 ) ) ;
#30093 = CARTESIAN_POINT ( 'NONE',  ( 3.135527875058820690, 216.4958274776887492, 79.40113791807857524 ) ) ;
#30094 = CARTESIAN_POINT ( 'NONE',  ( -3.753561863808878130, 218.3979405102790281, 42.09886208192143897 ) ) ;
#30095 = CARTESIAN_POINT ( 'NONE',  ( -6.139770520408224463, 198.4640165459539105, 50.04886208192143471 ) ) ;
#30096 = CARTESIAN_POINT ( 'NONE',  ( 88.09999999453761177, 159.7113355953771077, -14.50000000000000888 ) ) ;
#30097 = VECTOR ( 'NONE', #3597, 1000.000000000000000 ) ;
#30098 = CARTESIAN_POINT ( 'NONE',  ( -3.662846001190052991, 218.4274158808045740, 91.10113791807859229 ) ) ;
#30099 = CARTESIAN_POINT ( 'NONE',  ( -6.500168698208129925, 202.3363017425936050, 102.2011379180785866 ) ) ;
#30100 = AXIS2_PLACEMENT_3D ( 'NONE', #19807, #24917, #22697 ) ;
#30101 = CARTESIAN_POINT ( 'NONE',  ( -6.220909254589682469, 215.4770327129946850, 56.94886208192141908 ) ) ;
#30102 = EDGE_CURVE ( 'NONE', #13858, #22150, #25498, .T. ) ;
#30103 = AXIS2_PLACEMENT_3D ( 'NONE', #11016, #32408, #10857 ) ;
#30104 = DIRECTION ( 'NONE',  ( 0.000000000000000000, -0.5000000000000014433, -0.8660254037844379305 ) ) ;
#30105 = VERTEX_POINT ( 'NONE', #29214 ) ;
#30106 = CARTESIAN_POINT ( 'NONE',  ( 12.00000000000000711, 207.0476921513415220, 69.99886208192144466 ) ) ;
#30107 = EDGE_LOOP ( 'NONE', ( #13982, #1961, #25586, #20436, #12304 ) ) ;
#30108 = CARTESIAN_POINT ( 'NONE',  ( 71.57499999726881867, 164.1591823560292198, -12.60653300113719766 ) ) ;
#30109 = CARTESIAN_POINT ( 'NONE',  ( -4.903702542908436435, 200.1653181626580249, 41.04886208192144181 ) ) ;
#30110 = ORIENTED_EDGE ( 'NONE', *, *, #22049, .F. ) ;
#30111 = CARTESIAN_POINT ( 'NONE',  ( 82.57499999726880446, 145.8408176439707802, 12.60653300113718345 ) ) ;
#30112 = PLANE ( 'NONE',  #26035 ) ;
#30113 = EDGE_CURVE ( 'NONE', #22576, #9805, #5909, .T. ) ;
#30114 = VECTOR ( 'NONE', #12923, 1000.000000000000114 ) ;
#30115 = DIRECTION ( 'NONE',  ( 0.000000000000000000, 0.000000000000000000, -1.000000000000000000 ) ) ;
#30116 = CARTESIAN_POINT ( 'NONE',  ( 7.984503880673485376, 204.3529502787953902, 62.15113791807858945 ) ) ;
#30117 = CARTESIAN_POINT ( 'NONE',  ( 60.63708498984762940, 155.0000000000000000, 40.00000000000001421 ) ) ;
#30118 = CARTESIAN_POINT ( 'NONE',  ( -6.139770520408224463, 198.4640165459539389, 41.04886208192142760 ) ) ;
#30119 = EDGE_LOOP ( 'NONE', ( #7793, #8110, #4552 ) ) ;
#30120 = FACE_OUTER_BOUND ( 'NONE', #28649, .T. ) ;
#30121 = VECTOR ( 'NONE', #13995, 999.9999999999998863 ) ;
#30122 = FILL_AREA_STYLE ('',( #11557 ) ) ;
#30123 = DIRECTION ( 'NONE',  ( 1.000000000000000000, 0.000000000000000000, 0.000000000000000000 ) ) ;
#30124 = CARTESIAN_POINT ( 'NONE',  ( 85.71132485994282035, 155.0000000000000000, -15.00000000000002487 ) ) ;
#30125 = CARTESIAN_POINT ( 'NONE',  ( -4.903702542908436435, 200.1653181626580249, 23.04886208192143826 ) ) ;
#30126 = VECTOR ( 'NONE', #15322, 1000.000000000000000 ) ;
#30127 = CARTESIAN_POINT ( 'NONE',  ( 8.118202686958039038, 212.8392687619912635, 64.70113791807857240 ) ) ;
#30128 = CARTESIAN_POINT ( 'NONE',  ( -9.984503880673473830, 210.2968891136704315, 45.65113791807855392 ) ) ;
#30129 = CARTESIAN_POINT ( 'NONE',  ( 67.38867513459481984, 169.2658477444273331, 4.635254915624208216 ) ) ;
#30130 = CONICAL_SURFACE ( 'NONE', #19233, 32.10452846326769816, 1.466076571675243079 ) ;
#30131 = CARTESIAN_POINT ( 'NONE',  ( 0.05014649552810505201, 217.5146222423826714, 19.25113791807856600 ) ) ;
#30132 = CARTESIAN_POINT ( 'NONE',  ( 4.984841277089725686, 213.7757310962907411, 7.551137918078564049 ) ) ;
#30133 = CARTESIAN_POINT ( 'NONE',  ( 46.62499999726880873, 138.6155565068815463, -3.929120461958505118E-15 ) ) ;
#30134 = PRESENTATION_STYLE_ASSIGNMENT (( #22121 ) ) ;
#30135 = CARTESIAN_POINT ( 'NONE',  ( 87.49999999999995737, 158.6695690980871518, -15.06022462549181817 ) ) ;
#30136 = CARTESIAN_POINT ( 'NONE',  ( 12.00000000000000711, 206.9523078486586485, 26.00113791807856600 ) ) ;
#30137 = CARTESIAN_POINT ( 'NONE',  ( 77.50000000000000000, 155.0000000000000000, -6.938893903907228378E-15 ) ) ;
#30138 = EDGE_CURVE ( 'NONE', #29320, #15495, #1226, .T. ) ;
#30139 = CARTESIAN_POINT ( 'NONE',  ( -6.220909254589537696, 198.5229672870051161, 75.05113791807858092 ) ) ;
#30140 = CARTESIAN_POINT ( 'NONE',  ( 10.00000000000000711, 206.9523078486586201, 53.00113791807857666 ) ) ;
#30141 = DIRECTION ( 'NONE',  ( 0.000000000000000000, 0.000000000000000000, -1.000000000000000000 ) ) ;
#30142 = CIRCLE ( 'NONE', #5654, 1.535500000000000087 ) ;
#30143 = CARTESIAN_POINT ( 'NONE',  ( -2.047034997319599814, -2.859595677584359841, -2.899999999999983036 ) ) ;
#30144 = CARTESIAN_POINT ( 'NONE',  ( -7.456977232089471386, 217.1783343296987709, 17.94886208192143684 ) ) ;
#30145 = CARTESIAN_POINT ( 'NONE',  ( 10.00000000000000711, 207.0476921513415220, 15.99886208192143400 ) ) ;
#30146 = CARTESIAN_POINT ( 'NONE',  ( 67.29999999453761461, 142.6655632788954620, 8.961492836873471646 ) ) ;
#30147 = EDGE_LOOP ( 'NONE', ( #20773, #9702, #21376, #23495, #9919 ) ) ;
#30148 = CARTESIAN_POINT ( 'NONE',  ( 3.753561863808689836, 218.3979405102790565, 58.40113791807858235 ) ) ;
#30149 = CARTESIAN_POINT ( 'NONE',  ( 6.500168698208129925, 211.6636982574063381, 67.70113791807857240 ) ) ;
#30150 = CARTESIAN_POINT ( 'NONE',  ( -10.01549611932659722, 210.2015048109875011, 35.64886208192143613 ) ) ;
#30151 = ADVANCED_FACE ( 'NONE', ( #28882 ), #2991, .F. ) ;
#30152 = CARTESIAN_POINT ( 'NONE',  ( 75.71132485994280614, 155.0000000000000000, -15.00000000000002487 ) ) ;
#30153 = VERTEX_POINT ( 'NONE', #5538 ) ;
#30154 = CARTESIAN_POINT ( 'NONE',  ( -3.135527875058821579, 197.5041725223112223, 86.90113791807857524 ) ) ;
#30155 = AXIS2_PLACEMENT_3D ( 'NONE', #21766, #8816, #23825 ) ;
#30156 = ORIENTED_EDGE ( 'NONE', *, *, #16367, .T. ) ;
#30157 = DIRECTION ( 'NONE',  ( 1.000000000000000000, 0.000000000000000000, 0.000000000000000000 ) ) ;
#30158 = ADVANCED_FACE ( 'NONE', ( #13371 ), #15188, .T. ) ;
#30159 = CARTESIAN_POINT ( 'NONE',  ( 2.000000000000000000, 0.8865213383406723713, 1.535499999999998755 ) ) ;
#30160 = EDGE_LOOP ( 'NONE', ( #7193, #32786, #2771, #8558, #6079 ) ) ;
#30161 = CARTESIAN_POINT ( 'NONE',  ( -7.984503880673488041, 209.6470497212046098, 30.65113791807856458 ) ) ;
#30162 = CARTESIAN_POINT ( 'NONE',  ( 84.91132485994279477, 146.1832212156128890, 12.13525491562421976 ) ) ;
#30163 = CARTESIAN_POINT ( 'NONE',  ( 0.05014649552828275708, 196.4853777576173002, 16.74886208192143755 ) ) ;
#30164 = CARTESIAN_POINT ( 'NONE',  ( 54.47499999726880304, 149.9369285172503510, 15.58253174999999580 ) ) ;
#30165 = ORIENTED_EDGE ( 'NONE', *, *, #33090, .F. ) ;
#30166 = CARTESIAN_POINT ( 'NONE',  ( -2.517493886308901807, 199.4062855549015012, 53.90113791807858235 ) ) ;
#30167 = CARTESIAN_POINT ( 'NONE',  ( 67.51132485994278909, 146.1832212156128890, -12.13525491562423042 ) ) ;
#30168 =( NAMED_UNIT ( * ) SI_UNIT ( $, .STERADIAN. ) SOLID_ANGLE_UNIT ( ) );
#30169 = CARTESIAN_POINT ( 'NONE',  ( 57.31132485994280756, 140.7341522555726669, -4.635254915624220651 ) ) ;
#30170 = CARTESIAN_POINT ( 'NONE',  ( -9.984503880673420539, 203.7031108863293980, 101.3488620819213963 ) ) ;
#30171 = CARTESIAN_POINT ( 'NONE',  ( 59.87499999726882294, 171.3844434931184253, -7.942151717890132712E-15 ) ) ;
#30172 = CARTESIAN_POINT ( 'NONE',  ( -3.044812012440131443, 216.5253028482142952, 28.10113791807857098 ) ) ;
#30173 = CARTESIAN_POINT ( 'NONE',  ( 70.38867513459481984, 140.7341522555726669, -4.635254915624220651 ) ) ;
#30174 = ADVANCED_FACE ( 'NONE', ( #25070 ), #25579, .T. ) ;
#30175 = CARTESIAN_POINT ( 'NONE',  ( -8.062137200540920645, 212.9164362838581894, 18.80113791807856671 ) ) ;
#30176 = DIRECTION ( 'NONE',  ( 1.000000000000000000, 0.000000000000000000, 6.123233995736766036E-17 ) ) ;
#30177 = CARTESIAN_POINT ( 'NONE',  ( 78.60000000000000853, 159.7113355953771077, -14.50000000000000888 ) ) ;
#30178 = DIRECTION ( 'NONE',  ( 1.000000000000000000, 0.000000000000000000, 0.000000000000000000 ) ) ;
#30179 = DIRECTION ( 'NONE',  ( 1.000000000000000000, 0.000000000000000000, 0.000000000000000000 ) ) ;
#30180 = CARTESIAN_POINT ( 'NONE',  ( -3.662846001190052991, 218.4274158808045740, 1.101137918078565647 ) ) ;
#30181 = CARTESIAN_POINT ( 'NONE',  ( -125.0000000000000000, 0.000000000000000000, -35.00000000000000000 ) ) ;
#30182 = CARTESIAN_POINT ( 'NONE',  ( 44.27499999726881441, 160.0630714827496206, 15.58253174999999402 ) ) ;
#30183 = ADVANCED_FACE ( 'NONE', ( #1904, #4111 ), #9397, .T. ) ;
#30184 = CARTESIAN_POINT ( 'NONE',  ( 8.062137200540920645, 201.0835637161417822, 44.30113791807857382 ) ) ;
#30185 = CARTESIAN_POINT ( 'NONE',  ( 86.52499999726882152, 140.1801316387863778, 4.815267126137185549 ) ) ;
#30186 = CARTESIAN_POINT ( 'NONE',  ( -65.24999999999998579, -6.704941225331758828E-15, -35.00000000000000000 ) ) ;
#30187 = DIRECTION ( 'NONE',  ( -1.000000000000000000, -0.000000000000000000, -0.000000000000000000 ) ) ;
#30188 = CARTESIAN_POINT ( 'NONE',  ( 49.59999999453763309, 141.2096805137202580, -4.480746418436742040 ) ) ;
#30189 = ORIENTED_EDGE ( 'NONE', *, *, #6828, .T. ) ;
#30190 = CARTESIAN_POINT ( 'NONE',  ( 9.680171189290831535, 199.9079932115568852, 26.30113791807856316 ) ) ;
#30191 = CARTESIAN_POINT ( 'NONE',  ( 80.71132485994280614, 155.0000000000000000, 15.00000000000001243 ) ) ;
#30192 = LINE ( 'NONE', #14848, #28095 ) ;
#30193 = ORIENTED_EDGE ( 'NONE', *, *, #17926, .T. ) ;
#30194 = CARTESIAN_POINT ( 'NONE',  ( -11.98450388067341876, 203.0532714938636047, 44.34886208192143897 ) ) ;
#30195 = CARTESIAN_POINT ( 'NONE',  ( -6.220909254589537696, 198.5229672870051161, 3.051137918078564937 ) ) ;
#30196 = CARTESIAN_POINT ( 'NONE',  ( 0.05014649552810505201, 217.5146222423826714, 61.25113791807856245 ) ) ;
#30197 = CARTESIAN_POINT ( 'NONE',  ( -0.05014649552828365914, 215.4116977939061144, 27.24886208192143755 ) ) ;
#30198 = CARTESIAN_POINT ( 'NONE',  ( -67.50000000000000000, 0.000000000000000000, -17.00000000000001421 ) ) ;
#30199 = ORIENTED_EDGE ( 'NONE', *, *, #9062, .T. ) ;
#30200 = CARTESIAN_POINT ( 'NONE',  ( 8.000000000000008882, 206.9523078486586485, -0.9988620819214343305 ) ) ;
#30201 = EDGE_CURVE ( 'NONE', #4805, #21429, #26582, .T. ) ;
#30202 = ADVANCED_FACE ( 'NONE', ( #12124 ), #28133, .T. ) ;
#30203 = DIRECTION ( 'NONE',  ( 0.000000000000000000, 0.000000000000000000, 1.000000000000000000 ) ) ;
#30204 = CARTESIAN_POINT ( 'NONE',  ( 0.05014649552828288198, 194.3824533091408000, 88.74886208192143044 ) ) ;
#30205 = DIRECTION ( 'NONE',  ( -1.000000000000000000, 0.000000000000000000, 0.000000000000000000 ) ) ;
#30206 = ORIENTED_EDGE ( 'NONE', *, *, #1654, .T. ) ;
#30207 = CARTESIAN_POINT ( 'NONE',  ( 39.22499999726881015, 160.0630714827496206, -15.58253175000000823 ) ) ;
#30208 = DIRECTION ( 'NONE',  ( 1.000000000000000000, 0.000000000000000000, 0.000000000000000000 ) ) ;
#30209 = CARTESIAN_POINT ( 'NONE',  ( -4.411512144081271877E-13, -7.790635086499372086, -6.526184258131371152 ) ) ;
#30211 = ADVANCED_FACE ( 'NONE', ( #12463 ), #7024, .F. ) ;
#30210 = CARTESIAN_POINT ( 'NONE',  ( 6.139770520408223575, 215.5359834540460611, 57.54886208192142050 ) ) ;
#30212 = CARTESIAN_POINT ( 'NONE',  ( 39.47499999726881015, 160.0630714827496206, -15.58253175000000823 ) ) ;
#30213 = CARTESIAN_POINT ( 'NONE',  ( 5.000000000000000000, 4.685197434473814759, -5.637851296924623057E-15 ) ) ;
#30214 = CARTESIAN_POINT ( 'NONE',  ( 3.135527875058820690, 216.4958274776887492, 1.401137918078565914 ) ) ;
#30215 = DIRECTION ( 'NONE',  ( 1.000000000000000000, -0.000000000000000000, -0.000000000000000000 ) ) ;
#30216 = EDGE_CURVE ( 'NONE', #739, #22562, #6843, .T. ) ;
#30217 = CARTESIAN_POINT ( 'NONE',  ( 58.30000000000000426, 146.4771138417591203, -11.73074641843674470 ) ) ;
#30218 = CARTESIAN_POINT ( 'NONE',  ( 64.11132485994281183, 169.2658477444273331, -4.635254915624224203 ) ) ;
#30219 = CARTESIAN_POINT ( 'NONE',  ( 4.984841277089891776, 200.2242689037093726, 79.44886208192144750 ) ) ;
#30220 = DIRECTION ( 'NONE',  ( 1.000000000000000000, 0.000000000000000000, 0.000000000000000000 ) ) ;
#30221 = DIRECTION ( 'NONE',  ( 0.000000000000000000, 0.000000000000000000, 1.000000000000000000 ) ) ;
#30222 = ADVANCED_FACE ( 'NONE', ( #32728 ), #19793, .T. ) ;
#30223 = CARTESIAN_POINT ( 'NONE',  ( -7.375838497908014268, 196.7627149292498530, 83.04886208192144181 ) ) ;
#30224 = CARTESIAN_POINT ( 'NONE',  ( 67.22499999726879594, 160.0630714827496206, -15.58253175000000823 ) ) ;
#30226 = ORIENTED_EDGE ( 'NONE', *, *, #13733, .T. ) ;
#30225 = CARTESIAN_POINT ( 'NONE',  ( -8.118202686958039038, 201.1607312380087080, 18.20113791807856884 ) ) ;
#30227 = CARTESIAN_POINT ( 'NONE',  ( -10.00000000000000178, 206.0011379180784559, 103.4523078486585916 ) ) ;
#30228 = CARTESIAN_POINT ( 'NONE',  ( 80.37499999726881583, 155.0000000000000000, 15.58253174999999402 ) ) ;
#30229 = CARTESIAN_POINT ( 'NONE',  ( -3.662846001190052991, 218.4274158808045740, 82.10113791807857808 ) ) ;
#30230 = DIRECTION ( 'NONE',  ( -1.000000000000000000, 0.000000000000000000, 0.000000000000000000 ) ) ;
#30231 = ORIENTED_EDGE ( 'NONE', *, *, #22076, .F. ) ;
#30232 = CARTESIAN_POINT ( 'NONE',  ( -9.680171189290716072, 199.9079932115567146, 68.19886208192143329 ) ) ;
#30233 = CARTESIAN_POINT ( 'NONE',  ( 9.984503880673420539, 210.2968891136705736, 75.84886208192143897 ) ) ;
#30234 = CARTESIAN_POINT ( 'NONE',  ( -0.05014649552828442242, 219.6175466908591716, 18.24886208192143755 ) ) ;
#30235 = CARTESIAN_POINT ( 'NONE',  ( -3.500000000000001332, 2.020725942163676070, -0.3126073911696459207 ) ) ;
#30236 = CARTESIAN_POINT ( 'NONE',  ( 0.05014649552810505201, 217.5146222423826714, 31.25113791807857311 ) ) ;
#30237 = CARTESIAN_POINT ( 'NONE',  ( -0.2855619784720673793, 3.876582599186217948, -2.682579934988236658 ) ) ;
#30238 = CARTESIAN_POINT ( 'NONE',  ( 10.01549611932659545, 203.7984951890123853, 103.1488620819214077 ) ) ;
#30239 = CARTESIAN_POINT ( 'NONE',  ( -0.2259792476677698891, 7.636022678937394836, -6.470294263593361350 ) ) ;
#30240 = ORIENTED_EDGE ( 'NONE', *, *, #27240, .F. ) ;
#30241 = FACE_OUTER_BOUND ( 'NONE', #11512, .T. ) ;
#30242 = CARTESIAN_POINT ( 'NONE',  ( 2.517493886309087436, 199.4062855549015865, 67.59886208192143897 ) ) ;
#30243 = SHAPE_REPRESENTATION ( 'torque nut 01_iso_ISO 7040-M4-N', ( #2404 ), #19701 ) ;
#30244 = ORIENTED_EDGE ( 'NONE', *, *, #30492, .F. ) ;
#30245 = CARTESIAN_POINT ( 'NONE',  ( 83.82499999726880446, 168.2552932293087906, 9.630534252274372875 ) ) ;
#30246 = ORIENTED_EDGE ( 'NONE', *, *, #6390, .T. ) ;
#30247 = DIRECTION ( 'NONE',  ( -0.000000000000000000, -0.000000000000000000, 1.000000000000000000 ) ) ;
#30248 = CARTESIAN_POINT ( 'NONE',  ( 75.62499999726881583, 171.3844434931184253, -7.942151717890132712E-15 ) ) ;
#30249 = CARTESIAN_POINT ( 'NONE',  ( -52.50000000000002132, 155.0000000000000000, -16.99999999999999645 ) ) ;
#30250 = CARTESIAN_POINT ( 'NONE',  ( 4.903702542908601636, 200.1653181626581102, 77.45113791807855819 ) ) ;
#30251 = DIRECTION ( 'NONE',  ( -0.000000000000000000, -0.000000000000000000, 1.000000000000000000 ) ) ;
#30252 = CARTESIAN_POINT ( 'NONE',  ( 40.19999999999999574, 142.6655632788954620, -8.961492836873480528 ) ) ;
#30253 = CARTESIAN_POINT ( 'NONE',  ( -4.903702542908436435, 200.1653181626580249, 50.04886208192144181 ) ) ;
#30254 = CIRCLE ( 'NONE', #5311, 18.00000000000000355 ) ;
#30255 = CARTESIAN_POINT ( 'NONE',  ( 111.1125082318798007, 155.0000000000000000, -32.00000000000002842 ) ) ;
#30256 = CARTESIAN_POINT ( 'NONE',  ( -7.808218555861951238, 4.508077085120201666, -7.999534413642737540 ) ) ;
#30257 = LINE ( 'NONE', #25138, #2972 ) ;
#30258 = CARTESIAN_POINT ( 'NONE',  ( 48.12499999726880873, 155.0000000000000000, 15.58253174999999402 ) ) ;
#30259 = CARTESIAN_POINT ( 'NONE',  ( 61.57499999726881157, 164.1591823560292198, -12.60653300113719766 ) ) ;
#30260 = CARTESIAN_POINT ( 'NONE',  ( -12.00000000000000711, 207.0476921513413515, 54.50113791807857666 ) ) ;
#30261 = DIRECTION ( 'NONE',  ( 1.000000000000000000, 0.000000000000000000, 0.000000000000000000 ) ) ;
#30262 = CARTESIAN_POINT ( 'NONE',  ( -9.736236675707914401, 199.9851607334237542, 0.2011379180785655418 ) ) ;
#30263 = CARTESIAN_POINT ( 'NONE',  ( -8.062137200540920645, 212.9164362838581894, 81.80113791807858092 ) ) ;
#30264 = CARTESIAN_POINT ( 'NONE',  ( -3.753561863808878130, 218.3979405102790281, 45.09886208192143897 ) ) ;
#30265 = CARTESIAN_POINT ( 'NONE',  ( -8.062137200540822946, 201.0835637161416400, 50.19886208192144039 ) ) ;
#30266 = CARTESIAN_POINT ( 'NONE',  ( 0.000000000000000000, 0.000000000000000000, 0.000000000000000000 ) ) ;
#30267 = CARTESIAN_POINT ( 'NONE',  ( 7.456977232089302632, 217.1783343296989131, 91.55113791807858092 ) ) ;
#30268 = CYLINDRICAL_SURFACE ( 'NONE', #29521, 12.10452846326763598 ) ;
#30269 = CARTESIAN_POINT ( 'NONE',  ( 10.01549611932653860, 210.2015048109876716, 4.851137918078563871 ) ) ;
#30270 = CARTESIAN_POINT ( 'NONE',  ( 9.984503880673420539, 210.2968891136705167, 66.84886208192141055 ) ) ;
#30271 = DIRECTION ( 'NONE',  ( 0.000000000000000000, 0.000000000000000000, -1.000000000000000000 ) ) ;
#30272 = ORIENTED_EDGE ( 'NONE', *, *, #14945, .T. ) ;
#30273 = CARTESIAN_POINT ( 'NONE',  ( 3.753561863808876797, 195.6020594897209719, 67.59886208192143897 ) ) ;
#30274 = ORIENTED_EDGE ( 'NONE', *, *, #20214, .F. ) ;
#30275 = CARTESIAN_POINT ( 'NONE',  ( 71.87499999726881583, 171.3844434931184253, -7.942151717890132712E-15 ) ) ;
#30276 = CARTESIAN_POINT ( 'NONE',  ( -2.517493886309087880, 214.5937144450984135, 45.09886208192144608 ) ) ;
#30277 = VERTEX_POINT ( 'NONE', #17064 ) ;
#30278 = VECTOR ( 'NONE', #6517, 1000.000000000000000 ) ;
#30279 = CARTESIAN_POINT ( 'NONE',  ( 82.17499999726882720, 164.1591823560292198, 12.60653300113718167 ) ) ;
#30280 = DIRECTION ( 'NONE',  ( -1.000000000000000000, -0.000000000000000000, -0.000000000000000000 ) ) ;
#30281 = CLOSED_SHELL ( 'NONE', ( #12702, #25963, #32494, #10648, #17287, #16359, #24282, #1865, #18926, #27, #19107, #8818, #10026, #3907, #29923, #21011, #11005, #5970, #22288, #1196, #361, #11997, #10550, #13682, #2296, #23715, #23898, #29162 ) ) ;
#30282 = CARTESIAN_POINT ( 'NONE',  ( -1.127757440534757460, -7.231345287187099125, -6.344532336093708480 ) ) ;
#30283 = FACE_OUTER_BOUND ( 'NONE', #3407, .T. ) ;
#30284 = CARTESIAN_POINT ( 'NONE',  ( -10.01549611932659722, 210.2015048109875011, 44.64886208192143613 ) ) ;
#30285 = ORIENTED_EDGE ( 'NONE', *, *, #32029, .T. ) ;
#30286 = AXIS2_PLACEMENT_3D ( 'NONE', #16493, #11397, #32164 ) ;
#30287 = DIRECTION ( 'NONE',  ( 0.000000000000000000, 0.000000000000000000, 1.000000000000000000 ) ) ;
#30288 = FACE_OUTER_BOUND ( 'NONE', #409, .T. ) ;
#30289 = LINE ( 'NONE', #6955, #9870 ) ;
#30290 = CARTESIAN_POINT ( 'NONE',  ( 2.426778023690075337, 214.6231898156240447, 27.39886208192143613 ) ) ;
#30291 = CARTESIAN_POINT ( 'NONE',  ( 3.044812012440130555, 197.4746971517856764, 56.60113791807857098 ) ) ;
#30292 = ADVANCED_FACE ( 'NONE', ( #27616 ), #14676, .T. ) ;
#30293 = CARTESIAN_POINT ( 'NONE',  ( 8.062137200540920645, 201.0835637161417822, 47.30113791807857382 ) ) ;
#30294 = DIRECTION ( 'NONE',  ( -1.000000000000000000, 1.224646799147352714E-16, 0.000000000000000000 ) ) ;
#30295 = CONTEXT_DEPENDENT_SHAPE_REPRESENTATION ( #15745, #21507 ) ;
#30296 = CARTESIAN_POINT ( 'NONE',  ( -10.01549611932653860, 203.7984951890123284, 15.35113791807856565 ) ) ;
#30297 = CARTESIAN_POINT ( 'NONE',  ( -6.500168698208129925, 202.3363017425936050, 3.201137918078566624 ) ) ;
#30298 = CARTESIAN_POINT ( 'NONE',  ( 42.22499999726879594, 149.9369285172503510, 15.58253174999999580 ) ) ;
#30299 = CARTESIAN_POINT ( 'NONE',  ( -31.74999999999995737, 7.960204194457795477E-16, -6.500000000000000000 ) ) ;
#30300 = CARTESIAN_POINT ( 'NONE',  ( 34.62499999726881583, 138.6155565068815747, -3.929120461958505118E-15 ) ) ;
#30301 = CARTESIAN_POINT ( 'NONE',  ( 3.753561863808689836, 218.3979405102790565, 31.40113791807856813 ) ) ;
#30302 = CARTESIAN_POINT ( 'NONE',  ( 127.5000000000000000, 155.0000000000000000, -98.00000000000002842 ) ) ;
#30303 = AXIS2_PLACEMENT_3D ( 'NONE', #14483, #11764, #30502 ) ;
#30304 = CARTESIAN_POINT ( 'NONE',  ( 3.135527875058820690, 216.4958274776887492, 76.40113791807857524 ) ) ;
#30305 = CARTESIAN_POINT ( 'NONE',  ( -6.139770520408368348, 215.5359834540460042, 48.95113791807857240 ) ) ;
#30306 = DIRECTION ( 'NONE',  ( 1.000000000000000000, -0.000000000000000000, -0.000000000000000000 ) ) ;
#30307 = AXIS2_PLACEMENT_3D ( 'NONE', #1702, #6819, #25213 ) ;
#30308 = DIRECTION ( 'NONE',  ( 0.000000000000000000, 0.000000000000000000, -1.000000000000000000 ) ) ;
#30309 = CARTESIAN_POINT ( 'NONE',  ( -12.01549611932659722, 210.8513442034533227, 11.64886208192143613 ) ) ;
#30310 = CARTESIAN_POINT ( 'NONE',  ( -6.220909254589682469, 215.4770327129947134, 17.94886208192143684 ) ) ;
#30311 = CARTESIAN_POINT ( 'NONE',  ( 71.99999999453763166, 155.0000000000000000, -14.50000000000000711 ) ) ;
#30312 = ORIENTED_EDGE ( 'NONE', *, *, #11183, .T. ) ;
#30313 = CARTESIAN_POINT ( 'NONE',  ( -3.753561863808691168, 195.6020594897209435, 53.90113791807858235 ) ) ;
#30314 = CARTESIAN_POINT ( 'NONE',  ( 2.517493886308900919, 214.5937144450984420, 82.40113791807856103 ) ) ;
#30315 = CARTESIAN_POINT ( 'NONE',  ( -8.118202686958138514, 212.8392687619910930, 26.79886208192143826 ) ) ;
#30316 = CARTESIAN_POINT ( 'NONE',  ( 45.11132485994280472, 140.7341522555726669, 4.635254915624211769 ) ) ;
#30317 = CIRCLE ( 'NONE', #31394, 4.000000000000000000 ) ;
#30318 = ORIENTED_EDGE ( 'NONE', *, *, #6049, .T. ) ;
#30319 = ORIENTED_EDGE ( 'NONE', *, *, #27480, .T. ) ;
#30320 = ORIENTED_EDGE ( 'NONE', *, *, #1464, .T. ) ;
#30321 = CARTESIAN_POINT ( 'NONE',  ( 42.38867513459481984, 140.7341522555726669, -4.635254915624220651 ) ) ;
#30322 = CARTESIAN_POINT ( 'NONE',  ( 6.269955739554010421, 4.268932597852939104, -6.443844059477442876 ) ) ;
#30323 = ORIENTED_EDGE ( 'NONE', *, *, #26790, .F. ) ;
#30324 = CARTESIAN_POINT ( 'NONE',  ( -4.984841277089726574, 200.2242689037092305, 33.05113791807857382 ) ) ;
#30325 = CIRCLE ( 'NONE', #30904, 5.200000000000009948 ) ;
#30326 = CARTESIAN_POINT ( 'NONE',  ( 85.71132485994282035, 155.0000000000000000, -15.00000000000002487 ) ) ;
#30327 = AXIS2_PLACEMENT_3D ( 'NONE', #2336, #14938, #30786 ) ;
#30328 = CARTESIAN_POINT ( 'NONE',  ( -8.118202686958138514, 212.8392687619910930, 17.79886208192143826 ) ) ;
#30329 = CARTESIAN_POINT ( 'NONE',  ( 56.07499999726881157, 168.2552932293087906, 9.630534252274372875 ) ) ;
#30330 = ORIENTED_EDGE ( 'NONE', *, *, #4832, .T. ) ;
#30331 = CARTESIAN_POINT ( 'NONE',  ( -8.000000000000008882, 207.0476921513413515, 48.50113791807856956 ) ) ;
#30332 = CARTESIAN_POINT ( 'NONE',  ( 67.41132485994280898, 142.2402378747194405, -9.270509831248439525 ) ) ;
#30333 = AXIS2_PLACEMENT_3D ( 'NONE', #20504, #31241, #12835 ) ;
#30334 = PRESENTATION_STYLE_ASSIGNMENT (( #22154 ) ) ;
#30335 = DIRECTION ( 'NONE',  ( -1.000000000000000000, -0.000000000000000000, -0.000000000000000000 ) ) ;
#30336 = CARTESIAN_POINT ( 'NONE',  ( 6.139770520408223575, 215.5359834540460611, 96.54886208192141339 ) ) ;
#30337 = CARTESIAN_POINT ( 'NONE',  ( 63.67499999726880588, 168.2552932293087906, -9.630534252274385310 ) ) ;
#30338 = CARTESIAN_POINT ( 'NONE',  ( -3.135527875058821579, 197.5041725223112223, 32.90113791807857524 ) ) ;
#30339 = CARTESIAN_POINT ( 'NONE',  ( 70.18867513459481700, 140.7341522555726669, 4.635254915624211769 ) ) ;
#30340 = EDGE_CURVE ( 'NONE', #10071, #33208, #15014, .T. ) ;
#30341 = CARTESIAN_POINT ( 'NONE',  ( -6.139770520408369237, 215.5359834540460042, 15.95113791807856884 ) ) ;
#30342 = AXIS2_PLACEMENT_3D ( 'NONE', #16256, #3473, #14204 ) ;
#30343 = CARTESIAN_POINT ( 'NONE',  ( 121.5000000000000000, 80.04668119422552763, -74.95331880577366235 ) ) ;
#30344 = CARTESIAN_POINT ( 'NONE',  ( 78.99999999999998579, 170.2462022514548323, -7.872454543227099337E-15 ) ) ;
#30345 = CARTESIAN_POINT ( 'NONE',  ( -57.24307706584514932, 194.9404480003898925, -2.185445380844633689 ) ) ;
#30346 = DIRECTION ( 'NONE',  ( 0.000000000000000000, 0.000000000000000000, 1.000000000000000000 ) ) ;
#30347 = CARTESIAN_POINT ( 'NONE',  ( -3.753561863808691168, 195.6020594897209435, -0.09886208192143448870 ) ) ;
#30348 = CARTESIAN_POINT ( 'NONE',  ( 22.98492866215539365, -18.48391005502967843, -1.088725517910815066 ) ) ;
#30349 = CARTESIAN_POINT ( 'NONE',  ( 50.37499999726881583, 155.0000000000000000, 15.58253174999999402 ) ) ;
#30350 = CARTESIAN_POINT ( 'NONE',  ( -8.062137200540920645, 212.9164362838581894, 48.80113791807857382 ) ) ;
#30351 = CARTESIAN_POINT ( 'NONE',  ( 80.22499999726881015, 149.9369285172503510, 15.58253174999999580 ) ) ;
#30352 = EDGE_CURVE ( 'NONE', #31659, #31983, #21700, .T. ) ;
#30353 = DIRECTION ( 'NONE',  ( 0.000000000000000000, -1.000000000000000000, 9.859324684083082301E-16 ) ) ;
#30354 = CARTESIAN_POINT ( 'NONE',  ( 50.69999999453762740, 167.3344367211045096, 8.961492836873468093 ) ) ;
#30355 =( BOUNDED_CURVE ( )  B_SPLINE_CURVE ( 2, ( #21368, #31764, #11323, #29546, #24093, #21707, #10831, #16589, #760, #31600, #3645 ),
 .UNSPECIFIED., .F., .F. ) 
 B_SPLINE_CURVE_WITH_KNOTS ( ( 3, 2, 2, 2, 2, 3 ),
 ( 0.05357142857142861703, 0.05714285714285716883, 0.06071428571428571369, 0.06428571428571425161, 0.06785714285714281035, 0.07142857142857135522 ),
 .UNSPECIFIED. ) 
 CURVE ( )  GEOMETRIC_REPRESENTATION_ITEM ( )  RATIONAL_B_SPLINE_CURVE ( ( 0.9999999999999994449, 0.9510565162951540863, 1.000000000000000000, 0.9510565162951534202, 1.000000000000000000, 0.9510565162951534202, 1.000000000000000000, 0.9510565162951534202, 1.000000000000000000, 0.9510565162951544194, 0.9999999999999990008 ) ) 
 REPRESENTATION_ITEM ( '' )  );
#30356 = EDGE_LOOP ( 'NONE', ( #32824, #8902, #21549, #22311 ) ) ;
#30357 = CARTESIAN_POINT ( 'NONE',  ( -9.680171189290831535, 214.0920067884431148, 30.80113791807857027 ) ) ;
#30358 = CIRCLE ( 'NONE', #17854, 4.000000000000000888 ) ;
#30359 = CARTESIAN_POINT ( 'NONE',  ( 125.5000000000000000, 48.99999999999998579, -2.149999999999999023 ) ) ;
#30360 = CARTESIAN_POINT ( 'NONE',  ( 10.00000000000000711, 207.0476921513415220, 6.998862081921434886 ) ) ;
#30361 = AXIS2_PLACEMENT_3D ( 'NONE', #2386, #12939, #12775 ) ;
#30362 = CYLINDRICAL_SURFACE ( 'NONE', #7428, 4.000000000000000000 ) ;
#30363 = ORIENTED_EDGE ( 'NONE', *, *, #27227, .F. ) ;
#30364 = COLOUR_RGB ( '', 0.72549020, 0.75294118, 0.79215686) ;
#30365 = CARTESIAN_POINT ( 'NONE',  ( 0.05014649552810505201, 217.5146222423826714, 4.251137918078566003 ) ) ;
#30366 = CARTESIAN_POINT ( 'NONE',  ( 8.062137200540920645, 201.0835637161417822, 65.30113791807858092 ) ) ;
#30367 = EDGE_CURVE ( 'NONE', #1999, #25547, #29186, .T. ) ;
#30368 = CARTESIAN_POINT ( 'NONE',  ( 4.984841277089891776, 200.2242689037093726, 25.44886208192143684 ) ) ;
#30369 = CIRCLE ( 'NONE', #9691, 5.250000000000004441 ) ;
#30370 = CARTESIAN_POINT ( 'NONE',  ( -60.00000000000000000, -7.347880794884118356E-15, 20.00000000000000000 ) ) ;
#30371 = EDGE_LOOP ( 'NONE', ( #11679, #20303 ) ) ;
#30372 = CARTESIAN_POINT ( 'NONE',  ( 7.984503880673485376, 204.3529502787953902, 5.151137918078566358 ) ) ;
#30373 = EDGE_CURVE ( 'NONE', #15105, #28362, #31510, .T. ) ;
#30374 = CARTESIAN_POINT ( 'NONE',  ( -47.49999999999998579, 155.0000000000000000, -6.938893903907228378E-15 ) ) ;
#30375 = CARTESIAN_POINT ( 'NONE',  ( 7.375838497908012492, 217.2372850707501186, 90.54886208192144181 ) ) ;
#30376 = CARTESIAN_POINT ( 'NONE',  ( 40.47499999726881725, 149.9369285172503510, 15.58253174999999580 ) ) ;
#30377 = ORIENTED_EDGE ( 'NONE', *, *, #32599, .F. ) ;
#30378 = CARTESIAN_POINT ( 'NONE',  ( 47.52499999726881441, 169.8198683612136222, -4.815267126137197984 ) ) ;
#30379 = CARTESIAN_POINT ( 'NONE',  ( 38.98867513459482126, 163.8167787843871110, -12.13525491562423397 ) ) ;
#30380 = CARTESIAN_POINT ( 'NONE',  ( 54.51132485994281041, 163.8167787843871110, 12.13525491562421621 ) ) ;
#30381 = CONICAL_SURFACE ( 'NONE', #24394, 31.00000000000000000, 1.466076571675244411 ) ;
#30382 = CARTESIAN_POINT ( 'NONE',  ( 10.00000000000000711, 207.0476921513415220, 72.99886208192144466 ) ) ;
#30383 = CARTESIAN_POINT ( 'NONE',  ( 46.67499999726880588, 141.7447067706911810, 9.630534252274376428 ) ) ;
#30384 = CARTESIAN_POINT ( 'NONE',  ( -3.399999999999999911, 4.163799117101000559E-16, -0.4201245229258211977 ) ) ;
#30385 = CARTESIAN_POINT ( 'NONE',  ( 6.220909254589536808, 215.4770327129947702, 7.551137918078564049 ) ) ;
#30386 = CARTESIAN_POINT ( 'NONE',  ( 58.61132485994280472, 159.8737954434936910, 14.99999999999996447 ) ) ;
#30387 = CARTESIAN_POINT ( 'NONE',  ( 57.90000000000000568, 141.2096805137202580, 4.480746418436733158 ) ) ;
#30388 = CARTESIAN_POINT ( 'NONE',  ( -0.05014649552810635652, 196.4853777576173002, 89.75113791807854113 ) ) ;
#30389 = CARTESIAN_POINT ( 'NONE',  ( 47.71132485994280614, 155.0000000000000000, -15.00000000000002487 ) ) ;
#30390 = CARTESIAN_POINT ( 'NONE',  ( -7.984503880673422316, 204.3529502787951628, 80.34886208192143897 ) ) ;
#30391 = LINE ( 'NONE', #22552, #4759 ) ;
#30392 = DIRECTION ( 'NONE',  ( -1.000000000000000000, 0.000000000000000000, 0.000000000000000000 ) ) ;
#30393 = CARTESIAN_POINT ( 'NONE',  ( 12.00000000000000711, 207.0476921513415220, 84.99886208192144466 ) ) ;
#30394 = VECTOR ( 'NONE', #14288, 1000.000000000000000 ) ;
#30395 = CARTESIAN_POINT ( 'NONE',  ( 65.22499999726881015, 160.0630714827496206, -15.58253175000000823 ) ) ;
#30397 = ORIENTED_EDGE ( 'NONE', *, *, #25539, .T. ) ;
#30396 = CARTESIAN_POINT ( 'NONE',  ( 6.220909254589536808, 215.4770327129947987, 22.55113791807856671 ) ) ;
#30398 = LINE ( 'NONE', #30227, #22245 ) ;
#30399 = CARTESIAN_POINT ( 'NONE',  ( 84.57499999726880446, 145.8408176439707802, 12.60653300113718345 ) ) ;
#30400 = CARTESIAN_POINT ( 'NONE',  ( -7.456977232089304408, 196.8216656703010301, 90.05113791807858092 ) ) ;
#30401 = EDGE_CURVE ( 'NONE', #25104, #534, #10653, .T. ) ;
#30402 = ADVANCED_FACE ( 'NONE', ( #26412 ), #10428, .F. ) ;
#30403 = CARTESIAN_POINT ( 'NONE',  ( 72.58867513459482268, 146.1832212156128890, -12.13525491562423042 ) ) ;
#30404 = VERTEX_POINT ( 'NONE', #15521 ) ;
#30405 = CARTESIAN_POINT ( 'NONE',  ( -0.05014649552828442242, 219.6175466908591716, 72.24886208192143044 ) ) ;
#30406 = CARTESIAN_POINT ( 'NONE',  ( 10.00000000000000711, 207.0476921513415220, 72.99886208192144466 ) ) ;
#30407 = CARTESIAN_POINT ( 'NONE',  ( 7.375838497908012492, 217.2372850707501186, 18.54886208192143116 ) ) ;
#30408 = CARTESIAN_POINT ( 'NONE',  ( -27.50000000000000000, 0.000000000000000000, -18.00000000000000000 ) ) ;
#30409 = AXIS2_PLACEMENT_3D ( 'NONE', #14193, #26966, #21692 ) ;
#30410 = CARTESIAN_POINT ( 'NONE',  ( 6.139770520408368348, 198.4640165459539674, 35.45113791807857240 ) ) ;
#30411 = DIRECTION ( 'NONE',  ( 0.000000000000000000, 0.000000000000000000, 1.000000000000000000 ) ) ;
#30412 = EDGE_CURVE ( 'NONE', #17539, #25041, #10753, .T. ) ;
#30413 = CARTESIAN_POINT ( 'NONE',  ( -3.044812012439970683, 197.4746971517856196, 100.8988620819214361 ) ) ;
#30414 = AXIS2_PLACEMENT_3D ( 'NONE', #19102, #29490, #24383 ) ;
#30415 = CARTESIAN_POINT ( 'NONE',  ( -52.50000000000002132, 155.0000000000000000, 17.00000000000001066 ) ) ;
#30416 = VERTEX_POINT ( 'NONE', #20800 ) ;
#30417 = FACE_BOUND ( 'NONE', #13502, .T. ) ;
#30418 = CARTESIAN_POINT ( 'NONE',  ( 2.517493886309087436, 199.4062855549015865, 76.59886208192142476 ) ) ;
#30419 = EDGE_CURVE ( 'NONE', #18729, #2221, #5467, .T. ) ;
#30420 = VERTEX_POINT ( 'NONE', #18251 ) ;
#30421 = AXIS2_PLACEMENT_3D ( 'NONE', #12973, #2415, #10919 ) ;
#30422 = PLANE ( 'NONE',  #5875 ) ;
#30423 = VERTEX_POINT ( 'NONE', #15853 ) ;
#30424 = CARTESIAN_POINT ( 'NONE',  ( 76.32499999726881867, 145.8408176439707802, 12.60653300113718345 ) ) ;
#30425 = CARTESIAN_POINT ( 'NONE',  ( 25.25067902531500508, -17.17577847294298721, -16.29357272760982767 ) ) ;
#30426 = CARTESIAN_POINT ( 'NONE',  ( 4.984841277089725686, 213.7757310962907411, 82.55113791807858092 ) ) ;
#30427 = LINE ( 'NONE', #29919, #10767 ) ;
#30428 = CARTESIAN_POINT ( 'NONE',  ( 43.20000000000000995, 167.3344367211045096, 8.961492836873468093 ) ) ;
#30429 = CARTESIAN_POINT ( 'NONE',  ( 8.015496119326595448, 204.4483345814782638, 58.14886208192145034 ) ) ;
#30430 = CONICAL_SURFACE ( 'NONE', #15737, 3.499999999999999556, 1.047197551196589638 ) ;
#30431 = CARTESIAN_POINT ( 'NONE',  ( 6.539198257601831266, 3.775407874310744649, -6.286450516130488886 ) ) ;
#30432 = DIRECTION ( 'NONE',  ( 0.000000000000000000, 0.000000000000000000, 1.000000000000000000 ) ) ;
#30433 = FACE_OUTER_BOUND ( 'NONE', #19925, .T. ) ;
#30434 = CARTESIAN_POINT ( 'NONE',  ( 50.12499999726881583, 155.0000000000000000, 15.58253174999999402 ) ) ;
#30435 = CARTESIAN_POINT ( 'NONE',  ( 61.17499999726882010, 145.8408176439707802, -12.60653300113719588 ) ) ;
#30436 = CARTESIAN_POINT ( 'NONE',  ( -3.753561863808691168, 195.6020594897209435, 53.90113791807858235 ) ) ;
#30437 = CARTESIAN_POINT ( 'NONE',  ( -124.3127766070272315, -5.250000000000003553, 35.00001199999999812 ) ) ;
#30438 = CARTESIAN_POINT ( 'NONE',  ( 10.00000000000000711, 206.9523078486586201, 101.0011379180785696 ) ) ;
#30439 = EDGE_CURVE ( 'NONE', #20133, #28893, #5296, .T. ) ;
#30440 = CARTESIAN_POINT ( 'NONE',  ( -6.139770520408368348, 215.5359834540460042, 75.95113791807857240 ) ) ;
#30441 = CARTESIAN_POINT ( 'NONE',  ( -7.456977232089471386, 217.1783343296987709, 44.94886208192144039 ) ) ;
#30442 = CARTESIAN_POINT ( 'NONE',  ( -8.118202686958138514, 212.8392687619910930, 50.79886208192143471 ) ) ;
#30443 = DIRECTION ( 'NONE',  ( -1.000000000000000000, -0.000000000000000000, 0.000000000000000000 ) ) ;
#30444 = CARTESIAN_POINT ( 'NONE',  ( -9.736236675707914401, 199.9851607334237542, 87.20113791807858661 ) ) ;
#30445 = CARTESIAN_POINT ( 'NONE',  ( 83.41132485994282320, 142.2402378747194405, -9.270509831248439525 ) ) ;
#30446 = CARTESIAN_POINT ( 'NONE',  ( 6.139770520408368348, 198.4640165459539674, 5.451137918078567068 ) ) ;
#30447 = CARTESIAN_POINT ( 'NONE',  ( -10.01549611932659722, 210.2015048109875011, 65.64886208192143613 ) ) ;
#30448 = CYLINDRICAL_SURFACE ( 'NONE', #20534, 13.00000000000002487 ) ;
#30449 = ORIENTED_EDGE ( 'NONE', *, *, #27442, .F. ) ;
#30450 = CARTESIAN_POINT ( 'NONE',  ( 11.98450388067341876, 210.9467285061363953, 69.84886208192143897 ) ) ;
#30451 = ORIENTED_EDGE ( 'NONE', *, *, #33516, .T. ) ;
#30452 = CARTESIAN_POINT ( 'NONE',  ( 79.77499999726880731, 169.8198683612136222, -4.815267126137197984 ) ) ;
#30453 = CARTESIAN_POINT ( 'NONE',  ( -6.500168698208244500, 211.6636982574061676, 50.79886208192144892 ) ) ;
#30454 = AXIS2_PLACEMENT_3D ( 'NONE', #9018, #22302, #14129 ) ;
#30455 = ORIENTED_EDGE ( 'NONE', *, *, #28746, .F. ) ;
#30456 = CARTESIAN_POINT ( 'NONE',  ( 84.57499999726880446, 145.8408176439707802, 12.60653300113718345 ) ) ;
#30457 = CARTESIAN_POINT ( 'NONE',  ( 4.000000000000001776, 2.694222958124178486E-16, 2.200000000000001066 ) ) ;
#30458 = DIRECTION ( 'NONE',  ( 0.000000000000000000, -1.000000000000000000, 1.290957005378097920E-14 ) ) ;
#30459 = CARTESIAN_POINT ( 'NONE',  ( 58.82499999726881867, 141.7447067706911810, -9.630534252274385310 ) ) ;
#30460 = SURFACE_SIDE_STYLE ('',( #12054 ) ) ;
#30461 = CARTESIAN_POINT ( 'NONE',  ( 9.984503880673420539, 210.2968891136705167, 45.84886208192141765 ) ) ;
#30462 = VERTEX_POINT ( 'NONE', #4967 ) ;
#30463 = DIRECTION ( 'NONE',  ( 1.000000000000000000, -0.000000000000000000, -0.000000000000000000 ) ) ;
#30464 = FILL_AREA_STYLE ('',( #7124 ) ) ;
#30465 = DIRECTION ( 'NONE',  ( -1.000000000000000000, 0.000000000000000000, 0.000000000000000000 ) ) ;
#30466 = FACE_OUTER_BOUND ( 'NONE', #28790, .T. ) ;
#30467 = CARTESIAN_POINT ( 'NONE',  ( -4.984841277089891776, 213.7757310962905990, 26.94886208192142973 ) ) ;
#30468 = CARTESIAN_POINT ( 'NONE',  ( -8.118202686958039038, 201.1607312380087080, 57.20113791807857950 ) ) ;
#30469 = CARTESIAN_POINT ( 'NONE',  ( 8.118202686958039038, 212.8392687619912635, 49.70113791807857240 ) ) ;
#30470 = CARTESIAN_POINT ( 'NONE',  ( 3.135527875058820690, 216.4958274776887492, 13.40113791807856636 ) ) ;
#30471 = CARTESIAN_POINT ( 'NONE',  ( 2.517493886308900919, 214.5937144450984420, 1.401137918078566136 ) ) ;
#30472 = CARTESIAN_POINT ( 'NONE',  ( 53.12499999726881583, 155.0000000000000000, -15.58253175000000823 ) ) ;
#30473 = LINE ( 'NONE', #30299, #4024 ) ;
#30474 = CARTESIAN_POINT ( 'NONE',  ( 87.49999999999998579, 148.5314199800102415, -13.68475861882792088 ) ) ;
#30475 = CARTESIAN_POINT ( 'NONE',  ( -7.375838497908182134, 217.2372850707499765, 24.95113791807856884 ) ) ;
#30476 = DIRECTION ( 'NONE',  ( 0.000000000000000000, -0.04769215134144040580, 0.9988620819214356628 ) ) ;
#30477 = CARTESIAN_POINT ( 'NONE',  ( -10.01549611932653860, 203.7984951890123284, 72.35113791807859229 ) ) ;
#30478 = CARTESIAN_POINT ( 'NONE',  ( 10.00000000000000711, 206.9523078486586201, 47.00113791807856956 ) ) ;
#30479 = DIRECTION ( 'NONE',  ( 1.000000000000000000, 0.000000000000000000, 0.000000000000000000 ) ) ;
#30480 = CARTESIAN_POINT ( 'NONE',  ( 117.5000000000000000, 155.0000000000000000, -6.938893903907228378E-15 ) ) ;
#30481 = CARTESIAN_POINT ( 'NONE',  ( 12.00000000000000711, 207.0476921513415220, 15.99886208192143400 ) ) ;
#30482 = CARTESIAN_POINT ( 'NONE',  ( 6.139770520408223575, 215.5359834540460611, 21.54886208192143826 ) ) ;
#30483 = CARTESIAN_POINT ( 'NONE',  ( 74.69999999453764872, 167.3344367211045096, 8.961492836873468093 ) ) ;
#30484 = EDGE_LOOP ( 'NONE', ( #10352, #15406, #4842, #11299 ) ) ;
#30485 = CARTESIAN_POINT ( 'NONE',  ( 9.736236675707914401, 214.0148392665762458, 55.70113791807856529 ) ) ;
#30486 = CARTESIAN_POINT ( 'NONE',  ( 0.05014649552807626948, 215.4116977939061144, 82.25113791807856956 ) ) ;
#30487 = CARTESIAN_POINT ( 'NONE',  ( 9.984503880673420539, 210.2968891136705167, 39.84886208192141765 ) ) ;
#30488 = DIRECTION ( 'NONE',  ( -1.000000000000000000, -0.000000000000000000, -0.000000000000000000 ) ) ;
#30489 = VERTEX_POINT ( 'NONE', #26244 ) ;
#30490 = ORIENTED_EDGE ( 'NONE', *, *, #9346, .F. ) ;
#30491 = ORIENTED_EDGE ( 'NONE', *, *, #16249, .T. ) ;
#30492 = EDGE_CURVE ( 'NONE', #23167, #22913, #26069, .T. ) ;
#30493 = CARTESIAN_POINT ( 'NONE',  ( 58.08867513459483689, 142.2402378747194405, 9.270509831248432420 ) ) ;
#30494 = CARTESIAN_POINT ( 'NONE',  ( 32.50000000000000000, 155.0000000000000000, -6.938893903907228378E-15 ) ) ;
#30495 = ORIENTED_EDGE ( 'NONE', *, *, #14373, .F. ) ;
#30496 = CARTESIAN_POINT ( 'NONE',  ( 7.984503880673485376, 204.3529502787953902, 35.15113791807856103 ) ) ;
#30497 = DIRECTION ( 'NONE',  ( 0.000000000000000000, 0.9988620819214357738, 0.04769215134144196705 ) ) ;
#30498 = CARTESIAN_POINT ( 'NONE',  ( -9.984503880673420539, 203.7031108863293980, 11.34886208192143187 ) ) ;
#30499 = CARTESIAN_POINT ( 'NONE',  ( 56.47499999726882436, 149.9369285172503510, 15.58253174999999580 ) ) ;
#30500 = ORIENTED_EDGE ( 'NONE', *, *, #32635, .T. ) ;
#30501 = CARTESIAN_POINT ( 'NONE',  ( -4.903702542908602524, 213.8346818373418898, 63.95113791807857240 ) ) ;
#30502 = DIRECTION ( 'NONE',  ( 0.000000000000000000, 0.000000000000000000, 1.000000000000000000 ) ) ;
#30503 = DIRECTION ( 'NONE',  ( -1.000000000000000000, 0.000000000000000000, 0.000000000000000000 ) ) ;
#30504 = CARTESIAN_POINT ( 'NONE',  ( -8.118202686958138514, 212.8392687619910930, 101.7988620819214418 ) ) ;
#30505 = CARTESIAN_POINT ( 'NONE',  ( 65.47499999726881015, 160.0630714827496206, -15.58253175000000823 ) ) ;
#30506 = CARTESIAN_POINT ( 'NONE',  ( 10.00000000000000711, 206.9523078486586201, 35.00113791807856956 ) ) ;
#30507 = DIRECTION ( 'NONE',  ( 0.000000000000000000, 0.7071067811865442421, -0.7071067811865506814 ) ) ;
#30508 = CARTESIAN_POINT ( 'NONE',  ( 0.05014649552810505201, 217.5146222423826714, 22.25113791807856956 ) ) ;
#30509 = DIRECTION ( 'NONE',  ( 1.000000000000000000, 0.000000000000000000, 0.000000000000000000 ) ) ;
#30510 = CONICAL_SURFACE ( 'NONE', #15820, 32.00000000000002842, 0.1047197551196217685 ) ;
#30511 = CARTESIAN_POINT ( 'NONE',  ( 82.20000000000000284, 142.6655632788954620, -8.961492836873480528 ) ) ;
#30512 = CARTESIAN_POINT ( 'NONE',  ( -56.32919368135717519, 194.9806731544236982, 1.250698461946182505 ) ) ;
#30513 = CARTESIAN_POINT ( 'NONE',  ( 108.0049454219347354, 155.0000000000000000, -12.10452846326765020 ) ) ;
#30514 = CARTESIAN_POINT ( 'NONE',  ( -3.753561863808691168, 195.6020594897209435, 2.901137918078565470 ) ) ;
#30515 = PLANE ( 'NONE',  #27075 ) ;
#30516 = CARTESIAN_POINT ( 'NONE',  ( 52.37499999726881583, 155.0000000000000000, 15.58253174999999402 ) ) ;
#30517 = CARTESIAN_POINT ( 'NONE',  ( 6.139770520408368348, 198.4640165459539674, 44.45113791807855819 ) ) ;
#30518 = CARTESIAN_POINT ( 'NONE',  ( 83.82499999726880446, 168.2552932293087906, 9.630534252274372875 ) ) ;
#30519 = PLANE ( 'NONE',  #32606 ) ;
#30520 = CARTESIAN_POINT ( 'NONE',  ( -6.875000000000001776, -4.690970937165714894, -7.298562697733108173 ) ) ;
#30521 = CARTESIAN_POINT ( 'NONE',  ( 51.99999999453763166, 155.0000000000000000, -14.50000000000000711 ) ) ;
#30522 = ORIENTED_EDGE ( 'NONE', *, *, #22521, .F. ) ;
#30523 = CARTESIAN_POINT ( 'NONE',  ( -7.456977232089304408, 196.8216656703010301, 30.05113791807857027 ) ) ;
#30524 = DIRECTION ( 'NONE',  ( -1.000000000000000000, 0.000000000000000000, 0.000000000000000000 ) ) ;
#30525 = CARTESIAN_POINT ( 'NONE',  ( 6.220909254589681581, 198.5229672870052582, 13.44886208192143151 ) ) ;
#30526 = APPLICATION_CONTEXT ( 'automotive_design' ) ;
#30527 = CARTESIAN_POINT ( 'NONE',  ( 4.000000000000003553, 0.000000000000000000, 0.000000000000000000 ) ) ;
#30528 = ORIENTED_EDGE ( 'NONE', *, *, #19093, .F. ) ;
#30529 = CARTESIAN_POINT ( 'NONE',  ( 8.062137200540920645, 201.0835637161417822, 2.301137918078566269 ) ) ;
#30530 = CARTESIAN_POINT ( 'NONE',  ( -9.984503880673473830, 210.2968891136704315, 60.65113791807856103 ) ) ;
#30531 = ORIENTED_EDGE ( 'NONE', *, *, #21202, .F. ) ;
#30532 = CARTESIAN_POINT ( 'NONE',  ( -8.000000000000008882, 206.9523078486584780, 20.49886208192143755 ) ) ;
#30533 = EDGE_CURVE ( 'NONE', #10180, #2728, #28810, .T. ) ;
#30534 = CARTESIAN_POINT ( 'NONE',  ( 0.000000000000000000, 0.000000000000000000, 0.000000000000000000 ) ) ;
#30535 = CIRCLE ( 'NONE', #3868, 5.249999999999997335 ) ;
#30536 = VERTEX_POINT ( 'NONE', #30871 ) ;
#30537 = CARTESIAN_POINT ( 'NONE',  ( -7.984503880673488041, 209.6470497212046098, 3.651137918078566802 ) ) ;
#30538 = EDGE_CURVE ( 'NONE', #30979, #29388, #8126, .T. ) ;
#30539 = FACE_OUTER_BOUND ( 'NONE', #26921, .T. ) ;
#30540 = CARTESIAN_POINT ( 'NONE',  ( -3.662846001189865142, 195.5725841191952838, 91.89886208192143613 ) ) ;
#30541 = CARTESIAN_POINT ( 'NONE',  ( 35.77499999726881441, 169.8198683612136222, -4.815267126137197984 ) ) ;
#30542 = ORIENTED_EDGE ( 'NONE', *, *, #4964, .T. ) ;
#30543 = CARTESIAN_POINT ( 'NONE',  ( 42.22499999726879594, 149.9369285172503510, 15.58253174999999580 ) ) ;
#30544 = CARTESIAN_POINT ( 'NONE',  ( 39.08867513459482268, 167.7597621252805880, -9.270509831248443078 ) ) ;
#30545 = EDGE_CURVE ( 'NONE', #19921, #24261, #5663, .T. ) ;
#30546 = CARTESIAN_POINT ( 'NONE',  ( 54.21132485994281325, 170.7719333635740497, -7.904646289410545231E-15 ) ) ;
#30547 = CARTESIAN_POINT ( 'NONE',  ( 0.05014649552828275708, 196.4853777576173002, 73.74886208192144466 ) ) ;
#30548 = CARTESIAN_POINT ( 'NONE',  ( 50.27499999726880731, 160.0630714827496206, 15.58253174999999402 ) ) ;
#30549 = CARTESIAN_POINT ( 'NONE',  ( 10.00000000000000178, 0.000000000000000000, 0.000000000000000000 ) ) ;
#30550 = CARTESIAN_POINT ( 'NONE',  ( -6.220909254589537696, 198.5229672870051161, 0.05113791807856577637 ) ) ;
#30551 = CARTESIAN_POINT ( 'NONE',  ( 58.51132485994281041, 163.8167787843871110, 12.13525491562421621 ) ) ;
#30552 = CARTESIAN_POINT ( 'NONE',  ( 61.10000000000000142, 168.7903194862797420, 4.480746418436729606 ) ) ;
#30553 =( BOUNDED_CURVE ( )  B_SPLINE_CURVE ( 2, ( #11031, #17473, #22250, #28035, #11863, #6579, #6749, #27858, #32637, #1307, #19532 ),
 .UNSPECIFIED., .F., .F. ) 
 B_SPLINE_CURVE_WITH_KNOTS ( ( 3, 2, 2, 2, 2, 3 ),
 ( 0.6964285714285713969, 0.6999999999999999556, 0.7035714285714286254, 0.7071428571428570731, 0.7107142857142856318, 0.7142857142857141906 ),
 .UNSPECIFIED. ) 
 CURVE ( )  GEOMETRIC_REPRESENTATION_ITEM ( )  RATIONAL_B_SPLINE_CURVE ( ( 1.000000000000000000, 0.9510565162951534202, 1.000000000000000000, 0.9510565162951534202, 1.000000000000000000, 0.9510565162951534202, 1.000000000000000000, 0.9510565162951534202, 1.000000000000000000, 0.9510565162951549745, 0.9999999999999984457 ) ) 
 REPRESENTATION_ITEM ( '' )  );
#30554 = CARTESIAN_POINT ( 'NONE',  ( -10.01549611932653860, 203.7984951890123284, 93.35113791807857808 ) ) ;
#30555 = CARTESIAN_POINT ( 'NONE',  ( 2.000000000000000000, 1.773042676681340968, -2.276824562219559311E-15 ) ) ;
#30556 = CARTESIAN_POINT ( 'NONE',  ( 10.01549611932653860, 210.2015048109876716, 70.85113791807854966 ) ) ;
#30557 = CARTESIAN_POINT ( 'NONE',  ( -6.625705691649848461, 5.306270977113102916, -7.795653906409009792 ) ) ;
#30558 = CARTESIAN_POINT ( 'NONE',  ( 33.67499999726881299, 168.2552932293087906, -9.630534252274385310 ) ) ;
#30559 = CARTESIAN_POINT ( 'NONE',  ( 9.736236675708031640, 199.9851607334238963, 91.29886208192142760 ) ) ;
#30560 = CARTESIAN_POINT ( 'NONE',  ( 64.62499999726881583, 138.6155565068815463, -3.929120461958505118E-15 ) ) ;
#30562 = ORIENTED_EDGE ( 'NONE', *, *, #18354, .T. ) ;
#30561 = CARTESIAN_POINT ( 'NONE',  ( -8.062137200540920645, 212.9164362838581894, 33.80113791807857382 ) ) ;
#30563 = CARTESIAN_POINT ( 'NONE',  ( -58.82891977373553516, 194.9228321189716837, -2.483646737656201253 ) ) ;
#30564 = CARTESIAN_POINT ( 'NONE',  ( 86.77499999726882152, 140.1801316387863778, 4.815267126137185549 ) ) ;
#30565 = CARTESIAN_POINT ( 'NONE',  ( -9.736236675707914401, 199.9851607334237542, 84.20113791807858661 ) ) ;
#30566 = B_SPLINE_CURVE_WITH_KNOTS ( 'NONE', 3,
 ( #23348, #30681, #10244, #7678, #28291, #28455 ),
 .UNSPECIFIED., .F., .F.,
 ( 4, 2, 4 ),
 ( 2.475503369227215526E-07, 0.002222330217055624568, 0.004444412883774326306 ),
 .UNSPECIFIED. ) ;
#30567 = ADVANCED_FACE ( 'NONE', ( #15510 ), #31351, .T. ) ;
#30568 = FACE_OUTER_BOUND ( 'NONE', #21839, .T. ) ;
#30569 = ORIENTED_EDGE ( 'NONE', *, *, #33554, .T. ) ;
#30570 = CARTESIAN_POINT ( 'NONE',  ( 6.139770520408223575, 215.5359834540460611, 84.54886208192142760 ) ) ;
#30571 = CIRCLE ( 'NONE', #16958, 27.50000000000000355 ) ;
#30572 = CARTESIAN_POINT ( 'NONE',  ( 11.98450388067341876, 210.9467285061363953, 15.84886208192143719 ) ) ;
#30573 = CARTESIAN_POINT ( 'NONE',  ( -6.837824896291514243, 3.947820044545427454, -6.564402953523716278 ) ) ;
#30574 = CARTESIAN_POINT ( 'NONE',  ( -10.00000000000000711, 207.0476921513413515, 33.50113791807856956 ) ) ;
#30575 = CARTESIAN_POINT ( 'NONE',  ( -1.211595439868048629, 7.960739084487649109, -0.4504974108211966533 ) ) ;
#30576 = CARTESIAN_POINT ( 'NONE',  ( -3.135527875058982783, 216.4958274776886924, 99.09886208192143897 ) ) ;
#30577 = EDGE_CURVE ( 'NONE', #21804, #15528, #5281, .T. ) ;
#30578 = DIRECTION ( 'NONE',  ( 0.000000000000000000, 0.000000000000000000, -1.000000000000000000 ) ) ;
#30579 = ORIENTED_EDGE ( 'NONE', *, *, #16616, .T. ) ;
#30580 = CARTESIAN_POINT ( 'NONE',  ( -9.945352646237287431, 205.9548993908332193, 104.4520571433695579 ) ) ;
#30581 = CARTESIAN_POINT ( 'NONE',  ( -4.984841277089891776, 213.7757310962905990, 77.94886208192143329 ) ) ;
#30582 = EDGE_LOOP ( 'NONE', ( #16567, #17829, #1764, #20559, #25258 ) ) ;
#30583 = CARTESIAN_POINT ( 'NONE',  ( 125.5000000000000000, 155.0000000000000000, -6.938893903907228378E-15 ) ) ;
#30584 = EDGE_LOOP ( 'NONE', ( #19041, #14098, #20050, #26261 ) ) ;
#30585 = CARTESIAN_POINT ( 'NONE',  ( 0.000000000000000000, 0.000000000000000000, -16.57418492358057094 ) ) ;
#30586 = CIRCLE ( 'NONE', #1732, 5.000000000000000888 ) ;
#30587 = CARTESIAN_POINT ( 'NONE',  ( 73.67499999726879878, 168.2552932293087906, -9.630534252274387086 ) ) ;
#30588 = CARTESIAN_POINT ( 'NONE',  ( 82.82499999726881867, 141.7447067706911810, -9.630534252274385310 ) ) ;
#30589 = CARTESIAN_POINT ( 'NONE',  ( -7.500000000000000000, 0.7513028741560130452, -0.02472015219302865774 ) ) ;
#30590 = CARTESIAN_POINT ( 'NONE',  ( 4.903702542908601636, 200.1653181626581102, 83.45113791807857240 ) ) ;
#30591 = EDGE_CURVE ( 'NONE', #2685, #3624, #1036, .T. ) ;
#30592 = CARTESIAN_POINT ( 'NONE',  ( 3.499999999999996891, 0.000000000000000000, 2.066666666666666430 ) ) ;
#30594 = AXIS2_PLACEMENT_3D ( 'NONE', #26854, #3515, #21244 ) ;
#30593 = SHAPE_REPRESENTATION_RELATIONSHIP ( 'NONE' , 'NONE' ,  #17198, #15696 ) ;
#30595 = CARTESIAN_POINT ( 'NONE',  ( 44.90000000000000568, 168.7903194862797420, -4.480746418436745593 ) ) ;
#30596 = CARTESIAN_POINT ( 'NONE',  ( -7.984503880673422316, 204.3529502787951628, 53.34886208192144608 ) ) ;
#30597 = ADVANCED_FACE ( 'NONE', ( #2899 ), #13286, .T. ) ;
#30598 = CARTESIAN_POINT ( 'NONE',  ( -6.500000000000000888, -2.534234941938113828, -0.3584823952106175882 ) ) ;
#30599 = CARTESIAN_POINT ( 'NONE',  ( -2.352990130084580066E-16, 8.660254037844390851, -7.422398894150034288 ) ) ;
#30600 = CARTESIAN_POINT ( 'NONE',  ( -126.3741763928861985, 5.113356552508657948, 35.00001199999999812 ) ) ;
#30601 = CARTESIAN_POINT ( 'NONE',  ( 57.22499999726880304, 160.0630714827496206, -15.58253175000000823 ) ) ;
#30602 = CARTESIAN_POINT ( 'NONE',  ( 66.47499999726882436, 149.9369285172503510, 15.58253174999999580 ) ) ;
#30603 = CARTESIAN_POINT ( 'NONE',  ( -7.375838497908182134, 217.2372850707499765, 60.95113791807857240 ) ) ;
#30604 = CARTESIAN_POINT ( 'NONE',  ( -67.50000000000000000, 155.0000000000000000, 37.00000000000001421 ) ) ;
#30605 = EDGE_CURVE ( 'NONE', #5147, #25169, #14084, .T. ) ;
#30606 = CARTESIAN_POINT ( 'NONE',  ( 3.044812012440130555, 197.4746971517856764, 101.6011379180785781 ) ) ;
#30607 = CARTESIAN_POINT ( 'NONE',  ( 6.139770520408367460, 198.4640165459539389, 74.45113791807857240 ) ) ;
#30608 = CARTESIAN_POINT ( 'NONE',  ( -9.680171189290716072, 199.9079932115567146, 47.19886208192143329 ) ) ;
#30609 = AXIS2_PLACEMENT_3D ( 'NONE', #5692, #18485, #31756 ) ;
#30610 = CARTESIAN_POINT ( 'NONE',  ( 8.062137200540822946, 212.9164362838583315, 51.69886208192143329 ) ) ;
#30611 = CARTESIAN_POINT ( 'NONE',  ( -6.500000000000000000, 1.602771114417265164, -0.1495523863686162858 ) ) ;
#30612 = CARTESIAN_POINT ( 'NONE',  ( -7.375838497908182134, 217.2372850707499765, 87.95113791807857240 ) ) ;
#30613 = FACE_OUTER_BOUND ( 'NONE', #19422, .T. ) ;
#30614 = CARTESIAN_POINT ( 'NONE',  ( 8.118202686958039038, 212.8392687619912635, 7.701137918078566180 ) ) ;
#30615 = CARTESIAN_POINT ( 'NONE',  ( -8.118202686958138514, 212.8392687619910930, 68.79886208192144181 ) ) ;
#30616 = FACE_OUTER_BOUND ( 'NONE', #16890, .T. ) ;
#30617 = ORIENTED_EDGE ( 'NONE', *, *, #32005, .F. ) ;
#30618 = CARTESIAN_POINT ( 'NONE',  ( 12.00000000000000711, 207.0476921513415220, 75.99886208192144466 ) ) ;
#30619 = ORIENTED_EDGE ( 'NONE', *, *, #11053, .T. ) ;
#30620 = CARTESIAN_POINT ( 'NONE',  ( 77.87499999726881583, 171.3844434931184253, -7.942151717890132712E-15 ) ) ;
#30621 = CARTESIAN_POINT ( 'NONE',  ( 7.984503880673422316, 209.6470497212048372, 51.84886208192144608 ) ) ;
#30622 = B_SPLINE_CURVE_WITH_KNOTS ( 'NONE', 3,
 ( #33128, #9794, #20178, #30575, #7237, #17625 ),
 .UNSPECIFIED., .F., .F.,
 ( 4, 2, 4 ),
 ( 0.004444412883774334112, 0.006655097293744431999, 0.008865781703714530754 ),
 .UNSPECIFIED. ) ;
#30623 = VECTOR ( 'NONE', #1279, 1000.000000000000000 ) ;
#30624 = VERTEX_POINT ( 'NONE', #23355 ) ;
#30625 = CARTESIAN_POINT ( 'NONE',  ( 70.32499999726881867, 145.8408176439707802, 12.60653300113718345 ) ) ;
#30626 = CARTESIAN_POINT ( 'NONE',  ( 32.50000000000000000, 155.0000000000000000, -15.00000000000002487 ) ) ;
#30627 = CARTESIAN_POINT ( 'NONE',  ( -56.25248981486732447, 194.9849645003486387, 1.107065583161625621 ) ) ;
#30628 = CARTESIAN_POINT ( 'NONE',  ( 64.92499999726881299, 145.8408176439707802, -12.60653300113719588 ) ) ;
#30629 = ADVANCED_FACE ( 'NONE', ( #9900 ), #28118, .T. ) ;
#30630 = SURFACE_STYLE_FILL_AREA ( #20229 ) ;
#30631 = EDGE_CURVE ( 'NONE', #32869, #33215, #6485, .T. ) ;
#30632 = CARTESIAN_POINT ( 'NONE',  ( -8.118202686958138514, 212.8392687619910930, 41.79886208192143471 ) ) ;
#30633 = ORIENTED_EDGE ( 'NONE', *, *, #18880, .F. ) ;
#30634 = DIRECTION ( 'NONE',  ( 0.000000000000000000, 0.000000000000000000, -1.000000000000000000 ) ) ;
#30635 = AXIS2_PLACEMENT_3D ( 'NONE', #5627, #21294, #31688 ) ;
#30636 = CARTESIAN_POINT ( 'NONE',  ( 127.5000000000000000, 80.04668119422662187, 74.95331880577468553 ) ) ;
#30637 = CARTESIAN_POINT ( 'NONE',  ( 125.0000000000000000, 3.061616997868383121E-14, -20.00000000000000355 ) ) ;
#30638 = CARTESIAN_POINT ( 'NONE',  ( -8.015496119326597224, 209.5516654185217362, 29.64886208192143968 ) ) ;
#30639 = CARTESIAN_POINT ( 'NONE',  ( 3.044812012440130555, 197.4746971517856764, 74.60113791807856387 ) ) ;
#30640 = CARTESIAN_POINT ( 'NONE',  ( 45.18867513459481700, 169.2658477444273331, -4.635254915624224203 ) ) ;
#30641 = ADVANCED_FACE ( 'NONE', ( #4315, #27482, #20151, #11813, #17098 ), #6870, .F. ) ;
#30642 = CARTESIAN_POINT ( 'NONE',  ( -3.135527875058821579, 197.5041725223112223, 50.90113791807856813 ) ) ;
#30643 = CARTESIAN_POINT ( 'NONE',  ( -8.062137200540920645, 212.9164362838581894, 18.80113791807856671 ) ) ;
#30644 = CARTESIAN_POINT ( 'NONE',  ( 7.984503880673485376, 204.3529502787953902, 8.151137918078566358 ) ) ;
#30645 = CIRCLE ( 'NONE', #5080, 2.149999999999994138 ) ;
#30646 = CARTESIAN_POINT ( 'NONE',  ( -65.20000000000000284, 0.9203920079924619024, 19.30000000000001847 ) ) ;
#30647 = CARTESIAN_POINT ( 'NONE',  ( 35.82499999726880446, 168.2552932293087906, 9.630534252274372875 ) ) ;
#30648 = CARTESIAN_POINT ( 'NONE',  ( 9.680171189290831535, 199.9079932115568852, 32.30113791807855961 ) ) ;
#30649 = LINE ( 'NONE', #25529, #4807 ) ;
#30650 = CIRCLE ( 'NONE', #19205, 1.535500000000000087 ) ;
#30651 = CARTESIAN_POINT ( 'NONE',  ( -8.062137200540920645, 212.9164362838581894, 75.80113791807858092 ) ) ;
#30652 = CARTESIAN_POINT ( 'NONE',  ( 10.00000000000000711, 206.9523078486586201, 50.00113791807856956 ) ) ;
#30653 = CIRCLE ( 'NONE', #30103, 15.00000000000001776 ) ;
#30654 = DIRECTION ( 'NONE',  ( 1.000000000000000000, 0.000000000000000000, 0.000000000000000000 ) ) ;
#30655 = CARTESIAN_POINT ( 'NONE',  ( 5.000000000000000000, 3.513898075855356851, -2.028750000000006271 ) ) ;
#30656 = CARTESIAN_POINT ( 'NONE',  ( -3.662846001189865142, 195.5725841191952838, 16.89886208192143613 ) ) ;
#30657 = CARTESIAN_POINT ( 'NONE',  ( 10.01549611932659367, 203.7984951890124421, 19.14886208192143258 ) ) ;
#30658 = CARTESIAN_POINT ( 'NONE',  ( 73.39999999453763735, 141.2096805137202580, 4.480746418436733158 ) ) ;
#30659 = ORIENTED_EDGE ( 'NONE', *, *, #4170, .T. ) ;
#30660 = CARTESIAN_POINT ( 'NONE',  ( -3.662846001190052991, 218.4274158808045740, 55.10113791807857808 ) ) ;
#30661 = CARTESIAN_POINT ( 'NONE',  ( 4.984841277089725686, 213.7757310962907411, 79.55113791807858092 ) ) ;
#30662 = CARTESIAN_POINT ( 'NONE',  ( -6.139770520408224463, 198.4640165459539389, 44.04886208192143471 ) ) ;
#30663 = CARTESIAN_POINT ( 'NONE',  ( 104.9083388212530537, 155.0000000000000000, -32.00000000000000000 ) ) ;
#30664 = ORIENTED_EDGE ( 'NONE', *, *, #12713, .F. ) ;
#30665 = AXIS2_PLACEMENT_3D ( 'NONE', #5194, #15579, #17806 ) ;
#30666 = ORIENTED_EDGE ( 'NONE', *, *, #537, .F. ) ;
#30667 = ORIENTED_EDGE ( 'NONE', *, *, #7473, .F. ) ;
#30668 = PRODUCT_DEFINITION_SHAPE ( 'NONE', 'NONE',  #14589 ) ;
#30669 = CARTESIAN_POINT ( 'NONE',  ( 51.38867513459482694, 169.2658477444273331, 4.635254915624208216 ) ) ;
#30670 = CARTESIAN_POINT ( 'NONE',  ( 127.5000000000000000, 152.8499999999996533, -106.0000000000000000 ) ) ;
#30671 = EDGE_LOOP ( 'NONE', ( #24100, #32225, #22236, #5313, #26581, #26214, #29728, #29435 ) ) ;
#30672 = STYLED_ITEM ( 'NONE', ( #22502 ), #11828 ) ;
#30673 = CARTESIAN_POINT ( 'NONE',  ( 2.517493886308900919, 214.5937144450984420, 28.40113791807856813 ) ) ;
#30674 = CIRCLE ( 'NONE', #17037, 2.149999999999985256 ) ;
#30675 = CARTESIAN_POINT ( 'NONE',  ( 55.61132485994281183, 150.1262045565064227, -15.00000000000002665 ) ) ;
#30676 = CARTESIAN_POINT ( 'NONE',  ( 3.044812012439969795, 216.5253028482143520, 15.39886208192143613 ) ) ;
#30677 = AXIS2_PLACEMENT_3D ( 'NONE', #31894, #1071, #23899 ) ;
#30678 = CARTESIAN_POINT ( 'NONE',  ( 54.27499999726880731, 160.0630714827496206, 15.58253174999999224 ) ) ;
#30679 = ORIENTED_EDGE ( 'NONE', *, *, #33469, .T. ) ;
#30680 = CARTESIAN_POINT ( 'NONE',  ( 0.05014649552807626948, 215.4116977939061144, 55.25113791807857666 ) ) ;
#30681 = CARTESIAN_POINT ( 'NONE',  ( 6.901579824520443829, -4.675625068323827627, -0.7022220667781372549 ) ) ;
#30682 =( NAMED_UNIT ( * ) PLANE_ANGLE_UNIT ( ) SI_UNIT ( $, .RADIAN. ) );
#30683 = LINE ( 'NONE', #6657, #32561 ) ;
#30684 = CARTESIAN_POINT ( 'NONE',  ( 8.000000000000008882, 207.0476921513415220, 0.9988620819214347746 ) ) ;
#30685 = CARTESIAN_POINT ( 'NONE',  ( 64.57499999726881867, 145.8408176439707802, 12.60653300113718345 ) ) ;
#30686 = CARTESIAN_POINT ( 'NONE',  ( 8.118202686958039038, 212.8392687619912635, 46.70113791807857240 ) ) ;
#30687 = DIRECTION ( 'NONE',  ( 1.000000000000000000, 0.000000000000000000, 0.000000000000000000 ) ) ;
#30688 = CARTESIAN_POINT ( 'NONE',  ( -9.984503880673473830, 210.2968891136704315, 15.65113791807856813 ) ) ;
#30689 = CARTESIAN_POINT ( 'NONE',  ( 6.220909254589680693, 198.5229672870052582, 100.4488620819214475 ) ) ;
#30690 = STYLED_ITEM ( 'NONE', ( #30334 ), #31568 ) ;
#30691 = CARTESIAN_POINT ( 'NONE',  ( 84.90000000000000568, 168.7903194862797420, -4.480746418436745593 ) ) ;
#30692 = DIRECTION ( 'NONE',  ( 1.000000000000000000, 0.000000000000000000, 0.000000000000000000 ) ) ;
#30693 = DIRECTION ( 'NONE',  ( 0.01265860800194867734, -0.08535984102820122488, -0.9962697712884263090 ) ) ;
#30694 = CARTESIAN_POINT ( 'NONE',  ( 7.456977232089302632, 217.1783343296989131, 4.551137918078565825 ) ) ;
#30695 = CARTESIAN_POINT ( 'NONE',  ( 125.5000000000000000, 155.0000000000000000, -112.0000000000000711 ) ) ;
#30696 = CARTESIAN_POINT ( 'NONE',  ( 48.47499999726880304, 149.9369285172503510, 15.58253174999999580 ) ) ;
#30697 = CARTESIAN_POINT ( 'NONE',  ( 8.062137200540920645, 201.0835637161417822, 50.30113791807857382 ) ) ;
#30698 = DIRECTION ( 'NONE',  ( 0.000000000000000000, 0.000000000000000000, -1.000000000000000000 ) ) ;
#30699 = CARTESIAN_POINT ( 'NONE',  ( 52.51132485994281041, 163.8167787843871110, 12.13525491562421621 ) ) ;
#30700 = COLOUR_RGB ( '', 0.40784314, 0.44705882, 0.49803922) ;
#30701 = CARTESIAN_POINT ( 'NONE',  ( 51.39999999453763735, 141.2096805137202580, 4.480746418436733158 ) ) ;
#30702 = EDGE_LOOP ( 'NONE', ( #10517, #10755, #30619, #15923 ) ) ;
#30703 = CARTESIAN_POINT ( 'NONE',  ( -3.662846001190052991, 218.4274158808045740, 34.10113791807857098 ) ) ;
#30704 = CARTESIAN_POINT ( 'NONE',  ( 47.01132485994281041, 142.2402378747194405, 9.270509831248432420 ) ) ;
#30705 = CARTESIAN_POINT ( 'NONE',  ( 10.01549611932659545, 203.7984951890123853, 13.14886208192143258 ) ) ;
#30706 = CARTESIAN_POINT ( 'NONE',  ( 2.466666666666999408, 0.000000000000000000, 2.066666666667000385 ) ) ;
#30707 = B_SPLINE_CURVE_WITH_KNOTS ( 'NONE', 3,
 ( #3115, #13665, #21837, #5505, #15894, #5831 ),
 .UNSPECIFIED., .F., .F.,
 ( 4, 2, 4 ),
 ( 0.002044882221487550125, 0.003063384235218505856, 0.004081886248949461587 ),
 .UNSPECIFIED. ) ;
#30708 = ORIENTED_EDGE ( 'NONE', *, *, #3053, .T. ) ;
#30709 = CARTESIAN_POINT ( 'NONE',  ( -6.220909254589537696, 198.5229672870051161, 9.051137918078561384 ) ) ;
#30710 = CARTESIAN_POINT ( 'NONE',  ( 6.139770520408368348, 198.4640165459539674, 62.45113791807857950 ) ) ;
#30711 =( BOUNDED_SURFACE ( )  B_SPLINE_SURFACE ( 3, 2, ( 
 ( #7194, #33080, #14851, #12299, #32572, #6851, #24912, #25077, #4462, #14355, #11635, #11791, #12133, #9750, #9570, #27464, #22184, #14685, #11965, #32914, #1573, #20134, #30529, #22018, #6520, #25413, #17579, #30195, #19632, #16900, #27972, #6688, #32738, #4639, #9242, #30365, #15024, #4296, #17239, #17077, #7027, #17411, #32401, #3954, #27797, #9066, #27298, #24749, #1404, #28319, #41, #12809, #23200, #33254, #12983, #10437, #9920, #28488, #15530, #2086, #31049, #4803, #15196, #25754, #20305, #33594, #12472, #30709, #20809, #23030, #7371, #20477, #25588, #23377, #17750, #2252, #10276, #12633, #28144, #20654, #7546, #22863, #33427, #10100, #30879, #17932, #18092, #7876, #31212, #4977, #15363, #7707, #2426, #5142, #25922, #2594, #30470, #14625, #32674, #1846, #32847, #9681, #12066, #33194, #20240, #32509, #17005, #12575, #9858, #30296, #6789, #4062, #22804, #17177, #9510, #25524, #9340, #20075, #17689, #25178, #1674, #27561, #7132, #6964, #9181, #24846, #14786, #17353, #22454, #17515, #1510, #12236, #30643, #27738, #19897, #30131, #27904, #4401, #2193, #19734, #4227, #7312, #28076, #25021, #22622, #6620, #4738, #14451, #33010, #14962, #4576, #25350, #2020, #12409, #15129, #19570, #29963, #27400, #11907, #22292, #15799, #10541, #23473, #28593, #5414, #8149, #2860, #15474, #140, #31144, #20418, #18532, #26361, #15298, #7474, #5574, #25865, #12751, #301, #30811, #23142, #20922, #33530, #17859, #15632, #2531, #15966, #28914, #10700, #26192, #13244, #10203, #18201, #12914, #2706, #23641, #25690, #22967, #20588, #31315, #21078, #7981, #5077, #30989, #26036, #23310, #18365, #22248, #31482, #3020, #33366, #28257, #10041, #4911, #20747, #7646, #2360, #18028, #28423, #10374, #7810, #5243, #28757, #13084, #14341, #32390, #887, #22007, #29850, #3606, #19446, #29345, #24737, #29675, #11126, #9231, #26609, #3437, #19283, #22169, #11284, #1220, #30011, #21670, #6158, #24564, #11779, #32063, #19114, #9054, #24224, #27286, #6509, #8724, #8887, #16553, #6327, #24053, #16887, #29504, #26947, #3941, #14000, #19621, #1391, #6674, #5992, #32557, #1064, #3272, #13660, #3783, #722, #21501, #31888, #8556, #18950, #16380, #26772, #13834, #24397, #11452, #21831, #32222, #16720, #27122, #14171, #11618, #32725, #19790, #23017, #24898, #1721, #25400, #12121, #4790, #11955, #14837, #33415, #17399, #9392, #27959, #30184, #30517, #7182, #1559, #15183, #10089, #22338, #9909, #7360, #27453, #2072, #6840, #27613, #22679, #17226, #17566, #30866, #4107, #25575, #22512, #4282, #9559, #14673, #28129, #14499, #25067, #4628, #32901, #19951, #9735, #30350, #20466, #12623, #2240, #20291, #17739, #7013, #12287, #27785, #15011, #30697, #4449, #17061, #25236, #12459, #1900, #22851, #33065, #20123, #33243, #7863, #18414, #20797, #8196, #28966, #7531, #25741, #21292, #18581, #5292, #15518, #12797, #31527, #25909, #18248, #523, #7696, #28807, #10748, #26087, #13455, #13131, #5463, #15685, #17917, #33582, #23524, #2755, #31197, #15849, #10261, #192, #5624, #10589, #28637, #5130, #26239, #20966, #10915, #18078, #2582, #16016, #26408, #28, #31360, #15351, #3066, #23188, #12969, #23686, #13295, #347, #21128, #28474, #8029, #2910, #28308, #23848, #4963, #2412, #20638, #31037, #23364, #10425, #14126, #16848, #11572, #24185, #8841, #6113, #29131, #27241, #1351, #24016, #16173, #14290, #3396, #16509, #3895, #11236, #27073, #18745, #26734, #8680, #680, #5779, #21961, #24348, #24692, #21623, #19072, #29298, #29461, #32350, #9014, #31846, #11738, #26908, #26563, #11412, #5950, #847, #31686, #1175, #3233, #3736, #32017, #13790, #3566, #8356, #13956, #18904, #32181, #21788, #1016, #13619, #11082, #19241, #29636, #6283, #19403, #24519, #16340, #29805, #6465, #16676, #21463, #8510, #9864, #25186, #6629, #4745, #22125, #32680, #14793, #17695, #6796, #30477, #25530, #17184, #1681, #20082, #7318, #27567, #14632, #27912, #19743, #22810, #2028, #4234, #4408, #12074, #1854, #19578, #4582, #30139, #22464, #33201, #25029, #15136, #30651, #2199, #1516, #25357, #30304, #12414, #20247, #33018, #29971, #28083, #32515, #17015, #9188, #14969, #27408, #4069, #32855, #14457, #11913, #22299, #24853, #9347, #9518, #22631, #19904, #6971, #17359, #27745, #12244, #7139, #9688, #17523, #7483, #10382, #18539, #12921, #4918, #23481, #25697, #7653, #18035, #28921, #20929, #28430, #10048, #17868, #30997, #20754, #5421, #147, #13091, #18208, #28765, #31489, #26199, #5086, #10549, #31151, #20425, #8157, #15975, #15305, #30818, #5581, #15481, #7819, #26368, #26043, #2714, #28264, #10707, #12581, #2369, #15806, #2867, #22974, #31322, #12758, #23149, #28599, #33537, #7988, #33374, #10211, #21086, #25872, #20595, #2539, #23317, #23648, #14074, #5250, #18373, #15641, #13253, #308, #16302, #29757, #32310, #14082, #6246, #27029, #23976, #31969, #26692, #16464, #29595, #5740, #3027, #3195, #3522, #16633, #969, #18859, #13584, #6070, #3353, #13915, #13744, #3691, #24477, #13413, #21252, #16803, #1138, #807, #11036, #8312, #11532, #21419, #24141, #6422, #638, #24300, #21914, #21576, #8974, #8639, #11369, #11197, #23807, #29092, #19032, #29420, #26865, #21748, #16131, #32138, #19363, #8800, #19197, #31805, #479, #10876, #31645, #8470, #29255, #18705, #26524, #5907, #9476, #1314, #17479, #32472, #22256, #9643, #32977, #20039, #30438, #27363, #27706, #19864, #30606, #12204, #27200, #4031, #4368, #7098, #25142, #9306, #14420 ),
 ( #27864, #12031, #33161, #32810, #14750, #1639, #3856, #19537, #30262, #22419, #17144, #1807, #29931, #6924, #4538, #24989, #4191, #24813, #22591, #27530, #20205, #1475, #11871, #25317, #1982, #19698, #17316, #11702, #14929, #9140, #32643, #12372, #22769, #9824, #7271, #30092, #14248, #24648, #22086, #6584, #16968, #6758, #14590, #5210, #18168, #23272, #106, #3277, #31285, #10164, #28562, #25833, #15092, #13664, #21506, #10000, #2159, #730, #23107, #2496, #24059, #31115, #7777, #25486, #16225, #11131, #12542, #10508, #7945, #28041, #25998, #7438, #28219, #33669, #22932, #15596, #31893, #4702, #26615, #2324, #33327, #20547, #17818, #28722, #20384, #4876, #2669, #15265, #30776, #10344, #30952, #17653, #25657, #5829, #20887, #18327, #12712, #12879, #7614, #13051, #33495, #17998, #28389, #5046, #15437, #20715, #23441, #22176, #32566, #8729, #4114, #19288, #3442, #22013, #16558, #1069, #27459, #11787, #13840, #14348, #11457, #24404, #3612, #24904, #16725, #29510, #9060, #32396, #24571, #1567, #11289, #27128, #21836, #3790, #30018, #24744, #26953, #3948, #9237, #29680, #1399, #21676, #6681, #11627, #26778, #11960, #8562, #19120, #1228, #14506, #14005, #16894, #22344, #32229, #8892, #6515, #18956, #6335, #14177, #19627, #6165, #17068, #29350, #19454, #29857, #27291, #5998, #16385, #24229, #892, #32069, #10095, #1907, #25747, #7538, #2419, #12127, #2247, #7188, #12629, #23024, #9915, #30190, #17925, #12803, #27619, #33421, #4796, #20472, #15358, #27791, #4290, #22520, #32907, #14679, #4970, #15191, #33249, #25073, #1727, #32732, #6846, #17406, #7366, #4455, #30874, #9565, #30523, #9400, #33072, #19959, #20298, #30357, #14844, #25242, #19797, #17745, #12293, #17234, #7021, #22686, #9744, #28136, #20129, #17573, #27966, #4634, #15018, #28314, #25407, #2078, #12466, #22858, #25582, #30703, #7870, #2761, #21134, #8363, #28643, #15690, #28973, #20803, #23855, #3076, #5299, #5470, #13138, #15856, #20646, #5633, #31205, #23531, #530, #26093, #16182, #31693, #26571, #2589, #26415, #31369, #13464, #10923, #356, #31043, #18754, #3240, #18085, #21299, #16024, #29138, #5786, #18254, #28482, #12976, #23372, #5137, #23195, #33589, #23694, #15524, #25916, #10269, #7702, #200, #31533, #10598, #35, #10431, #20974, #8037, #18421, #28813, #10756, #26247, #2918, #13302, #8203, #18588, #19081, #11090, #18912, #32025, #26916, #9023, #687, #8689, #24358, #16347, #21470, #27249, #6291, #29980, #3574, #1025, #11247, #11420, #3904, #14299, #13799, #9196, #21797, #8519, #27082, #21632, #6121, #32523, #16856, #29306, #19412, #16517, #29469, #13963, #6638, #32190, #855, #14134, #3745, #29644, #17023, #26741, #8849, #19249, #16685, #1358, #29814, #24529, #6473, #24701, #1184, #11746, #3403, #22133, #11580, #31854, #27417, #13627, #24193, #21970, #32358, #19586, #24024, #5958, #22473, #2206, #12588, #30313, #20090, #11921, #28091, #9356, #32864, #20256, #9873, #30660, #7327, #4243, #4592, #30485, #7492, #22818, #4077, #12252, #17703, #25365, #14978, #9698, #4754, #22982, #15145, #6980, #2037, #22640, #1525, #33381, #17876, #30148, #22307, #20432, #9526, #33028, #10055, #17533, #27920, #32688, #30825, #14465, #19751, #25538, #24862, #6805, #12424, #27577, #14640, #7148, #17192, #33209, #25037, #1689, #12083, #19913, #17367, #27753, #4417, #14803, #25195, #1863, #28771, #18043, #12766, #20935, #7826, #21257, #23814, #5587, #31495, #18544, #15488, #23487, #18214, #7993, #21093, #31004, #28271, #28436, #5426, #8162, #26205, #10388, #5093, #31327, #28605, #15811, #5256, #28927, #15981, #4926, #23157, #8318, #26373, #26049, #2545, #33544, #3033, #12929, #15650, #31651, #25879, #2873, #13418, #13096, #485, #153, #13258, #2719, #15313, #20602, #10556, #18379, #23654, #313, #7660, #10712, #10882, #25705, #2377, #23324, #10220, #8657, #20761, #31158, #13589, #8805, #32477, #5745, #16810, #3360, #26530, #11202, #8475, #29762, #16137, #18864, #19203, #29262, #3201, #11375, #31976, #11707, #14255, #6428, #21920, #8981, #5913, #13920, #8646, #32143, #11537, #21424, #18712, #16308, #29601, #32315, #16638, #812, #26697, #21754, #19037, #6251, #29426, #19368, #27205, #29097, #23983, #644, #3861, #16471, #13751, #11042, #24654, #24146, #6075, #22092, #21581, #27034, #1319, #3527, #31810, #24305, #3698, #26870, #976, #14088, #24482, #1144, #32816, #20045, #11877, #1814, #20211, #6929, #19871, #6764, #7104, #9481, #2164, #9311, #27535, #7278, #17659, #1645, #25148, #16973, #33167, #14426, #4197, #25322, #14934, #1988, #12377, #19704, #9649, #12209, #12547, #27870, #9146, #17322, #22775, #30444, #17484, #14755, #9831, #28047, #30612, #12038, #4545, #27712, #6590, #4708, #22938, #1481, #27369, #25493, #14597, #4373, #15097, #22596, #32984, #4036, #19543, #29936, #24818, #22262, #32649, #30098, #17149, #24994, #30267, #22425, #31290, #23278, #26332, #33500, #18003, #31453, #8122, #33334, #15601, #25662, #278, #13216, #15443, #26004, #33674, #2676, #30782, #5386, #30959, #10348, #10673, #2501, #2998, #18504, #13377, #12719, #2831, #7782, #23614, #21052, #10513, #7443, #28889, #10006, #28225, #5544, #15771, #15935, #20389, #28394, #4883, #23112, #10172, #15270, #17823, #26164, #111, #2331, #20552, #7619, #5052, #25839, #7951, #12885, #20720, #31119, #18173, #28567, #5215, #13056, #20893, #23446, #18334, #28727, #29723, #32108, #29221, #21217, #29057, #8440, #3321, #19161, #10844, #18827 ),
 ( #8942, #26995, #18666, #29558, #16272, #5873, #26658, #6385, #31935, #11000, #24265, #13882, #6039, #16773, #26492, #8605, #13705, #19002, #11503, #6212, #31774, #16600, #3656, #773, #14050, #3160, #21881, #26827, #8279, #27172, #23775, #16430, #3827, #8771, #441, #29392, #24446, #11333, #935, #3491, #1110, #19332, #32276, #24105, #21718, #31612, #5709, #16097, #13550, #23942, #604, #21380, #11169, #21545, #33124, #27669, #4337, #22055, #12341, #20174, #32439, #7068, #4503, #24617, #22565, #3998, #24786, #19838, #9106, #14721, #28009, #1278, #22737, #32612, #19502, #6727, #14395, #25286, #11672, #1442, #25112, #11837, #29901, #6891, #27501, #7234, #9791, #1952, #17450, #14894, #22222, #9448, #4158, #1773, #27833, #16937, #14219, #9275, #12174, #30572, #32950, #30061, #19669, #17282, #14555, #9611, #24953, #17622, #6554, #27333, #17118, #1611, #12001, #22387, #32776, #30234, #20007, #30407, #15403, #31414, #4844, #25961, #7915, #23240, #10638, #10312, #2636, #12846, #4675, #30746, #20688, #33634, #28359, #15564, #7405, #31087, #15735, #2465, #25801, #2292, #13020, #5013, #8083, #15235, #23071, #2800, #5346, #23412, #9962, #17788, #28687, #20349, #33463, #20852, #10476, #31251, #18295, #25624, #5179, #12676, #76, #26133, #7746, #13182, #28187, #23579, #18131, #22902, #21015, #15060, #10134, #28530, #247, #20516, #18467, #25455, #30919, #17968, #2129, #12513, #7582, #33296, #11137, #21178, #29516, #8733, #10964, #21512, #18794, #31898, #26294, #896, #26455, #29183, #6172, #31736, #21841, #3616, #32232, #8241, #32073, #3284, #19125, #16563, #6003, #2966, #14011, #8898, #23735, #26957, #11296, #24409, #11462, #23904, #401, #18629, #29019, #10804, #1074, #21682, #29355, #31575, #5676, #28853, #13344, #13510, #3450, #569, #5509, #16066, #26620, #15898, #5836, #3121, #16392, #21340, #8408, #16231, #13669, #13846, #24066, #736, #8572, #18962, #26784, #24233, #6339, #14354, #30024, #22017, #27132, #33386, #11964, #2382, #32571, #6687, #16899, #17076, #10060, #20437, #19461, #15318, #27463, #14182, #32737, #27297, #11790, #4932, #22988, #24576, #25546, #22183, #1403, #24748, #12771, #4118, #6519, #19803, #9407, #1572, #23162, #32400, #14510, #9241, #24911, #7499, #2211, #19631, #22348, #30194, #33550, #6850, #3953, #17238, #27626, #4295, #19293, #9065, #15150, #12593, #30833, #17882, #28278, #25711, #29685, #16731, #3794, #1233, #29861, #11634, #13264, #28443, #26536, #10228, #20767, #2880, #5751, #28611, #18549, #13594, #5262, #23493, #8168, #29103, #10394, #20608, #26211, #2551, #10888, #23820, #26054, #23659, #160, #318, #7666, #15987, #7832, #10561, #21263, #13102, #3206, #18718, #23988, #23331, #13423, #18385, #490, #31656, #21100, #18049, #16143, #31011, #5098, #8325, #26378, #15493, #25884, #15656, #12935, #497, #31164, #18220, #2727, #3039, #10717, #20940, #31332, #8000, #28777, #5433, #28934, #15819, #31500, #5594, #32148, #6596, #983, #26703, #11542, #13758, #29431, #6080, #16978, #8986, #16478, #31816, #5918, #19042, #13925, #29769, #21430, #26875, #11380, #3365, #8481, #14260, #27041, #27375, #24312, #21759, #31984, #8809, #24661, #1324, #818, #29941, #19209, #29268, #14094, #8651, #3532, #19547, #3867, #16313, #6435, #24151, #29607, #16816, #27212, #11712, #22097, #11208, #1149, #3705, #4041, #19373, #650, #6256, #32484, #21927, #32319, #16642, #9152, #14431, #11048, #24488, #18871, #21589, #22268, #20395, #28233, #17154, #9317, #7449, #30273, #32990, #10014, #4553, #14940, #32653, #22945, #30788, #19708, #17665, #15106, #1488, #33173, #14603, #1649, #30450, #30106, #25328, #4889, #11882, #33341, #9488, #6769, #17329, #24998, #2170, #27540, #12043, #1995, #22431, #4203, #17490, #4379, #17830, #24824, #12553, #28053, #25500, #32823, #20051, #14761, #12385, #4714, #19877, #6937, #27719, #22782, #25154, #9838, #1822, #12215, #27876, #22603, #20218, #9658, #7111, #30618, #7286, #12728, #26169, #20899, #33679, #28399, #23118, #10518, #5057, #23286, #15776, #30965, #15606, #117, #10353, #5392, #31124, #26010, #20727, #15276, #20560, #18179, #7787, #28572, #2683, #7625, #5221, #31295, #13061, #23451, #15451, #7957, #18340, #25669, #18008, #25845, #28732, #2338, #33505, #2506, #12890, #10178, #25442, #19827, #10124, #17959, #30223, #4833, #2279, #22374, #20336, #1761, #22554, #17610, #6878, #2118, #25789, #32763, #20505, #30393, #17267, #4489, #12161, #23061, #9436, #32939, #12501, #9600, #27656, #4665, #25274, #5003, #7572, #33453, #15224, #12663, #19993, #7221, #1939, #22890, #25613, #14708, #11988, #7055, #33282, #30907, #9949, #27820, #17437, #15049, #12328, #30735, #22724, #28349, #15391, #4324, #25100, #14881, #33112, #9778, #20162, #30559, #27999, #7395, #17776, #28174, #2623, #23726, #5667, #21004, #8398, #8071, #389, #10629, #2455, #28519, #18456, #31402, #26123, #13335, #5168, #28843, #13498, #236, #13171, #66, #10792, #2791, #29174, #13010, #20839, #560, #3109, #21166, #7735, #15554, #26445, #18120, #31242, #18619, #8230, #29006, #16056, #23403, #2956, #5499, #5824, #31563, #12836, #15888, #23892, #10953, #21328, #26282, #31725, #18784, #16218, #28674, #23227, #33623, #10303, #20679, #31077, #25948, #10465, #7904, #18285, #5333, #15724, #23567, #29218, #21878, #19961, #5870, #3824, #18999, #6036, #1107, #24101, #19329, #9746, #16268, #27794, #13879, #3318, #21715, #29389, #7023, #26655, #16427, #29719, #26823 ),
 ( #769, #8939, #3487, #32105, #14846, #32910, #11166, #1729, #8768, #11330, #24262, #12296, #3653, #932, #6382, #16770, #11500, #22688, #31932, #14047, #19158, #24443, #17408, #12129, #29554, #24614, #9567, #6208, #22525, #8602, #4458, #32272, #13702, #33075, #21542, #16597, #27169, #25246, #26991, #14216, #30360, #1911, #33425, #18087, #5302, #20301, #20131, #2423, #12468, #20805, #38, #2249, #12806, #10097, #23197, #17575, #25919, #17747, #20474, #31207, #23026, #13141, #28645, #23534, #33251, #23374, #28316, #10434, #7873, #31046, #27969, #15692, #202, #15021, #18256, #2591, #26096, #2763, #15193, #25410, #9917, #30705, #2082, #30525, #12979, #30876, #7191, #22860, #33591, #4972, #7542, #7704, #7368, #10272, #4636, #17927, #15360, #28140, #28484, #25749, #4800, #25584, #12630, #20651, #5139, #15526, #15859, #13304, #857, #26251, #5636, #26743, #16349, #3405, #13801, #10758, #11092, #3242, #13966, #29309, #10601, #18757, #24195, #31857, #21472, #16184, #11251, #29473, #21635, #3078, #8521, #29141, #8039, #6124, #24362, #2921, #28816, #26919, #16027, #5788, #16520, #24026, #689, #18425, #32028, #5472, #20976, #13629, #8692, #31370, #18914, #358, #21136, #26574, #23696, #5960, #31536, #8205, #19084, #28975, #18590, #13466, #26417, #3577, #23858, #532, #10926, #21301, #31695, #8365, #14302, #27755, #30315, #12086, #4245, #25039, #21973, #29983, #24703, #14467, #27579, #3750, #1030, #1187, #1527, #14643, #32691, #16859, #11583, #4079, #1361, #11924, #11748, #1691, #22476, #11422, #19252, #14805, #32867, #32525, #9025, #6294, #9528, #19414, #22135, #4419, #32361, #22309, #19915, #19589, #6982, #6641, #9359, #9199, #21800, #32192, #17370, #29816, #8852, #27252, #24532, #29647, #16688, #6478, #19754, #3906, #27086, #27419, #17025, #14138, #24864, #30150, #6808, #17194, #12427, #20434, #4757, #4928, #18045, #27922, #25198, #25368, #25708, #28439, #23159, #7329, #2039, #28274, #25542, #2379, #15147, #25881, #12931, #1866, #9700, #5258, #2547, #22985, #33211, #30487, #15490, #9875, #2208, #18216, #22821, #12768, #5095, #10057, #31161, #30828, #33546, #33383, #12255, #17535, #7495, #17879, #12590, #10223, #4595, #15315, #23327, #20605, #31008, #20259, #7662, #5384, #28607, #30662, #17706, #10391, #20763, #7829, #7150, #14981, #22642, #28094, #33031, #20093, #21427, #8478, #18866, #15814, #16139, #8322, #19039, #647, #15652, #23816, #29264, #3203, #26532, #21259, #31813, #815, #5915, #8165, #13591, #487, #13099, #11205, #29428, #7995, #156, #31979, #21096, #10885, #21585, #29100, #5747, #23490, #16310, #10558, #26051, #18715, #26699, #2723, #23985, #5430, #26208, #31653, #20937, #11045, #3362, #31329, #13754, #18381, #24148, #8648, #28773, #2877, #13260, #23656, #315, #10714, #18546, #31497, #28930, #5591, #15984, #26375, #3036, #13420, #22428, #11539, #14257, #24996, #19545, #29939, #13923, #9314, #3529, #6077, #32480, #30101, #16474, #14428, #29604, #16640, #11709, #979, #6593, #19874, #26872, #4200, #24484, #24309, #32317, #6253, #17151, #11377, #27038, #16975, #3701, #21756, #9148, #19370, #32819, #1647, #27537, #19706, #6766, #14091, #1321, #29765, #27371, #32651, #8807, #32145, #1146, #4038, #14600, #24821, #21923, #8983, #1484, #6431, #11879, #16813, #12040, #9484, #19206, #27209, #3863, #24657, #22094, #22264, #1819, #20556, #4549, #7282, #23283, #30447, #17826, #33503, #15101, #2504, #2167, #28228, #4711, #30270, #22598, #12550, #25496, #20215, #7446, #32987, #22942, #7622, #28050, #17662, #27873, #4886, #30615, #33677, #7108, #14937, #28397, #30962, #15273, #12212, #9653, #18006, #20048, #25325, #12724, #2335, #23115, #10175, #17487, #30785, #25151, #5055, #15448, #25843, #12888, #1991, #12381, #22778, #33170, #9835, #10351, #6933, #33338, #25666, #17325, #10010, #4376, #20392, #27716, #14758, #8443, #15604, #18508, #26663, #21058, #13059, #31615, #114, #15774, #26167, #3325, #29061, #2834, #18177, #26008, #5389, #281, #16101, #7785, #13219, #31458, #23449, #28570, #607, #13381, #13709, #10676, #8125, #18338, #28892, #11003, #21383, #20897, #16275, #5547, #2679, #447, #28730, #23618, #5877, #23946, #10516, #26495, #15939, #26336, #3001, #24108, #23778, #7955, #21220, #10848, #8282, #777, #31293, #18669, #5712, #3164, #18830, #13555, #31778, #29224, #20723, #31122, #5219, #13885, #32616, #14222, #29395, #27505, #11172, #21721, #3830, #6731, #29562, #19506, #14559, #6216, #24449, #9109, #30065, #11337, #21548, #27175, #3495, #11841, #24790, #26998, #24620, #1113, #1281, #8609, #16940, #8774, #11506, #22227, #14053, #4164, #19673, #24959, #24268, #14398, #19335, #1447, #9280, #22059, #19005, #17122, #31938, #3659, #938, #6043, #16434, #32111, #11676, #19166, #26830, #32442, #21884, #16603, #32281, #8946, #29726, #6388, #16777, #29904, #6557, #27336, #4002, #4341, #1614, #1777, #2134, #4848, #33301, #17454, #12178, #4679, #1956, #12517, #14898, #2297, #23075, #12005, #19842, #15408, #12681, #33129, #9615, #6895, #25628, #20011, #12345, #28363, #22569, #22907, #15239, #20179, #7587, #7238, #9966, #9796, #22391, #27675, #17626, #30576, #25290, #20354, #14725, #28013, #33468, #15064, #22741, #32954, #30750, #25459, #5017, #30413, #7073, #10138, #20520, #7409, #17288, #25116, #30923, #27837, #4507, #17792, #28191, #17972, #32780, #9453, #30238, #18473, #29188, #10809, #25806, #251, #18634, #13348, #26298, #31419, #8246, #10968 ),
 ( #28857, #16070, #2469, #406, #15568, #2640, #8087, #20692, #15902, #5840, #12851, #23910, #10480, #33638, #2804, #29023, #28535, #13515, #5513, #10317, #8412, #23244, #13025, #2970, #21345, #20857, #21183, #31091, #31255, #5350, #23739, #31740, #25966, #7750, #31580, #18135, #26459, #5680, #7920, #3125, #15741, #573, #5184, #18798, #23416, #26137, #80, #28691, #18300, #13186, #23583, #10642, #21019, #24413, #29864, #19464, #27136, #13673, #24752, #9244, #11141, #6524, #22021, #3957, #32574, #11301, #21516, #29360, #16397, #31902, #22186, #32403, #19130, #11638, #9068, #32078, #24071, #900, #24579, #21686, #14357, #8576, #14015, #19634, #16568, #18966, #3798, #6008, #8737, #29522, #30027, #1237, #6176, #740, #26789, #26961, #3620, #16902, #3289, #1079, #11466, #3454, #13850, #27300, #8904, #16235, #21845, #32238, #24237, #19297, #1407, #11793, #29689, #26626, #6343, #16736, #14185, #14687, #32916, #25591, #9923, #1575, #12475, #9572, #22530, #1736, #23033, #14854, #27630, #7197, #30532, #22695, #33430, #9411, #25251, #19965, #1917, #28148, #22867, #25079, #2089, #20309, #30713, #11967, #12136, #33258, #7374, #17753, #4806, #6853, #17583, #33084, #10103, #25417, #6691, #12302, #15199, #27975, #4642, #9754, #2256, #12637, #20480, #30368, #15027, #20138, #4123, #17079, #27466, #32740, #24914, #14514, #7030, #22351, #19806, #30197, #17242, #4298, #17413, #27799, #4465, #23540, #21592, #7549, #5920, #20657, #7710, #2769, #25758, #21433, #11383, #17935, #29434, #15533, #4980, #23380, #31052, #8653, #28322, #18095, #31818, #28492, #15367, #208, #10440, #24316, #26877, #19044, #820, #31986, #5145, #26101, #20812, #11051, #24154, #33598, #30883, #25925, #8483, #11210, #29270, #12986, #2598, #18874, #31216, #16315, #7880, #6083, #16480, #2429, #12812, #23204, #3534, #28650, #45, #10279, #13927, #18261, #5308, #986, #15699, #26706, #13148, #3368, #13760, #27378, #9321, #29944, #21762, #14097, #4044, #6600, #11715, #32656, #24491, #14434, #32826, #19550, #32487, #19376, #19712, #22100, #14765, #21930, #6438, #19880, #22434, #30109, #27045, #1153, #25158, #11545, #6259, #4382, #27215, #16982, #6942, #1491, #11886, #29611, #25001, #19212, #32152, #24827, #12047, #8812, #6773, #32323, #8989, #22271, #16645, #17157, #1825, #3708, #30276, #16819, #29772, #14263, #3871, #9492, #24664, #1327, #27543, #9155, #4208, #14606, #1652, #17332, #27722, #23290, #15455, #2510, #33176, #7453, #25503, #25674, #5062, #14944, #12218, #12388, #12733, #25849, #10182, #28057, #22785, #15280, #12558, #23122, #2173, #12894, #33683, #22606, #30453, #26015, #10357, #10018, #20222, #17494, #20731, #30621, #22950, #5225, #9841, #33509, #31128, #30792, #18183, #17835, #20565, #20399, #32993, #4556, #28237, #4893, #33346, #30969, #25331, #2343, #7792, #7629, #18012, #7289, #28403, #28576, #15610, #17669, #4717, #9661, #20054, #7114, #27880, #1998, #15109, #7961, #31463, #18836, #8448, #29229, #5883, #2839, #3170, #29065, #6048, #21390, #2687, #10853, #16280, #23951, #13562, #8287, #26668, #21552, #3330, #28897, #612, #21225, #122, #31944, #453, #13715, #24115, #13226, #8615, #13386, #31299, #16106, #10680, #5553, #19011, #782, #18344, #11176, #15946, #18514, #8131, #29400, #31621, #23623, #11010, #26500, #18675, #16440, #5396, #5718, #26343, #31783, #13065, #23455, #21062, #10523, #20903, #23783, #28737, #15779, #26172, #286, #3006, #9458, #26836, #3664, #19513, #22395, #11511, #1452, #30242, #21891, #6394, #24795, #12009, #27004, #3501, #9115, #19172, #27510, #6735, #8951, #29909, #16782, #6562, #24273, #32621, #24456, #27180, #4169, #29733, #19846, #1619, #6900, #6221, #30070, #1288, #17126, #14563, #4007, #943, #32785, #13890, #21726, #24965, #9284, #11344, #32116, #32287, #8779, #16610, #14058, #29568, #1118, #19677, #3836, #22233, #19339, #14228, #24626, #11681, #11845, #22065, #32448, #16946, #27341, #14403, #17631, #9620, #28195, #30418, #12350, #22745, #23248, #25634, #33137, #14730, #22573, #1960, #30581, #12686, #4346, #9800, #28018, #20015, #25120, #30926, #9972, #33641, #7244, #4683, #14903, #2138, #15069, #12523, #5022, #23081, #25294, #33473, #20523, #25463, #10142, #7077, #15412, #20360, #1782, #10321, #17292, #27842, #30754, #12856, #20183, #2301, #20695, #22911, #33305, #15243, #2473, #17459, #27681, #7413, #4512, #17975, #7592, #17797, #4853, #28366, #25809, #12183, #31094, #32958, #8091, #18801, #10647, #743, #16240, #11144, #20861, #10972, #15905, #21348, #31745, #18637, #5187, #26629, #21519, #2643, #8415, #13518, #29193, #7753, #16073, #5844, #3293, #21187, #31584, #15572, #13677, #25970, #18141, #410, #24075, #28539, #26463, #31260, #18304, #13351, #13028, #8249, #23419, #83, #10483, #26140, #7923, #254, #28696, #5354, #15744, #2807, #29027, #13189, #23588, #10812, #21023, #31423, #18477, #28860, #5516, #26303, #2974, #23745, #5684, #3131, #577, #23913, #31906, #32081, #32407, #1410, #29867, #14019, #8743, #1243, #32242, #9073, #11472, #32578, #19640, #8579, #16400, #11970, #9247, #29692, #6182, #3458, #22190, #16573, #8908, #24919, #30030, #11641, #26794, #14518, #18969, #19133, #24583, #27470, #26964, #6527, #1578, #3625, #21850, #16907, #17083, #29526, #29365, #14190, #24240, #6695, #11800, #24417, #22025, #19302, #19468, #6011, #3962, #1082, #6349, #4126, #16740, #13854, #906, #11305, #21689, #27140, #3801, #27303, #14362, #24756 ),
 ( #30200, #7033, #30717, #17417, #10106, #17246, #20141, #28325, #22699, #14690, #33262, #1740, #27802, #4469, #4984, #7377, #14858, #19809, #27634, #25254, #1920, #17756, #9414, #12305, #33089, #25082, #6857, #2260, #15029, #15370, #9757, #30537, #19970, #7201, #12641, #23037, #22534, #17938, #17587, #4302, #2093, #30372, #27978, #7552, #25594, #12139, #28153, #4645, #25421, #12480, #25763, #22870, #9575, #9928, #20313, #4810, #2435, #32919, #15202, #33434, #20483, #30887, #22355, #32744, #8213, #16035, #23543, #5647, #15537, #211, #26425, #25928, #541, #15868, #31056, #29149, #12816, #23383, #5480, #8378, #31220, #21147, #16195, #7884, #26104, #10770, #31705, #12990, #23208, #28823, #5148, #13476, #3088, #28654, #26263, #2772, #2932, #10283, #18600, #10444, #13152, #23869, #15703, #5797, #21310, #26585, #2603, #10934, #20984, #18766, #33604, #23706, #20661, #7713, #18099, #28495, #48, #28987, #20816, #18264, #5314, #10609, #31379, #8051, #18435, #13313, #366, #31544, #32369, #19423, #19092, #11102, #21645, #11592, #32039, #24713, #31866, #1040, #9210, #3585, #29321, #14146, #16357, #8701, #29480, #19600, #21982, #6135, #699, #8530, #16529, #26927, #9033, #24033, #13977, #24374, #5969, #21482, #16868, #29655, #29992, #11431, #21808, #867, #32200, #27261, #3916, #3414, #32534, #8861, #18925, #16697, #11261, #19262, #22144, #6489, #26752, #29828, #6303, #27099, #3761, #6649, #24541, #24204, #1195, #14313, #1369, #17036, #13811, #11758, #3250, #13639, #15160, #33220, #1701, #22829, #30673, #6817, #22489, #32877, #33394, #2050, #9537, #24873, #32703, #12097, #6992, #9885, #14476, #19926, #4427, #30161, #1537, #7339, #20102, #10067, #17379, #14815, #25048, #25210, #17717, #28105, #27588, #22996, #1877, #22317, #7158, #30324, #27763, #12600, #4766, #9370, #20268, #12263, #22655, #33041, #20443, #9712, #14652, #27935, #17544, #30496, #30842, #17204, #4606, #14990, #25379, #25553, #2217, #12438, #7506, #27430, #4087, #11934, #4258, #19764, #20945, #2390, #499, #17891, #28450, #10566, #13431, #2559, #26217, #21270, #12943, #31170, #15826, #3046, #18055, #28285, #167, #10235, #18557, #31506, #6, #31337, #7841, #8007, #15325, #23664, #15499, #18226, #28942, #20774, #10894, #26386, #31665, #31017, #21105, #26064, #8174, #5602, #28784, #25718, #23826, #4940, #12778, #15994, #323, #23168, #33559, #20618, #7673, #5108, #25890, #23341, #10402, #10724, #28617, #13272, #5269, #15662, #2734, #13109, #2886, #23500, #18390, #5440, #6088, #14269, #8659, #657, #19218, #26542, #22107, #8994, #16486, #16320, #13600, #32328, #26711, #19050, #1332, #8490, #29616, #11550, #26884, #24670, #13934, #6264, #3541, #8333, #11059, #24323, #992, #31992, #16654, #21440, #11391, #19382, #21768, #29439, #5927, #27052, #32157, #11720, #18882, #3373, #6444, #29779, #3714, #23994, #31824, #16826, #29275, #13767, #24498, #14103, #1158, #21936, #24161, #8817, #27221, #18725, #3877, #29109, #5758, #16151, #3213, #826, #11217, #21599, #25816, #30934, #17163, #15248, #22441, #19557, #2479, #33647, #4050, #10327, #32493, #12691, #15418, #12861, #28201, #4860, #16990, #7598, #6606, #9162, #25641, #5029, #27384, #33478, #32662, #9327, #17803, #14440, #2307, #29950, #11891, #24833, #32833, #19719, #20366, #4213, #1497, #30116, #1659, #28371, #25007, #6778, #20528, #23089, #22278, #27549, #14611, #12053, #9498, #17980, #30759, #23253, #7418, #10147, #19752, #26917, #27250, #8850, #4244, #19413, #3575, #22134, #16686, #1185, #27578, #11923, #13964, #14466, #11581, #17193, #1690, #24359, #22308, #24863, #30149, #1027, #29471, #21798, #6807, #19250, #11421, #14642, #1526, #21971, #4078, #32689, #24530, #16518, #27083, #17024, #3747, #25038, #32191, #6475, #12084, #9024, #29645, #19587, #6292, #14135, #32359, #22474, #27418, #29815, #6122, #16857, #3905, #14301, #9357, #24702, #1359, #11747, #32524, #9198, #8690, #29981, #19082, #6639, #9874, #19914, #10221, #17369, #17704, #33030, #28437, #20257, #27754, #12589, #7149, #25366, #18044, #2378, #4418, #4927, #2038, #14979, #27921, #15489, #7328, #20092, #33382, #22983, #15146, #25880, #1864, #28092, #12426, #4755, #20603, #15314, #17534, #28273, #12767, #30661, #25706, #12253, #31006, #2207, #14804, #2546, #32865, #9699, #25541, #5094, #4593, #7493, #12930, #22820, #33210, #30826, #9527, #30486, #30314, #10056, #25196, #33545, #23158, #20433, #17877, #7661, #6981, #22641, #29098, #20936, #23655, #645, #26206, #16309, #31811, #26698, #2721, #26531, #31496, #3202, #13590, #486, #20762, #31159, #23984, #7827, #23325, #15982, #11043, #7589, #31652, #13097, #154, #28928, #18215, #13419, #3361, #10389, #21425, #7994, #28606, #15812, #23488, #8476, #5257, #10557, #23815, #31328, #15651, #26374, #2874, #26050, #18865, #29263, #5914, #18380, #28772, #18545, #13259, #3034, #5428, #5746, #16138, #314, #10884, #10713, #21258, #21094, #8164, #8319, #5588, #18713, #27036, #14427, #1483, #13752, #31977, #27536, #24819, #11538, #21755, #19038, #4037, #32144, #24483, #6765, #13921, #1320, #16974, #32316, #19705, #19369, #11708, #21921, #24147, #6076, #29764, #8982, #3699, #24655, #16472, #6429, #11878, #16811, #1145, #11376, #22093, #14089, #17150, #24307, #8806, #22263, #32650, #32479, #29427, #26871, #9312, #3528, #19204, #29937, #19544, #6591, #27370, #977, #14256, #27206, #813, #9147, #11203, #3862, #30099, #21583, #8647, #29602, #6252 ),
 ( #16639, #7106, #30961, #12721, #7621, #17324, #7445, #12380, #17825, #28227, #15100, #1646, #23114, #18005, #32817, #4885, #10008, #25665, #22426, #24995, #27714, #15272, #4375, #19873, #10174, #20391, #17486, #33336, #30784, #20047, #12039, #22597, #12549, #32986, #2333, #9483, #1990, #20555, #4547, #30269, #25495, #14757, #9652, #30446, #4199, #22940, #27872, #6932, #25150, #14936, #25324, #33502, #1816, #22777, #33169, #12211, #9833, #14598, #30614, #20213, #7280, #17661, #28049, #4710, #2166, #13218, #28568, #23944, #5388, #23282, #8124, #2678, #20895, #13552, #31614, #33676, #444, #31292, #10515, #23448, #11002, #2833, #15603, #28891, #18507, #10675, #21382, #31121, #23616, #7953, #280, #16100, #10846, #13058, #23777, #8281, #15773, #21219, #7784, #26494, #31456, #12887, #31776, #28396, #5217, #21054, #606, #113, #3000, #8442, #18336, #28729, #26334, #5054, #26007, #15445, #5546, #20722, #29059, #18668, #26166, #15938, #13380, #5711, #3163, #25841, #18175, #2503, #10350, #8773, #29725, #21547, #11505, #29903, #16602, #29560, #16432, #16776, #19163, #11839, #19004, #3493, #16939, #19505, #6387, #24107, #31937, #9108, #775, #13884, #1280, #24619, #11674, #22057, #29394, #19334, #21883, #22225, #3829, #18829, #26997, #32441, #27174, #14221, #24448, #6556, #4001, #27335, #11336, #14397, #3658, #16274, #24788, #32614, #11171, #29223, #5876, #1444, #26660, #3323, #32278, #8944, #13708, #8608, #6041, #26829, #24267, #937, #21720, #32110, #6214, #14052, #1112, #4160, #33127, #23073, #30063, #7407, #27672, #17120, #1775, #32778, #20352, #6729, #9451, #9793, #19840, #27503, #1954, #22567, #2294, #4846, #30748, #12515, #33298, #30236, #4505, #32952, #22739, #14557, #15062, #25457, #25626, #20176, #22904, #7236, #25114, #6893, #12343, #9613, #30574, #20009, #9964, #17790, #9278, #24956, #19671, #28189, #7070, #17284, #1613, #15237, #4339, #30410, #12678, #14723, #17624, #12003, #27835, #22389, #14896, #28011, #12176, #17452, #25288, #4677, #2132, #18133, #8085, #3123, #28532, #13023, #31416, #18631, #33636, #33466, #15738, #25803, #403, #13346, #15566, #26135, #23414, #2802, #30921, #5511, #31089, #78, #10806, #2638, #26457, #8243, #13512, #12849, #2968, #7917, #23737, #21181, #10640, #7585, #29021, #10136, #28361, #31578, #15900, #5678, #17970, #20518, #23242, #16068, #10315, #15405, #5015, #26296, #10478, #28855, #2467, #25964, #20690, #5181, #18471, #20854, #7748, #31253, #18297, #28689, #5348, #13184, #21016, #23581, #249, #29358, #29863, #32234, #6005, #21342, #29185, #8574, #3452, #19295, #10966, #18964, #898, #26623, #31738, #3797, #16566, #6522, #13848, #11298, #8410, #1235, #18796, #8735, #24068, #19463, #21684, #5838, #3618, #31900, #16394, #9067, #27134, #16233, #29687, #26786, #24235, #32076, #16901, #19127, #11139, #24411, #14013, #6174, #27299, #3286, #29518, #26959, #1077, #11636, #6341, #11464, #16733, #14184, #21843, #24578, #13671, #22019, #8900, #738, #32402, #3955, #21514, #23907, #571, #14686, #25414, #17240, #7372, #22864, #17751, #27465, #17580, #22529, #27973, #4640, #25249, #11792, #33255, #28145, #9243, #15025, #20135, #2087, #32573, #1405, #4120, #12473, #14512, #30026, #20306, #30530, #27628, #9751, #7195, #30196, #22185, #32739, #22692, #9409, #9921, #19633, #12134, #30710, #25078, #6689, #1915, #24913, #19805, #6852, #14356, #33081, #4297, #17078, #1574, #1734, #32915, #24750, #11966, #9571, #19964, #22350, #30366, #7028, #17412, #27798, #4463, #14852, #12300, #15863, #23031, #23378, #4978, #362, #15531, #33428, #18259, #12810, #31050, #23700, #8042, #10101, #10605, #7708, #20655, #33595, #21140, #12984, #25755, #5305, #28648, #20810, #31540, #7547, #42, #18093, #10438, #26256, #20979, #23201, #205, #18429, #25923, #31374, #17933, #2925, #7877, #20478, #8208, #4804, #15364, #31213, #10762, #10277, #13145, #18594, #28489, #5143, #2767, #15197, #2427, #25589, #15697, #30880, #5475, #28819, #2595, #26099, #23538, #13308, #2253, #12634, #28320, #32363, #13633, #8525, #26922, #14141, #29144, #28980, #11255, #21304, #29650, #8855, #11095, #21638, #18917, #32033, #26420, #1034, #26580, #29315, #6297, #31860, #21977, #3754, #9028, #8370, #32195, #3408, #19255, #16692, #6127, #3083, #24536, #5640, #23863, #27090, #11426, #1190, #13470, #16030, #18760, #11587, #5792, #10929, #535, #21803, #5964, #24365, #31699, #21476, #16188, #24028, #3580, #693, #3245, #16352, #26746, #13805, #24198, #861, #16524, #8696, #19087, #29475, #13971, #28234, #24867, #16862, #24707, #4082, #32695, #15277, #6481, #14471, #30154, #22139, #27255, #33506, #12554, #2507, #9363, #6812, #3910, #30966, #14307, #4249, #19593, #15452, #17199, #1364, #33342, #27424, #11929, #5058, #23119, #11752, #25671, #22312, #1529, #19758, #12891, #27583, #6644, #20396, #10015, #1696, #23287, #32527, #14647, #25043, #22947, #7626, #2339, #30789, #12729, #10179, #7450, #20562, #9204, #18009, #17832, #29986, #33680, #19418, #17030, #4890, #28400, #25846, #29819, #31125, #5393, #21060, #13062, #18180, #23948, #3003, #26665, #23620, #31461, #7788, #21385, #28573, #28894, #10519, #5881, #8128, #5222, #23780, #18341, #2836, #29226, #13559, #15607, #16103, #13222, #26170, #15777, #3327, #18510, #31296, #10850, #450, #26339, #13712, #23452, #5549, #284, #15942, #31780, #26497, #28734, #5715, #609, #13383, #3167, #119, #8445, #21222, #26012, #24111, #10354 ) ),
 .UNSPECIFIED., .T., .F., .T. ) 
 B_SPLINE_SURFACE_WITH_KNOTS ( ( 4, 3, 4 ),
 ( 3, 2, 2, 2, 2, 2, 2, 2, 2, 2, 2, 2, 2, 2, 2, 2, 2, 2, 2, 2, 2, 2, 2, 2, 2, 2, 2, 2, 2, 2, 2, 2, 2, 2, 2, 2, 2, 2, 2, 2, 2, 2, 2, 2, 2, 2, 2, 2, 2, 2, 2, 2, 2, 2, 2, 2, 2, 2, 2, 2, 2, 2, 2, 2, 2, 2, 2, 2, 2, 2, 2, 2, 2, 2, 2, 2, 2, 2, 2, 2, 2, 2, 2, 2, 2, 2, 2, 2, 2, 2, 2, 2, 2, 2, 2, 2, 2, 2, 2, 2, 2, 2, 2, 2, 2, 2, 2, 2, 2, 2, 2, 2, 2, 2, 2, 2, 2, 2, 2, 2, 2, 2, 2, 2, 2, 2, 2, 2, 2, 2, 2, 2, 2, 2, 2, 2, 2, 2, 2, 2, 2, 2, 2, 2, 2, 2, 2, 2, 2, 2, 2, 2, 2, 2, 2, 2, 2, 2, 2, 2, 2, 2, 2, 2, 2, 2, 2, 2, 2, 2, 2, 2, 2, 2, 2, 2, 2, 2, 2, 2, 2, 2, 2, 2, 2, 2, 2, 2, 2, 2, 2, 2, 2, 2, 2, 2, 2, 2, 2, 2, 2, 2, 2, 2, 2, 2, 2, 2, 2, 2, 2, 2, 2, 2, 2, 2, 2, 2, 2, 2, 2, 2, 2, 2, 2, 2, 2, 2, 2, 2, 2, 2, 2, 2, 2, 2, 2, 2, 2, 2, 2, 2, 2, 2, 2, 2, 2, 2, 2, 2, 2, 2, 2, 2, 2, 2, 2, 2, 2, 2, 2, 2, 2, 2, 2, 2, 2, 2, 2, 2, 2, 2, 2, 2, 2, 2, 2, 2, 2, 2, 2, 2, 2, 2, 2, 2, 2, 2, 2, 2, 2, 2, 2, 2, 2, 2, 2, 2, 2, 2, 2, 2, 2, 2, 2, 2, 2, 2, 2, 2, 2, 2, 2, 2, 2, 2, 2, 2, 2, 2, 2, 2, 2, 2, 2, 2, 2, 2, 2, 2, 2, 2, 2, 2, 2, 2, 2, 2, 2, 2, 2, 2, 2, 2, 2, 2, 3 ),
 ( 0.000000000000000000, 0.5000000000000000000, 1.000000000000000000 ),
 ( 0.000000000000000000, 0.002857142857142857140, 0.005714285714285714281, 0.008571428571428571855, 0.01142857142857142856, 0.01428571428571428527, 0.01714285714285714371, 0.02000000000000000042, 0.02285714285714285712, 0.02571428571428571383, 0.02857142857142857054, 0.03142857142857143071, 0.03428571428571428742, 0.03714285714285714413, 0.04000000000000000083, 0.04285714285714285754, 0.04571428571428571425, 0.04857142857142857095, 0.05142857142857142766, 0.05428571428571428437, 0.05714285714285714107, 0.05999999999999999778, 0.06285714285714286143, 0.06571428571428571119, 0.06857142857142857484, 0.07142857142857142461, 0.07428571428571428825, 0.07714285714285713802, 0.08000000000000000167, 0.08285714285714285143, 0.08571428571428571508, 0.08857142857142856485, 0.09142857142857142849, 0.09428571428571429214, 0.09714285714285714191, 0.1000000000000000056, 0.1028571428571428553, 0.1057142857142857190, 0.1085714285714285687, 0.1114285714285714324, 0.1142857142857142821, 0.1171428571428571458, 0.1199999999999999956, 0.1228571428571428592, 0.1257142857142857229, 0.1285714285714285587, 0.1314285714285714224, 0.1342857142857142860, 0.1371428571428571497, 0.1400000000000000133, 0.1428571428571428492, 0.1457142857142857129, 0.1485714285714285765, 0.1514285714285714401, 0.1542857142857142760, 0.1571428571428571397, 0.1600000000000000033, 0.1628571428571428670, 0.1657142857142857029, 0.1685714285714285665, 0.1714285714285714302, 0.1742857142857142938, 0.1771428571428571297, 0.1799999999999999933, 0.1828571428571428570, 0.1857142857142857206, 0.1885714285714285843, 0.1914285714285714202, 0.1942857142857142838, 0.1971428571428571475, 0.2000000000000000111, 0.2028571428571428470, 0.2057142857142857106, 0.2085714285714285743, 0.2114285714285714379, 0.2142857142857142738, 0.2171428571428571375, 0.2200000000000000011, 0.2228571428571428648, 0.2257142857142857006, 0.2285714285714285643, 0.2314285714285714279, 0.2342857142857142916, 0.2371428571428571552, 0.2399999999999999911, 0.2428571428571428548, 0.2457142857142857184, 0.2485714285714285821, 0.2514285714285714457, 0.2542857142857142816, 0.2571428571428571175, 0.2600000000000000089, 0.2628571428571428448, 0.2657142857142857362, 0.2685714285714285721, 0.2714285714285714080, 0.2742857142857142994, 0.2771428571428571352, 0.2800000000000000266, 0.2828571428571428625, 0.2857142857142856984, 0.2885714285714285898, 0.2914285714285714257, 0.2942857142857142616, 0.2971428571428571530, 0.2999999999999999889, 0.3028571428571428803, 0.3057142857142857162, 0.3085714285714285521, 0.3114285714285714435, 0.3142857142857142794, 0.3171428571428571153, 0.3200000000000000067, 0.3228571428571428426, 0.3257142857142857340, 0.3285714285714285698, 0.3314285714285714057, 0.3342857142857142971, 0.3371428571428571330, 0.3400000000000000244, 0.3428571428571428603, 0.3457142857142856962, 0.3485714285714285876, 0.3514285714285714235, 0.3542857142857142594, 0.3571428571428571508, 0.3599999999999999867, 0.3628571428571428781, 0.3657142857142857140, 0.3685714285714285499, 0.3714285714285714413, 0.3742857142857142771, 0.3771428571428571686, 0.3800000000000000044, 0.3828571428571428403, 0.3857142857142857317, 0.3885714285714285676, 0.3914285714285714035, 0.3942857142857142949, 0.3971428571428571308, 0.4000000000000000222, 0.4028571428571428581, 0.4057142857142856940, 0.4085714285714285854, 0.4114285714285714213, 0.4142857142857143127, 0.4171428571428571486, 0.4199999999999999845, 0.4228571428571428759, 0.4257142857142857117, 0.4285714285714285476, 0.4314285714285714390, 0.4342857142857142749, 0.4371428571428571663, 0.4400000000000000022, 0.4428571428571428381, 0.4457142857142857295, 0.4485714285714285654, 0.4514285714285714013, 0.4542857142857142927, 0.4571428571428571286, 0.4600000000000000200, 0.4628571428571428559, 0.4657142857142856918, 0.4685714285714285832, 0.4714285714285714191, 0.4742857142857143105, 0.4771428571428571463, 0.4799999999999999822, 0.4828571428571428736, 0.4857142857142857095, 0.4885714285714285454, 0.4914285714285714368, 0.4942857142857142727, 0.4971428571428571641, 0.5000000000000000000, 0.5028571428571428914, 0.5057142857142856718, 0.5085714285714285632, 0.5114285714285714546, 0.5142857142857142350, 0.5171428571428571264, 0.5200000000000000178, 0.5228571428571429092, 0.5257142857142856895, 0.5285714285714285809, 0.5314285714285714723, 0.5342857142857142527, 0.5371428571428571441, 0.5400000000000000355, 0.5428571428571428159, 0.5457142857142857073, 0.5485714285714285987, 0.5514285714285713791, 0.5542857142857142705, 0.5571428571428571619, 0.5600000000000000533, 0.5628571428571428337, 0.5657142857142857251, 0.5685714285714286165, 0.5714285714285713969, 0.5742857142857142883, 0.5771428571428571797, 0.5799999999999999600, 0.5828571428571428514, 0.5857142857142857428, 0.5885714285714285232, 0.5914285714285714146, 0.5942857142857143060, 0.5971428571428571974, 0.5999999999999999778, 0.6028571428571428692, 0.6057142857142857606, 0.6085714285714285410, 0.6114285714285714324, 0.6142857142857143238, 0.6171428571428571042, 0.6199999999999999956, 0.6228571428571428870, 0.6257142857142856673, 0.6285714285714285587, 0.6314285714285714501, 0.6342857142857142305, 0.6371428571428571219, 0.6400000000000000133, 0.6428571428571429047, 0.6457142857142856851, 0.6485714285714285765, 0.6514285714285714679, 0.6542857142857142483, 0.6571428571428571397, 0.6600000000000000311, 0.6628571428571428115, 0.6657142857142857029, 0.6685714285714285943, 0.6714285714285713746, 0.6742857142857142660, 0.6771428571428571574, 0.6800000000000000488, 0.6828571428571428292, 0.6857142857142857206, 0.6885714285714286120, 0.6914285714285713924, 0.6942857142857142838, 0.6971428571428571752, 0.6999999999999999556, 0.7028571428571428470, 0.7057142857142857384, 0.7085714285714285188, 0.7114285714285714102, 0.7142857142857143016, 0.7171428571428571930, 0.7199999999999999734, 0.7228571428571428648, 0.7257142857142857562, 0.7285714285714285365, 0.7314285714285714279, 0.7342857142857143193, 0.7371428571428570997, 0.7399999999999999911, 0.7428571428571428825, 0.7457142857142856629, 0.7485714285714285543, 0.7514285714285714457, 0.7542857142857143371, 0.7571428571428571175, 0.7600000000000000089, 0.7628571428571429003, 0.7657142857142856807, 0.7685714285714285721, 0.7714285714285714635, 0.7742857142857142438, 0.7771428571428571352, 0.7800000000000000266, 0.7828571428571428070, 0.7857142857142856984, 0.7885714285714285898, 0.7914285714285714812, 0.7942857142857142616, 0.7971428571428571530, 0.8000000000000000444, 0.8028571428571428248, 0.8057142857142857162, 0.8085714285714286076, 0.8114285714285713880, 0.8142857142857142794, 0.8171428571428571708, 0.8199999999999999512, 0.8228571428571428426, 0.8257142857142857340, 0.8285714285714286254, 0.8314285714285714057, 0.8342857142857142971, 0.8371428571428571885, 0.8399999999999999689, 0.8428571428571428603, 0.8457142857142857517, 0.8485714285714285321, 0.8514285714285714235, 0.8542857142857143149, 0.8571428571428570953, 0.8599999999999999867, 0.8628571428571428781, 0.8657142857142857695, 0.8685714285714285499, 0.8714285714285714413, 0.8742857142857143327, 0.8771428571428571130, 0.8800000000000000044, 0.8828571428571428958, 0.8857142857142856762, 0.8885714285714285676, 0.8914285714285714590, 0.8942857142857142394, 0.8971428571428571308, 0.9000000000000000222, 0.9028571428571428026, 0.9057142857142856940, 0.9085714285714285854, 0.9114285714285714768, 0.9142857142857142572, 0.9171428571428571486, 0.9200000000000000400, 0.9228571428571428203, 0.9257142857142857117, 0.9285714285714286031, 0.9314285714285713835, 0.9342857142857142749, 0.9371428571428571663, 0.9399999999999999467, 0.9428571428571428381, 0.9457142857142857295, 0.9485714285714286209, 0.9514285714285714013, 0.9542857142857142927, 0.9571428571428571841, 0.9599999999999999645, 0.9628571428571428559, 0.9657142857142857473, 0.9685714285714285277, 0.9714285714285714191, 0.9742857142857143105, 0.9771428571428570908, 0.9799999999999999822, 0.9828571428571428736, 0.9857142857142857650, 0.9955714285714286627 ),
 .UNSPECIFIED. ) 
 GEOMETRIC_REPRESENTATION_ITEM ( )  RATIONAL_B_SPLINE_SURFACE ( (
 ( 1.000000000000000000, 0.9510565162951535312, 1.000000000000000000, 0.9510565162951535312, 1.000000000000000000, 0.9510565162951535312, 1.000000000000000000, 0.9510565162951535312, 1.000000000000000000, 0.9510565162951535312, 1.000000000000000000, 0.9510565162951535312, 1.000000000000000000, 0.9510565162951535312, 1.000000000000000000, 0.9510565162951535312, 1.000000000000000000, 0.9510565162951535312, 1.000000000000000000, 0.9510565162951535312, 1.000000000000000000, 0.9510565162951535312, 1.000000000000000000, 0.9510565162951535312, 1.000000000000000000, 0.9510565162951535312, 1.000000000000000000, 0.9510565162951535312, 1.000000000000000000, 0.9510565162951535312, 1.000000000000000000, 0.9510565162951535312, 1.000000000000000000, 0.9510565162951535312, 1.000000000000000000, 0.9510565162951535312, 1.000000000000000000, 0.9510565162951535312, 1.000000000000000000, 0.9510565162951535312, 1.000000000000000000, 0.9510565162951535312, 1.000000000000000000, 0.9510565162951535312, 1.000000000000000000, 0.9510565162951535312, 1.000000000000000000, 0.9510565162951535312, 1.000000000000000000, 0.9510565162951535312, 1.000000000000000000, 0.9510565162951535312, 1.000000000000000000, 0.9510565162951535312, 1.000000000000000000, 0.9510565162951535312, 1.000000000000000000, 0.9510565162951535312, 1.000000000000000000, 0.9510565162951535312, 1.000000000000000000, 0.9510565162951535312, 1.000000000000000000, 0.9510565162951535312, 1.000000000000000000, 0.9510565162951535312, 1.000000000000000000, 0.9510565162951535312, 1.000000000000000000, 0.9510565162951535312, 1.000000000000000000, 0.9510565162951535312, 1.000000000000000000, 0.9510565162951535312, 1.000000000000000000, 0.9510565162951535312, 1.000000000000000000, 0.9510565162951535312, 1.000000000000000000, 0.9510565162951535312, 1.000000000000000000, 0.9510565162951535312, 1.000000000000000000, 0.9510565162951535312, 1.000000000000000000, 0.9510565162951535312, 1.000000000000000000, 0.9510565162951535312, 1.000000000000000000, 0.9510565162951535312, 1.000000000000000000, 0.9510565162951535312, 1.000000000000000000, 0.9510565162951535312, 1.000000000000000000, 0.9510565162951535312, 1.000000000000000000, 0.9510565162951535312, 1.000000000000000000, 0.9510565162951535312, 1.000000000000000000, 0.9510565162951535312, 1.000000000000000000, 0.9510565162951535312, 1.000000000000000000, 0.9510565162951535312, 1.000000000000000000, 0.9510565162951535312, 1.000000000000000000, 0.9510565162951535312, 1.000000000000000000, 0.9510565162951535312, 1.000000000000000000, 0.9510565162951535312, 1.000000000000000000, 0.9510565162951535312, 1.000000000000000000, 0.9510565162951535312, 1.000000000000000000, 0.9510565162951535312, 1.000000000000000000, 0.9510565162951535312, 1.000000000000000000, 0.9510565162951535312, 1.000000000000000000, 0.9510565162951535312, 1.000000000000000000, 0.9510565162951535312, 1.000000000000000000, 0.9510565162951535312, 1.000000000000000000, 0.9510565162951535312, 1.000000000000000000, 0.9510565162951535312, 1.000000000000000000, 0.9510565162951535312, 1.000000000000000000, 0.9510565162951535312, 1.000000000000000000, 0.9510565162951535312, 1.000000000000000000, 0.9510565162951535312, 1.000000000000000000, 0.9510565162951535312, 1.000000000000000000, 0.9510565162951535312, 1.000000000000000000, 0.9510565162951535312, 1.000000000000000000, 0.9510565162951535312, 1.000000000000000000, 0.9510565162951535312, 1.000000000000000000, 0.9510565162951535312, 1.000000000000000000, 0.9510565162951535312, 1.000000000000000000, 0.9510565162951535312, 1.000000000000000000, 0.9510565162951535312, 1.000000000000000000, 0.9510565162951535312, 1.000000000000000000, 0.9510565162951535312, 1.000000000000000000, 0.9510565162951535312, 1.000000000000000000, 0.9510565162951535312, 1.000000000000000000, 0.9510565162951535312, 1.000000000000000000, 0.9510565162951535312, 1.000000000000000000, 0.9510565162951535312, 1.000000000000000000, 0.9510565162951535312, 1.000000000000000000, 0.9510565162951535312, 1.000000000000000000, 0.9510565162951535312, 1.000000000000000000, 0.9510565162951535312, 1.000000000000000000, 0.9510565162951535312, 1.000000000000000000, 0.9510565162951535312, 1.000000000000000000, 0.9510565162951535312, 1.000000000000000000, 0.9510565162951535312, 1.000000000000000000, 0.9510565162951535312, 1.000000000000000000, 0.9510565162951535312, 1.000000000000000000, 0.9510565162951535312, 1.000000000000000000, 0.9510565162951535312, 1.000000000000000000, 0.9510565162951535312, 1.000000000000000000, 0.9510565162951535312, 1.000000000000000000, 0.9510565162951535312, 1.000000000000000000, 0.9510565162951535312, 1.000000000000000000, 0.9510565162951535312, 1.000000000000000000, 0.9510565162951535312, 1.000000000000000000, 0.9510565162951535312, 1.000000000000000000, 0.9510565162951535312, 1.000000000000000000, 0.9510565162951535312, 1.000000000000000000, 0.9510565162951535312, 1.000000000000000000, 0.9510565162951535312, 1.000000000000000000, 0.9510565162951535312, 1.000000000000000000, 0.9510565162951535312, 1.000000000000000000, 0.9510565162951535312, 1.000000000000000000, 0.9510565162951535312, 1.000000000000000000, 0.9510565162951535312, 1.000000000000000000, 0.9510565162951535312, 1.000000000000000000, 0.9510565162951535312, 1.000000000000000000, 0.9510565162951535312, 1.000000000000000000, 0.9510565162951535312, 1.000000000000000000, 0.9510565162951535312, 1.000000000000000000, 0.9510565162951535312, 1.000000000000000000, 0.9510565162951535312, 1.000000000000000000, 0.9510565162951535312, 1.000000000000000000, 0.9510565162951535312, 1.000000000000000000, 0.9510565162951535312, 1.000000000000000000, 0.9510565162951535312, 1.000000000000000000, 0.9510565162951535312, 1.000000000000000000, 0.9510565162951535312, 1.000000000000000000, 0.9510565162951535312, 1.000000000000000000, 0.9510565162951535312, 1.000000000000000000, 0.9510565162951535312, 1.000000000000000000, 0.9510565162951535312, 1.000000000000000000, 0.9510565162951535312, 1.000000000000000000, 0.9510565162951535312, 1.000000000000000000, 0.9510565162951535312, 1.000000000000000000, 0.9510565162951535312, 1.000000000000000000, 0.9510565162951535312, 1.000000000000000000, 0.9510565162951535312, 1.000000000000000000, 0.9510565162951535312, 1.000000000000000000, 0.9510565162951535312, 1.000000000000000000, 0.9510565162951535312, 1.000000000000000000, 0.9510565162951535312, 1.000000000000000000, 0.9510565162951535312, 1.000000000000000000, 0.9510565162951535312, 1.000000000000000000, 0.9510565162951535312, 1.000000000000000000, 0.9510565162951535312, 1.000000000000000000, 0.9510565162951535312, 1.000000000000000000, 0.9510565162951535312, 1.000000000000000000, 0.9510565162951535312, 1.000000000000000000, 0.9510565162951535312, 1.000000000000000000, 0.9510565162951535312, 1.000000000000000000, 0.9510565162951535312, 1.000000000000000000, 0.9510565162951535312, 1.000000000000000000, 0.9510565162951535312, 1.000000000000000000, 0.9510565162951535312, 1.000000000000000000, 0.9510565162951535312, 1.000000000000000000, 0.9510565162951535312, 1.000000000000000000, 0.9510565162951535312, 1.000000000000000000, 0.9510565162951535312, 1.000000000000000000, 0.9510565162951535312, 1.000000000000000000, 0.9510565162951535312, 1.000000000000000000, 0.9510565162951535312, 1.000000000000000000, 0.9510565162951535312, 1.000000000000000000, 0.9510565162951535312, 1.000000000000000000, 0.9510565162951535312, 1.000000000000000000, 0.9510565162951535312, 1.000000000000000000, 0.9510565162951535312, 1.000000000000000000, 0.9510565162951535312, 1.000000000000000000, 0.9510565162951535312, 1.000000000000000000, 0.9510565162951535312, 1.000000000000000000, 0.9510565162951535312, 1.000000000000000000, 0.9510565162951535312, 1.000000000000000000, 0.9510565162951535312, 1.000000000000000000, 0.9510565162951535312, 1.000000000000000000, 0.9510565162951535312, 1.000000000000000000, 0.9510565162951535312, 1.000000000000000000, 0.9510565162951535312, 1.000000000000000000, 0.9510565162951535312, 1.000000000000000000, 0.9510565162951535312, 1.000000000000000000, 0.9510565162951535312, 1.000000000000000000, 0.9510565162951535312, 1.000000000000000000, 0.9510565162951535312, 1.000000000000000000, 0.9510565162951535312, 1.000000000000000000, 0.9510565162951535312, 1.000000000000000000, 0.9510565162951535312, 1.000000000000000000, 0.9510565162951535312, 1.000000000000000000, 0.9510565162951535312, 1.000000000000000000, 0.9510565162951535312, 1.000000000000000000, 0.9510565162951535312, 1.000000000000000000, 0.9510565162951535312, 1.000000000000000000, 0.9510565162951535312, 1.000000000000000000, 0.9510565162951535312, 1.000000000000000000, 0.9510565162951535312, 1.000000000000000000, 0.9510565162951535312, 1.000000000000000000, 0.9510565162951535312, 1.000000000000000000, 0.9510565162951535312, 1.000000000000000000, 0.9510565162951535312, 1.000000000000000000, 0.9510565162951535312, 1.000000000000000000, 0.9510565162951535312, 1.000000000000000000, 0.9510565162951535312, 1.000000000000000000, 0.9510565162951535312, 1.000000000000000000, 0.9510565162951535312, 1.000000000000000000, 0.9510565162951535312, 1.000000000000000000, 0.9510565162951535312, 1.000000000000000000, 0.9510565162951535312, 1.000000000000000000, 0.9510565162951535312, 1.000000000000000000, 0.9510565162951535312, 1.000000000000000000, 0.9510565162951535312, 1.000000000000000000, 0.9510565162951535312, 1.000000000000000000, 0.9510565162951535312, 1.000000000000000000, 0.9510565162951535312, 1.000000000000000000, 0.9510565162951535312, 1.000000000000000000, 0.9510565162951535312, 1.000000000000000000, 0.9510565162951535312, 1.000000000000000000, 0.9510565162951535312, 1.000000000000000000, 0.9510565162951535312, 1.000000000000000000, 0.9510565162951535312, 1.000000000000000000, 0.9510565162951535312, 1.000000000000000000, 0.9510565162951535312, 1.000000000000000000, 0.9510565162951535312, 1.000000000000000000, 0.9510565162951535312, 1.000000000000000000, 0.9510565162951535312, 1.000000000000000000, 0.9510565162951535312, 1.000000000000000000, 0.9510565162951535312, 1.000000000000000000, 0.9510565162951535312, 1.000000000000000000, 0.9510565162951535312, 1.000000000000000000, 0.9510565162951535312, 1.000000000000000000, 0.9510565162951535312, 1.000000000000000000, 0.9510565162951535312, 1.000000000000000000, 0.9510565162951535312, 1.000000000000000000, 0.9510565162951535312, 1.000000000000000000, 0.9510565162951535312, 1.000000000000000000, 0.9510565162951535312, 1.000000000000000000, 0.9510565162951535312, 1.000000000000000000, 0.9510565162951535312, 1.000000000000000000, 0.9510565162951535312, 1.000000000000000000, 0.9510565162951535312, 1.000000000000000000, 0.9510565162951535312, 1.000000000000000000, 0.9510565162951535312, 1.000000000000000000, 0.9510565162951535312, 1.000000000000000000, 0.9510565162951535312, 1.000000000000000000, 0.9510565162951535312, 1.000000000000000000, 0.9510565162951535312, 1.000000000000000000, 0.9510565162951535312, 1.000000000000000000, 0.9510565162951535312, 1.000000000000000000, 0.9510565162951535312, 1.000000000000000000, 0.9510565162951535312, 1.000000000000000000, 0.9510565162951535312, 1.000000000000000000, 0.9510565162951535312, 1.000000000000000000, 0.9510565162951535312, 1.000000000000000000, 0.9510565162951535312, 1.000000000000000000, 0.9510565162951535312, 1.000000000000000000, 0.9510565162951535312, 1.000000000000000000, 0.9510565162951535312, 1.000000000000000000, 0.9510565162951535312, 1.000000000000000000, 0.9510565162951535312, 1.000000000000000000, 0.9510565162951535312, 1.000000000000000000, 0.9510565162951535312, 1.000000000000000000, 0.9510565162951535312, 1.000000000000000000, 0.9510565162951535312, 1.000000000000000000, 0.9510565162951535312, 1.000000000000000000, 0.9510565162951535312, 1.000000000000000000, 0.9510565162951535312, 1.000000000000000000, 0.9510565162951535312, 1.000000000000000000, 0.9510565162951535312, 1.000000000000000000, 0.9510565162951535312, 1.000000000000000000, 0.9510565162951535312, 1.000000000000000000, 0.9510565162951535312, 1.000000000000000000, 0.9510565162951535312, 1.000000000000000000, 0.9510565162951535312, 1.000000000000000000, 0.9510565162951535312, 1.000000000000000000, 0.9510565162951535312, 1.000000000000000000, 0.9510565162951535312, 1.000000000000000000, 0.9510565162951535312, 1.000000000000000000, 0.9510565162951535312, 1.000000000000000000, 0.9510565162951535312, 1.000000000000000000, 0.9510565162951535312, 1.000000000000000000, 0.9510565162951535312, 1.000000000000000000, 0.9510565162951535312, 1.000000000000000000, 0.9510565162951535312, 1.000000000000000000, 0.9510565162951535312, 1.000000000000000000, 0.9510565162951535312, 1.000000000000000000, 0.9510565162951535312, 1.000000000000000000, 0.9510565162951535312, 1.000000000000000000, 0.9510565162951535312, 1.000000000000000000, 0.9510565162951535312, 1.000000000000000000, 0.9510565162951535312, 1.000000000000000000, 0.9510565162951535312, 1.000000000000000000, 0.9510565162951535312, 1.000000000000000000, 0.9510565162951535312, 1.000000000000000000, 0.9510565162951535312, 1.000000000000000000, 0.9510565162951535312, 1.000000000000000000, 0.9510565162951535312, 1.000000000000000000, 0.9510565162951535312, 1.000000000000000000, 0.9510565162951535312, 1.000000000000000000, 0.9510565162951535312, 1.000000000000000000, 0.9510565162951535312, 1.000000000000000000, 0.9510565162951535312, 1.000000000000000000, 0.9510565162951535312, 1.000000000000000000, 0.9510565162951535312, 1.000000000000000000, 0.9510565162951535312, 1.000000000000000000, 0.9510565162951535312, 1.000000000000000000, 0.9510565162951535312, 1.000000000000000000, 0.9510565162951535312, 1.000000000000000000, 0.9510565162951535312, 1.000000000000000000, 0.9510565162951535312, 1.000000000000000000, 0.9510565162951535312, 1.000000000000000000, 0.9510565162951535312, 1.000000000000000000, 0.9510565162951535312, 1.000000000000000000, 0.9510565162951535312, 1.000000000000000000, 0.9510565162951535312, 1.000000000000000000, 0.9510565162951535312, 1.000000000000000000, 0.9510565162951535312, 1.000000000000000000, 0.9510565162951535312, 1.000000000000000000, 0.9510565162951535312, 1.000000000000000000, 0.9510565162951535312, 1.000000000000000000, 0.9510565162951535312, 1.000000000000000000, 0.9510565162951535312, 1.000000000000000000, 0.9510565162951535312, 1.000000000000000000, 0.9510565162951535312, 1.000000000000000000, 0.9510565162951535312, 1.000000000000000000, 0.9510565162951535312, 1.000000000000000000, 0.9510565162951535312, 1.000000000000000000, 0.9510565162951535312, 1.000000000000000000, 0.9510565162951535312, 1.000000000000000000, 0.9510565162951535312, 1.000000000000000000, 0.9510565162951535312, 1.000000000000000000, 0.9510565162951535312, 1.000000000000000000, 0.9510565162951535312, 1.000000000000000000, 0.9510565162951535312, 1.000000000000000000, 0.9510565162951535312, 1.000000000000000000, 0.9510565162951535312, 1.000000000000000000, 0.9510565162951535312, 1.000000000000000000, 0.9510565162951535312, 1.000000000000000000, 0.9510565162951535312, 1.000000000000000000, 0.9510565162951535312, 1.000000000000000000, 0.9510565162951535312, 1.000000000000000000, 0.9510565162951535312, 1.000000000000000000, 0.9510565162951535312, 1.000000000000000000, 0.9510565162951535312, 1.000000000000000000, 0.9510565162951535312, 1.000000000000000000, 0.9510565162951535312, 1.000000000000000000, 0.9510565162951535312, 1.000000000000000000, 0.9510565162951535312, 1.000000000000000000, 0.9510565162951535312, 1.000000000000000000, 1.000000000000000000, 1.000000000000000000),
 ( 0.3333333333333333703, 0.3170188387650512141, 0.3333333333333333703, 0.3170188387650512141, 0.3333333333333333703, 0.3170188387650512141, 0.3333333333333333703, 0.3170188387650512141, 0.3333333333333333703, 0.3170188387650512141, 0.3333333333333333703, 0.3170188387650512141, 0.3333333333333333703, 0.3170188387650512141, 0.3333333333333333703, 0.3170188387650512141, 0.3333333333333333703, 0.3170188387650512141, 0.3333333333333333703, 0.3170188387650512141, 0.3333333333333333703, 0.3170188387650512141, 0.3333333333333333703, 0.3170188387650512141, 0.3333333333333333703, 0.3170188387650512141, 0.3333333333333333703, 0.3170188387650512141, 0.3333333333333333703, 0.3170188387650512141, 0.3333333333333333703, 0.3170188387650512141, 0.3333333333333333703, 0.3170188387650512141, 0.3333333333333333703, 0.3170188387650512141, 0.3333333333333333703, 0.3170188387650512141, 0.3333333333333333703, 0.3170188387650512141, 0.3333333333333333703, 0.3170188387650512141, 0.3333333333333333703, 0.3170188387650512141, 0.3333333333333333703, 0.3170188387650512141, 0.3333333333333333703, 0.3170188387650512141, 0.3333333333333333703, 0.3170188387650512141, 0.3333333333333333703, 0.3170188387650512141, 0.3333333333333333703, 0.3170188387650512141, 0.3333333333333333703, 0.3170188387650512141, 0.3333333333333333703, 0.3170188387650512141, 0.3333333333333333703, 0.3170188387650512141, 0.3333333333333333703, 0.3170188387650512141, 0.3333333333333333703, 0.3170188387650512141, 0.3333333333333333703, 0.3170188387650512141, 0.3333333333333333703, 0.3170188387650512141, 0.3333333333333333703, 0.3170188387650512141, 0.3333333333333333703, 0.3170188387650512141, 0.3333333333333333703, 0.3170188387650512141, 0.3333333333333333703, 0.3170188387650512141, 0.3333333333333333703, 0.3170188387650512141, 0.3333333333333333703, 0.3170188387650512141, 0.3333333333333333703, 0.3170188387650512141, 0.3333333333333333703, 0.3170188387650512141, 0.3333333333333333703, 0.3170188387650512141, 0.3333333333333333703, 0.3170188387650512141, 0.3333333333333333703, 0.3170188387650512141, 0.3333333333333333703, 0.3170188387650512141, 0.3333333333333333703, 0.3170188387650512141, 0.3333333333333333703, 0.3170188387650512141, 0.3333333333333333703, 0.3170188387650512141, 0.3333333333333333703, 0.3170188387650512141, 0.3333333333333333703, 0.3170188387650512141, 0.3333333333333333703, 0.3170188387650512141, 0.3333333333333333703, 0.3170188387650512141, 0.3333333333333333703, 0.3170188387650512141, 0.3333333333333333703, 0.3170188387650512141, 0.3333333333333333703, 0.3170188387650512141, 0.3333333333333333703, 0.3170188387650512141, 0.3333333333333333703, 0.3170188387650512141, 0.3333333333333333703, 0.3170188387650512141, 0.3333333333333333703, 0.3170188387650512141, 0.3333333333333333703, 0.3170188387650512141, 0.3333333333333333703, 0.3170188387650512141, 0.3333333333333333703, 0.3170188387650512141, 0.3333333333333333703, 0.3170188387650512141, 0.3333333333333333703, 0.3170188387650512141, 0.3333333333333333703, 0.3170188387650512141, 0.3333333333333333703, 0.3170188387650512141, 0.3333333333333333703, 0.3170188387650512141, 0.3333333333333333703, 0.3170188387650512141, 0.3333333333333333703, 0.3170188387650512141, 0.3333333333333333703, 0.3170188387650512141, 0.3333333333333333703, 0.3170188387650512141, 0.3333333333333333703, 0.3170188387650512141, 0.3333333333333333703, 0.3170188387650512141, 0.3333333333333333703, 0.3170188387650512141, 0.3333333333333333703, 0.3170188387650512141, 0.3333333333333333703, 0.3170188387650512141, 0.3333333333333333703, 0.3170188387650512141, 0.3333333333333333703, 0.3170188387650512141, 0.3333333333333333703, 0.3170188387650512141, 0.3333333333333333703, 0.3170188387650512141, 0.3333333333333333703, 0.3170188387650512141, 0.3333333333333333703, 0.3170188387650512141, 0.3333333333333333703, 0.3170188387650512141, 0.3333333333333333703, 0.3170188387650512141, 0.3333333333333333703, 0.3170188387650512141, 0.3333333333333333703, 0.3170188387650512141, 0.3333333333333333703, 0.3170188387650512141, 0.3333333333333333703, 0.3170188387650512141, 0.3333333333333333703, 0.3170188387650512141, 0.3333333333333333703, 0.3170188387650512141, 0.3333333333333333703, 0.3170188387650512141, 0.3333333333333333703, 0.3170188387650512141, 0.3333333333333333703, 0.3170188387650512141, 0.3333333333333333703, 0.3170188387650512141, 0.3333333333333333703, 0.3170188387650512141, 0.3333333333333333703, 0.3170188387650512141, 0.3333333333333333703, 0.3170188387650512141, 0.3333333333333333703, 0.3170188387650512141, 0.3333333333333333703, 0.3170188387650512141, 0.3333333333333333703, 0.3170188387650512141, 0.3333333333333333703, 0.3170188387650512141, 0.3333333333333333703, 0.3170188387650512141, 0.3333333333333333703, 0.3170188387650512141, 0.3333333333333333703, 0.3170188387650512141, 0.3333333333333333703, 0.3170188387650512141, 0.3333333333333333703, 0.3170188387650512141, 0.3333333333333333703, 0.3170188387650512141, 0.3333333333333333703, 0.3170188387650512141, 0.3333333333333333703, 0.3170188387650512141, 0.3333333333333333703, 0.3170188387650512141, 0.3333333333333333703, 0.3170188387650512141, 0.3333333333333333703, 0.3170188387650512141, 0.3333333333333333703, 0.3170188387650512141, 0.3333333333333333703, 0.3170188387650512141, 0.3333333333333333703, 0.3170188387650512141, 0.3333333333333333703, 0.3170188387650512141, 0.3333333333333333703, 0.3170188387650512141, 0.3333333333333333703, 0.3170188387650512141, 0.3333333333333333703, 0.3170188387650512141, 0.3333333333333333703, 0.3170188387650512141, 0.3333333333333333703, 0.3170188387650512141, 0.3333333333333333703, 0.3170188387650512141, 0.3333333333333333703, 0.3170188387650512141, 0.3333333333333333703, 0.3170188387650512141, 0.3333333333333333703, 0.3170188387650512141, 0.3333333333333333703, 0.3170188387650512141, 0.3333333333333333703, 0.3170188387650512141, 0.3333333333333333703, 0.3170188387650512141, 0.3333333333333333703, 0.3170188387650512141, 0.3333333333333333703, 0.3170188387650512141, 0.3333333333333333703, 0.3170188387650512141, 0.3333333333333333703, 0.3170188387650512141, 0.3333333333333333703, 0.3170188387650512141, 0.3333333333333333703, 0.3170188387650512141, 0.3333333333333333703, 0.3170188387650512141, 0.3333333333333333703, 0.3170188387650512141, 0.3333333333333333703, 0.3170188387650512141, 0.3333333333333333703, 0.3170188387650512141, 0.3333333333333333703, 0.3170188387650512141, 0.3333333333333333703, 0.3170188387650512141, 0.3333333333333333703, 0.3170188387650512141, 0.3333333333333333703, 0.3170188387650512141, 0.3333333333333333703, 0.3170188387650512141, 0.3333333333333333703, 0.3170188387650512141, 0.3333333333333333703, 0.3170188387650512141, 0.3333333333333333703, 0.3170188387650512141, 0.3333333333333333703, 0.3170188387650512141, 0.3333333333333333703, 0.3170188387650512141, 0.3333333333333333703, 0.3170188387650512141, 0.3333333333333333703, 0.3170188387650512141, 0.3333333333333333703, 0.3170188387650512141, 0.3333333333333333703, 0.3170188387650512141, 0.3333333333333333703, 0.3170188387650512141, 0.3333333333333333703, 0.3170188387650512141, 0.3333333333333333703, 0.3170188387650512141, 0.3333333333333333703, 0.3170188387650512141, 0.3333333333333333703, 0.3170188387650512141, 0.3333333333333333703, 0.3170188387650512141, 0.3333333333333333703, 0.3170188387650512141, 0.3333333333333333703, 0.3170188387650512141, 0.3333333333333333703, 0.3170188387650512141, 0.3333333333333333703, 0.3170188387650512141, 0.3333333333333333703, 0.3170188387650512141, 0.3333333333333333703, 0.3170188387650512141, 0.3333333333333333703, 0.3170188387650512141, 0.3333333333333333703, 0.3170188387650512141, 0.3333333333333333703, 0.3170188387650512141, 0.3333333333333333703, 0.3170188387650512141, 0.3333333333333333703, 0.3170188387650512141, 0.3333333333333333703, 0.3170188387650512141, 0.3333333333333333703, 0.3170188387650512141, 0.3333333333333333703, 0.3170188387650512141, 0.3333333333333333703, 0.3170188387650512141, 0.3333333333333333703, 0.3170188387650512141, 0.3333333333333333703, 0.3170188387650512141, 0.3333333333333333703, 0.3170188387650512141, 0.3333333333333333703, 0.3170188387650512141, 0.3333333333333333703, 0.3170188387650512141, 0.3333333333333333703, 0.3170188387650512141, 0.3333333333333333703, 0.3170188387650512141, 0.3333333333333333703, 0.3170188387650512141, 0.3333333333333333703, 0.3170188387650512141, 0.3333333333333333703, 0.3170188387650512141, 0.3333333333333333703, 0.3170188387650512141, 0.3333333333333333703, 0.3170188387650512141, 0.3333333333333333703, 0.3170188387650512141, 0.3333333333333333703, 0.3170188387650512141, 0.3333333333333333703, 0.3170188387650512141, 0.3333333333333333703, 0.3170188387650512141, 0.3333333333333333703, 0.3170188387650512141, 0.3333333333333333703, 0.3170188387650512141, 0.3333333333333333703, 0.3170188387650512141, 0.3333333333333333703, 0.3170188387650512141, 0.3333333333333333703, 0.3170188387650512141, 0.3333333333333333703, 0.3170188387650512141, 0.3333333333333333703, 0.3170188387650512141, 0.3333333333333333703, 0.3170188387650512141, 0.3333333333333333703, 0.3170188387650512141, 0.3333333333333333703, 0.3170188387650512141, 0.3333333333333333703, 0.3170188387650512141, 0.3333333333333333703, 0.3170188387650512141, 0.3333333333333333703, 0.3170188387650512141, 0.3333333333333333703, 0.3170188387650512141, 0.3333333333333333703, 0.3170188387650512141, 0.3333333333333333703, 0.3170188387650512141, 0.3333333333333333703, 0.3170188387650512141, 0.3333333333333333703, 0.3170188387650512141, 0.3333333333333333703, 0.3170188387650512141, 0.3333333333333333703, 0.3170188387650512141, 0.3333333333333333703, 0.3170188387650512141, 0.3333333333333333703, 0.3170188387650512141, 0.3333333333333333703, 0.3170188387650512141, 0.3333333333333333703, 0.3170188387650512141, 0.3333333333333333703, 0.3170188387650512141, 0.3333333333333333703, 0.3170188387650512141, 0.3333333333333333703, 0.3170188387650512141, 0.3333333333333333703, 0.3170188387650512141, 0.3333333333333333703, 0.3170188387650512141, 0.3333333333333333703, 0.3170188387650512141, 0.3333333333333333703, 0.3170188387650512141, 0.3333333333333333703, 0.3170188387650512141, 0.3333333333333333703, 0.3170188387650512141, 0.3333333333333333703, 0.3170188387650512141, 0.3333333333333333703, 0.3170188387650512141, 0.3333333333333333703, 0.3170188387650512141, 0.3333333333333333703, 0.3170188387650512141, 0.3333333333333333703, 0.3170188387650512141, 0.3333333333333333703, 0.3170188387650512141, 0.3333333333333333703, 0.3170188387650512141, 0.3333333333333333703, 0.3170188387650512141, 0.3333333333333333703, 0.3170188387650512141, 0.3333333333333333703, 0.3170188387650512141, 0.3333333333333333703, 0.3170188387650512141, 0.3333333333333333703, 0.3170188387650512141, 0.3333333333333333703, 0.3170188387650512141, 0.3333333333333333703, 0.3170188387650512141, 0.3333333333333333703, 0.3170188387650512141, 0.3333333333333333703, 0.3170188387650512141, 0.3333333333333333703, 0.3170188387650512141, 0.3333333333333333703, 0.3170188387650512141, 0.3333333333333333703, 0.3170188387650512141, 0.3333333333333333703, 0.3170188387650512141, 0.3333333333333333703, 0.3170188387650512141, 0.3333333333333333703, 0.3170188387650512141, 0.3333333333333333703, 0.3170188387650512141, 0.3333333333333333703, 0.3170188387650512141, 0.3333333333333333703, 0.3170188387650512141, 0.3333333333333333703, 0.3170188387650512141, 0.3333333333333333703, 0.3170188387650512141, 0.3333333333333333703, 0.3170188387650512141, 0.3333333333333333703, 0.3170188387650512141, 0.3333333333333333703, 0.3170188387650512141, 0.3333333333333333703, 0.3170188387650512141, 0.3333333333333333703, 0.3170188387650512141, 0.3333333333333333703, 0.3170188387650512141, 0.3333333333333333703, 0.3170188387650512141, 0.3333333333333333703, 0.3170188387650512141, 0.3333333333333333703, 0.3170188387650512141, 0.3333333333333333703, 0.3170188387650512141, 0.3333333333333333703, 0.3170188387650512141, 0.3333333333333333703, 0.3170188387650512141, 0.3333333333333333703, 0.3170188387650512141, 0.3333333333333333703, 0.3170188387650512141, 0.3333333333333333703, 0.3170188387650512141, 0.3333333333333333703, 0.3170188387650512141, 0.3333333333333333703, 0.3170188387650512141, 0.3333333333333333703, 0.3170188387650512141, 0.3333333333333333703, 0.3170188387650512141, 0.3333333333333333703, 0.3170188387650512141, 0.3333333333333333703, 0.3170188387650512141, 0.3333333333333333703, 0.3170188387650512141, 0.3333333333333333703, 0.3170188387650512141, 0.3333333333333333703, 0.3170188387650512141, 0.3333333333333333703, 0.3170188387650512141, 0.3333333333333333703, 0.3170188387650512141, 0.3333333333333333703, 0.3170188387650512141, 0.3333333333333333703, 0.3170188387650512141, 0.3333333333333333703, 0.3170188387650512141, 0.3333333333333333703, 0.3170188387650512141, 0.3333333333333333703, 0.3170188387650512141, 0.3333333333333333703, 0.3170188387650512141, 0.3333333333333333703, 0.3170188387650512141, 0.3333333333333333703, 0.3170188387650512141, 0.3333333333333333703, 0.3170188387650512141, 0.3333333333333333703, 0.3170188387650512141, 0.3333333333333333703, 0.3170188387650512141, 0.3333333333333333703, 0.3170188387650512141, 0.3333333333333333703, 0.3170188387650512141, 0.3333333333333333703, 0.3170188387650512141, 0.3333333333333333703, 0.3170188387650512141, 0.3333333333333333703, 0.3170188387650512141, 0.3333333333333333703, 0.3170188387650512141, 0.3333333333333333703, 0.3170188387650512141, 0.3333333333333333703, 0.3170188387650512141, 0.3333333333333333703, 0.3170188387650512141, 0.3333333333333333703, 0.3170188387650512141, 0.3333333333333333703, 0.3170188387650512141, 0.3333333333333333703, 0.3170188387650512141, 0.3333333333333333703, 0.3170188387650512141, 0.3333333333333333703, 0.3170188387650512141, 0.3333333333333333703, 0.3170188387650512141, 0.3333333333333333703, 0.3170188387650512141, 0.3333333333333333703, 0.3170188387650512141, 0.3333333333333333703, 0.3170188387650512141, 0.3333333333333333703, 0.3170188387650512141, 0.3333333333333333703, 0.3170188387650512141, 0.3333333333333333703, 0.3170188387650512141, 0.3333333333333333703, 0.3170188387650512141, 0.3333333333333333703, 0.3170188387650512141, 0.3333333333333333703, 0.3170188387650512141, 0.3333333333333333703, 0.3170188387650512141, 0.3333333333333333703, 0.3170188387650512141, 0.3333333333333333703, 0.3170188387650512141, 0.3333333333333333703, 0.3170188387650512141, 0.3333333333333333703, 0.3170188387650512141, 0.3333333333333333703, 0.3170188387650512141, 0.3333333333333333703, 0.3170188387650512141, 0.3333333333333333703, 0.3170188387650512141, 0.3333333333333333703, 0.3170188387650512141, 0.3333333333333333703, 0.3170188387650512141, 0.3333333333333333703, 0.3170188387650512141, 0.3333333333333333703, 0.3170188387650512141, 0.3333333333333333703, 0.3170188387650512141, 0.3333333333333333703, 0.3170188387650512141, 0.3333333333333333703, 0.3170188387650512141, 0.3333333333333333703, 0.3170188387650512141, 0.3333333333333333703, 0.3170188387650512141, 0.3333333333333333703, 0.3170188387650512141, 0.3333333333333333703, 0.3170188387650512141, 0.3333333333333333703, 0.3170188387650512141, 0.3333333333333333703, 0.3170188387650512141, 0.3333333333333333703, 0.3170188387650512141, 0.3333333333333333703, 0.3170188387650512141, 0.3333333333333333703, 0.3170188387650512141, 0.3333333333333333703, 0.3170188387650512141, 0.3333333333333333703, 0.3170188387650512141, 0.3333333333333333703, 0.3170188387650512141, 0.3333333333333333703, 0.3170188387650512141, 0.3333333333333333703, 0.3170188387650512141, 0.3333333333333333703, 0.3170188387650512141, 0.3333333333333333703, 0.3170188387650512141, 0.3333333333333333703, 0.3170188387650512141, 0.3333333333333333703, 0.3170188387650512141, 0.3333333333333333703, 0.3170188387650512141, 0.3333333333333333703, 0.3333333333333333703, 0.3333333333333333703),
 ( 0.3333333333333333703, 0.3170188387650512141, 0.3333333333333333703, 0.3170188387650512141, 0.3333333333333333703, 0.3170188387650512141, 0.3333333333333333703, 0.3170188387650512141, 0.3333333333333333703, 0.3170188387650512141, 0.3333333333333333703, 0.3170188387650512141, 0.3333333333333333703, 0.3170188387650512141, 0.3333333333333333703, 0.3170188387650512141, 0.3333333333333333703, 0.3170188387650512141, 0.3333333333333333703, 0.3170188387650512141, 0.3333333333333333703, 0.3170188387650512141, 0.3333333333333333703, 0.3170188387650512141, 0.3333333333333333703, 0.3170188387650512141, 0.3333333333333333703, 0.3170188387650512141, 0.3333333333333333703, 0.3170188387650512141, 0.3333333333333333703, 0.3170188387650512141, 0.3333333333333333703, 0.3170188387650512141, 0.3333333333333333703, 0.3170188387650512141, 0.3333333333333333703, 0.3170188387650512141, 0.3333333333333333703, 0.3170188387650512141, 0.3333333333333333703, 0.3170188387650512141, 0.3333333333333333703, 0.3170188387650512141, 0.3333333333333333703, 0.3170188387650512141, 0.3333333333333333703, 0.3170188387650512141, 0.3333333333333333703, 0.3170188387650512141, 0.3333333333333333703, 0.3170188387650512141, 0.3333333333333333703, 0.3170188387650512141, 0.3333333333333333703, 0.3170188387650512141, 0.3333333333333333703, 0.3170188387650512141, 0.3333333333333333703, 0.3170188387650512141, 0.3333333333333333703, 0.3170188387650512141, 0.3333333333333333703, 0.3170188387650512141, 0.3333333333333333703, 0.3170188387650512141, 0.3333333333333333703, 0.3170188387650512141, 0.3333333333333333703, 0.3170188387650512141, 0.3333333333333333703, 0.3170188387650512141, 0.3333333333333333703, 0.3170188387650512141, 0.3333333333333333703, 0.3170188387650512141, 0.3333333333333333703, 0.3170188387650512141, 0.3333333333333333703, 0.3170188387650512141, 0.3333333333333333703, 0.3170188387650512141, 0.3333333333333333703, 0.3170188387650512141, 0.3333333333333333703, 0.3170188387650512141, 0.3333333333333333703, 0.3170188387650512141, 0.3333333333333333703, 0.3170188387650512141, 0.3333333333333333703, 0.3170188387650512141, 0.3333333333333333703, 0.3170188387650512141, 0.3333333333333333703, 0.3170188387650512141, 0.3333333333333333703, 0.3170188387650512141, 0.3333333333333333703, 0.3170188387650512141, 0.3333333333333333703, 0.3170188387650512141, 0.3333333333333333703, 0.3170188387650512141, 0.3333333333333333703, 0.3170188387650512141, 0.3333333333333333703, 0.3170188387650512141, 0.3333333333333333703, 0.3170188387650512141, 0.3333333333333333703, 0.3170188387650512141, 0.3333333333333333703, 0.3170188387650512141, 0.3333333333333333703, 0.3170188387650512141, 0.3333333333333333703, 0.3170188387650512141, 0.3333333333333333703, 0.3170188387650512141, 0.3333333333333333703, 0.3170188387650512141, 0.3333333333333333703, 0.3170188387650512141, 0.3333333333333333703, 0.3170188387650512141, 0.3333333333333333703, 0.3170188387650512141, 0.3333333333333333703, 0.3170188387650512141, 0.3333333333333333703, 0.3170188387650512141, 0.3333333333333333703, 0.3170188387650512141, 0.3333333333333333703, 0.3170188387650512141, 0.3333333333333333703, 0.3170188387650512141, 0.3333333333333333703, 0.3170188387650512141, 0.3333333333333333703, 0.3170188387650512141, 0.3333333333333333703, 0.3170188387650512141, 0.3333333333333333703, 0.3170188387650512141, 0.3333333333333333703, 0.3170188387650512141, 0.3333333333333333703, 0.3170188387650512141, 0.3333333333333333703, 0.3170188387650512141, 0.3333333333333333703, 0.3170188387650512141, 0.3333333333333333703, 0.3170188387650512141, 0.3333333333333333703, 0.3170188387650512141, 0.3333333333333333703, 0.3170188387650512141, 0.3333333333333333703, 0.3170188387650512141, 0.3333333333333333703, 0.3170188387650512141, 0.3333333333333333703, 0.3170188387650512141, 0.3333333333333333703, 0.3170188387650512141, 0.3333333333333333703, 0.3170188387650512141, 0.3333333333333333703, 0.3170188387650512141, 0.3333333333333333703, 0.3170188387650512141, 0.3333333333333333703, 0.3170188387650512141, 0.3333333333333333703, 0.3170188387650512141, 0.3333333333333333703, 0.3170188387650512141, 0.3333333333333333703, 0.3170188387650512141, 0.3333333333333333703, 0.3170188387650512141, 0.3333333333333333703, 0.3170188387650512141, 0.3333333333333333703, 0.3170188387650512141, 0.3333333333333333703, 0.3170188387650512141, 0.3333333333333333703, 0.3170188387650512141, 0.3333333333333333703, 0.3170188387650512141, 0.3333333333333333703, 0.3170188387650512141, 0.3333333333333333703, 0.3170188387650512141, 0.3333333333333333703, 0.3170188387650512141, 0.3333333333333333703, 0.3170188387650512141, 0.3333333333333333703, 0.3170188387650512141, 0.3333333333333333703, 0.3170188387650512141, 0.3333333333333333703, 0.3170188387650512141, 0.3333333333333333703, 0.3170188387650512141, 0.3333333333333333703, 0.3170188387650512141, 0.3333333333333333703, 0.3170188387650512141, 0.3333333333333333703, 0.3170188387650512141, 0.3333333333333333703, 0.3170188387650512141, 0.3333333333333333703, 0.3170188387650512141, 0.3333333333333333703, 0.3170188387650512141, 0.3333333333333333703, 0.3170188387650512141, 0.3333333333333333703, 0.3170188387650512141, 0.3333333333333333703, 0.3170188387650512141, 0.3333333333333333703, 0.3170188387650512141, 0.3333333333333333703, 0.3170188387650512141, 0.3333333333333333703, 0.3170188387650512141, 0.3333333333333333703, 0.3170188387650512141, 0.3333333333333333703, 0.3170188387650512141, 0.3333333333333333703, 0.3170188387650512141, 0.3333333333333333703, 0.3170188387650512141, 0.3333333333333333703, 0.3170188387650512141, 0.3333333333333333703, 0.3170188387650512141, 0.3333333333333333703, 0.3170188387650512141, 0.3333333333333333703, 0.3170188387650512141, 0.3333333333333333703, 0.3170188387650512141, 0.3333333333333333703, 0.3170188387650512141, 0.3333333333333333703, 0.3170188387650512141, 0.3333333333333333703, 0.3170188387650512141, 0.3333333333333333703, 0.3170188387650512141, 0.3333333333333333703, 0.3170188387650512141, 0.3333333333333333703, 0.3170188387650512141, 0.3333333333333333703, 0.3170188387650512141, 0.3333333333333333703, 0.3170188387650512141, 0.3333333333333333703, 0.3170188387650512141, 0.3333333333333333703, 0.3170188387650512141, 0.3333333333333333703, 0.3170188387650512141, 0.3333333333333333703, 0.3170188387650512141, 0.3333333333333333703, 0.3170188387650512141, 0.3333333333333333703, 0.3170188387650512141, 0.3333333333333333703, 0.3170188387650512141, 0.3333333333333333703, 0.3170188387650512141, 0.3333333333333333703, 0.3170188387650512141, 0.3333333333333333703, 0.3170188387650512141, 0.3333333333333333703, 0.3170188387650512141, 0.3333333333333333703, 0.3170188387650512141, 0.3333333333333333703, 0.3170188387650512141, 0.3333333333333333703, 0.3170188387650512141, 0.3333333333333333703, 0.3170188387650512141, 0.3333333333333333703, 0.3170188387650512141, 0.3333333333333333703, 0.3170188387650512141, 0.3333333333333333703, 0.3170188387650512141, 0.3333333333333333703, 0.3170188387650512141, 0.3333333333333333703, 0.3170188387650512141, 0.3333333333333333703, 0.3170188387650512141, 0.3333333333333333703, 0.3170188387650512141, 0.3333333333333333703, 0.3170188387650512141, 0.3333333333333333703, 0.3170188387650512141, 0.3333333333333333703, 0.3170188387650512141, 0.3333333333333333703, 0.3170188387650512141, 0.3333333333333333703, 0.3170188387650512141, 0.3333333333333333703, 0.3170188387650512141, 0.3333333333333333703, 0.3170188387650512141, 0.3333333333333333703, 0.3170188387650512141, 0.3333333333333333703, 0.3170188387650512141, 0.3333333333333333703, 0.3170188387650512141, 0.3333333333333333703, 0.3170188387650512141, 0.3333333333333333703, 0.3170188387650512141, 0.3333333333333333703, 0.3170188387650512141, 0.3333333333333333703, 0.3170188387650512141, 0.3333333333333333703, 0.3170188387650512141, 0.3333333333333333703, 0.3170188387650512141, 0.3333333333333333703, 0.3170188387650512141, 0.3333333333333333703, 0.3170188387650512141, 0.3333333333333333703, 0.3170188387650512141, 0.3333333333333333703, 0.3170188387650512141, 0.3333333333333333703, 0.3170188387650512141, 0.3333333333333333703, 0.3170188387650512141, 0.3333333333333333703, 0.3170188387650512141, 0.3333333333333333703, 0.3170188387650512141, 0.3333333333333333703, 0.3170188387650512141, 0.3333333333333333703, 0.3170188387650512141, 0.3333333333333333703, 0.3170188387650512141, 0.3333333333333333703, 0.3170188387650512141, 0.3333333333333333703, 0.3170188387650512141, 0.3333333333333333703, 0.3170188387650512141, 0.3333333333333333703, 0.3170188387650512141, 0.3333333333333333703, 0.3170188387650512141, 0.3333333333333333703, 0.3170188387650512141, 0.3333333333333333703, 0.3170188387650512141, 0.3333333333333333703, 0.3170188387650512141, 0.3333333333333333703, 0.3170188387650512141, 0.3333333333333333703, 0.3170188387650512141, 0.3333333333333333703, 0.3170188387650512141, 0.3333333333333333703, 0.3170188387650512141, 0.3333333333333333703, 0.3170188387650512141, 0.3333333333333333703, 0.3170188387650512141, 0.3333333333333333703, 0.3170188387650512141, 0.3333333333333333703, 0.3170188387650512141, 0.3333333333333333703, 0.3170188387650512141, 0.3333333333333333703, 0.3170188387650512141, 0.3333333333333333703, 0.3170188387650512141, 0.3333333333333333703, 0.3170188387650512141, 0.3333333333333333703, 0.3170188387650512141, 0.3333333333333333703, 0.3170188387650512141, 0.3333333333333333703, 0.3170188387650512141, 0.3333333333333333703, 0.3170188387650512141, 0.3333333333333333703, 0.3170188387650512141, 0.3333333333333333703, 0.3170188387650512141, 0.3333333333333333703, 0.3170188387650512141, 0.3333333333333333703, 0.3170188387650512141, 0.3333333333333333703, 0.3170188387650512141, 0.3333333333333333703, 0.3170188387650512141, 0.3333333333333333703, 0.3170188387650512141, 0.3333333333333333703, 0.3170188387650512141, 0.3333333333333333703, 0.3170188387650512141, 0.3333333333333333703, 0.3170188387650512141, 0.3333333333333333703, 0.3170188387650512141, 0.3333333333333333703, 0.3170188387650512141, 0.3333333333333333703, 0.3170188387650512141, 0.3333333333333333703, 0.3170188387650512141, 0.3333333333333333703, 0.3170188387650512141, 0.3333333333333333703, 0.3170188387650512141, 0.3333333333333333703, 0.3170188387650512141, 0.3333333333333333703, 0.3170188387650512141, 0.3333333333333333703, 0.3170188387650512141, 0.3333333333333333703, 0.3170188387650512141, 0.3333333333333333703, 0.3170188387650512141, 0.3333333333333333703, 0.3170188387650512141, 0.3333333333333333703, 0.3170188387650512141, 0.3333333333333333703, 0.3170188387650512141, 0.3333333333333333703, 0.3170188387650512141, 0.3333333333333333703, 0.3170188387650512141, 0.3333333333333333703, 0.3170188387650512141, 0.3333333333333333703, 0.3170188387650512141, 0.3333333333333333703, 0.3170188387650512141, 0.3333333333333333703, 0.3170188387650512141, 0.3333333333333333703, 0.3170188387650512141, 0.3333333333333333703, 0.3170188387650512141, 0.3333333333333333703, 0.3170188387650512141, 0.3333333333333333703, 0.3170188387650512141, 0.3333333333333333703, 0.3170188387650512141, 0.3333333333333333703, 0.3170188387650512141, 0.3333333333333333703, 0.3170188387650512141, 0.3333333333333333703, 0.3170188387650512141, 0.3333333333333333703, 0.3170188387650512141, 0.3333333333333333703, 0.3170188387650512141, 0.3333333333333333703, 0.3170188387650512141, 0.3333333333333333703, 0.3170188387650512141, 0.3333333333333333703, 0.3170188387650512141, 0.3333333333333333703, 0.3170188387650512141, 0.3333333333333333703, 0.3170188387650512141, 0.3333333333333333703, 0.3170188387650512141, 0.3333333333333333703, 0.3170188387650512141, 0.3333333333333333703, 0.3170188387650512141, 0.3333333333333333703, 0.3170188387650512141, 0.3333333333333333703, 0.3170188387650512141, 0.3333333333333333703, 0.3170188387650512141, 0.3333333333333333703, 0.3170188387650512141, 0.3333333333333333703, 0.3170188387650512141, 0.3333333333333333703, 0.3170188387650512141, 0.3333333333333333703, 0.3170188387650512141, 0.3333333333333333703, 0.3170188387650512141, 0.3333333333333333703, 0.3170188387650512141, 0.3333333333333333703, 0.3170188387650512141, 0.3333333333333333703, 0.3170188387650512141, 0.3333333333333333703, 0.3170188387650512141, 0.3333333333333333703, 0.3170188387650512141, 0.3333333333333333703, 0.3170188387650512141, 0.3333333333333333703, 0.3170188387650512141, 0.3333333333333333703, 0.3170188387650512141, 0.3333333333333333703, 0.3170188387650512141, 0.3333333333333333703, 0.3170188387650512141, 0.3333333333333333703, 0.3170188387650512141, 0.3333333333333333703, 0.3170188387650512141, 0.3333333333333333703, 0.3170188387650512141, 0.3333333333333333703, 0.3170188387650512141, 0.3333333333333333703, 0.3170188387650512141, 0.3333333333333333703, 0.3170188387650512141, 0.3333333333333333703, 0.3170188387650512141, 0.3333333333333333703, 0.3170188387650512141, 0.3333333333333333703, 0.3170188387650512141, 0.3333333333333333703, 0.3170188387650512141, 0.3333333333333333703, 0.3170188387650512141, 0.3333333333333333703, 0.3170188387650512141, 0.3333333333333333703, 0.3170188387650512141, 0.3333333333333333703, 0.3170188387650512141, 0.3333333333333333703, 0.3170188387650512141, 0.3333333333333333703, 0.3170188387650512141, 0.3333333333333333703, 0.3170188387650512141, 0.3333333333333333703, 0.3170188387650512141, 0.3333333333333333703, 0.3170188387650512141, 0.3333333333333333703, 0.3170188387650512141, 0.3333333333333333703, 0.3170188387650512141, 0.3333333333333333703, 0.3170188387650512141, 0.3333333333333333703, 0.3170188387650512141, 0.3333333333333333703, 0.3170188387650512141, 0.3333333333333333703, 0.3170188387650512141, 0.3333333333333333703, 0.3170188387650512141, 0.3333333333333333703, 0.3170188387650512141, 0.3333333333333333703, 0.3170188387650512141, 0.3333333333333333703, 0.3170188387650512141, 0.3333333333333333703, 0.3170188387650512141, 0.3333333333333333703, 0.3170188387650512141, 0.3333333333333333703, 0.3170188387650512141, 0.3333333333333333703, 0.3170188387650512141, 0.3333333333333333703, 0.3170188387650512141, 0.3333333333333333703, 0.3170188387650512141, 0.3333333333333333703, 0.3170188387650512141, 0.3333333333333333703, 0.3170188387650512141, 0.3333333333333333703, 0.3170188387650512141, 0.3333333333333333703, 0.3170188387650512141, 0.3333333333333333703, 0.3170188387650512141, 0.3333333333333333703, 0.3170188387650512141, 0.3333333333333333703, 0.3170188387650512141, 0.3333333333333333703, 0.3170188387650512141, 0.3333333333333333703, 0.3170188387650512141, 0.3333333333333333703, 0.3170188387650512141, 0.3333333333333333703, 0.3170188387650512141, 0.3333333333333333703, 0.3170188387650512141, 0.3333333333333333703, 0.3170188387650512141, 0.3333333333333333703, 0.3170188387650512141, 0.3333333333333333703, 0.3170188387650512141, 0.3333333333333333703, 0.3170188387650512141, 0.3333333333333333703, 0.3170188387650512141, 0.3333333333333333703, 0.3170188387650512141, 0.3333333333333333703, 0.3170188387650512141, 0.3333333333333333703, 0.3170188387650512141, 0.3333333333333333703, 0.3170188387650512141, 0.3333333333333333703, 0.3170188387650512141, 0.3333333333333333703, 0.3170188387650512141, 0.3333333333333333703, 0.3170188387650512141, 0.3333333333333333703, 0.3170188387650512141, 0.3333333333333333703, 0.3170188387650512141, 0.3333333333333333703, 0.3170188387650512141, 0.3333333333333333703, 0.3170188387650512141, 0.3333333333333333703, 0.3170188387650512141, 0.3333333333333333703, 0.3170188387650512141, 0.3333333333333333703, 0.3170188387650512141, 0.3333333333333333703, 0.3170188387650512141, 0.3333333333333333703, 0.3170188387650512141, 0.3333333333333333703, 0.3170188387650512141, 0.3333333333333333703, 0.3170188387650512141, 0.3333333333333333703, 0.3170188387650512141, 0.3333333333333333703, 0.3170188387650512141, 0.3333333333333333703, 0.3333333333333333703, 0.3333333333333333703),
 ( 1.000000000000000000, 0.9510565162951535312, 1.000000000000000000, 0.9510565162951535312, 1.000000000000000000, 0.9510565162951535312, 1.000000000000000000, 0.9510565162951535312, 1.000000000000000000, 0.9510565162951535312, 1.000000000000000000, 0.9510565162951535312, 1.000000000000000000, 0.9510565162951535312, 1.000000000000000000, 0.9510565162951535312, 1.000000000000000000, 0.9510565162951535312, 1.000000000000000000, 0.9510565162951535312, 1.000000000000000000, 0.9510565162951535312, 1.000000000000000000, 0.9510565162951535312, 1.000000000000000000, 0.9510565162951535312, 1.000000000000000000, 0.9510565162951535312, 1.000000000000000000, 0.9510565162951535312, 1.000000000000000000, 0.9510565162951535312, 1.000000000000000000, 0.9510565162951535312, 1.000000000000000000, 0.9510565162951535312, 1.000000000000000000, 0.9510565162951535312, 1.000000000000000000, 0.9510565162951535312, 1.000000000000000000, 0.9510565162951535312, 1.000000000000000000, 0.9510565162951535312, 1.000000000000000000, 0.9510565162951535312, 1.000000000000000000, 0.9510565162951535312, 1.000000000000000000, 0.9510565162951535312, 1.000000000000000000, 0.9510565162951535312, 1.000000000000000000, 0.9510565162951535312, 1.000000000000000000, 0.9510565162951535312, 1.000000000000000000, 0.9510565162951535312, 1.000000000000000000, 0.9510565162951535312, 1.000000000000000000, 0.9510565162951535312, 1.000000000000000000, 0.9510565162951535312, 1.000000000000000000, 0.9510565162951535312, 1.000000000000000000, 0.9510565162951535312, 1.000000000000000000, 0.9510565162951535312, 1.000000000000000000, 0.9510565162951535312, 1.000000000000000000, 0.9510565162951535312, 1.000000000000000000, 0.9510565162951535312, 1.000000000000000000, 0.9510565162951535312, 1.000000000000000000, 0.9510565162951535312, 1.000000000000000000, 0.9510565162951535312, 1.000000000000000000, 0.9510565162951535312, 1.000000000000000000, 0.9510565162951535312, 1.000000000000000000, 0.9510565162951535312, 1.000000000000000000, 0.9510565162951535312, 1.000000000000000000, 0.9510565162951535312, 1.000000000000000000, 0.9510565162951535312, 1.000000000000000000, 0.9510565162951535312, 1.000000000000000000, 0.9510565162951535312, 1.000000000000000000, 0.9510565162951535312, 1.000000000000000000, 0.9510565162951535312, 1.000000000000000000, 0.9510565162951535312, 1.000000000000000000, 0.9510565162951535312, 1.000000000000000000, 0.9510565162951535312, 1.000000000000000000, 0.9510565162951535312, 1.000000000000000000, 0.9510565162951535312, 1.000000000000000000, 0.9510565162951535312, 1.000000000000000000, 0.9510565162951535312, 1.000000000000000000, 0.9510565162951535312, 1.000000000000000000, 0.9510565162951535312, 1.000000000000000000, 0.9510565162951535312, 1.000000000000000000, 0.9510565162951535312, 1.000000000000000000, 0.9510565162951535312, 1.000000000000000000, 0.9510565162951535312, 1.000000000000000000, 0.9510565162951535312, 1.000000000000000000, 0.9510565162951535312, 1.000000000000000000, 0.9510565162951535312, 1.000000000000000000, 0.9510565162951535312, 1.000000000000000000, 0.9510565162951535312, 1.000000000000000000, 0.9510565162951535312, 1.000000000000000000, 0.9510565162951535312, 1.000000000000000000, 0.9510565162951535312, 1.000000000000000000, 0.9510565162951535312, 1.000000000000000000, 0.9510565162951535312, 1.000000000000000000, 0.9510565162951535312, 1.000000000000000000, 0.9510565162951535312, 1.000000000000000000, 0.9510565162951535312, 1.000000000000000000, 0.9510565162951535312, 1.000000000000000000, 0.9510565162951535312, 1.000000000000000000, 0.9510565162951535312, 1.000000000000000000, 0.9510565162951535312, 1.000000000000000000, 0.9510565162951535312, 1.000000000000000000, 0.9510565162951535312, 1.000000000000000000, 0.9510565162951535312, 1.000000000000000000, 0.9510565162951535312, 1.000000000000000000, 0.9510565162951535312, 1.000000000000000000, 0.9510565162951535312, 1.000000000000000000, 0.9510565162951535312, 1.000000000000000000, 0.9510565162951535312, 1.000000000000000000, 0.9510565162951535312, 1.000000000000000000, 0.9510565162951535312, 1.000000000000000000, 0.9510565162951535312, 1.000000000000000000, 0.9510565162951535312, 1.000000000000000000, 0.9510565162951535312, 1.000000000000000000, 0.9510565162951535312, 1.000000000000000000, 0.9510565162951535312, 1.000000000000000000, 0.9510565162951535312, 1.000000000000000000, 0.9510565162951535312, 1.000000000000000000, 0.9510565162951535312, 1.000000000000000000, 0.9510565162951535312, 1.000000000000000000, 0.9510565162951535312, 1.000000000000000000, 0.9510565162951535312, 1.000000000000000000, 0.9510565162951535312, 1.000000000000000000, 0.9510565162951535312, 1.000000000000000000, 0.9510565162951535312, 1.000000000000000000, 0.9510565162951535312, 1.000000000000000000, 0.9510565162951535312, 1.000000000000000000, 0.9510565162951535312, 1.000000000000000000, 0.9510565162951535312, 1.000000000000000000, 0.9510565162951535312, 1.000000000000000000, 0.9510565162951535312, 1.000000000000000000, 0.9510565162951535312, 1.000000000000000000, 0.9510565162951535312, 1.000000000000000000, 0.9510565162951535312, 1.000000000000000000, 0.9510565162951535312, 1.000000000000000000, 0.9510565162951535312, 1.000000000000000000, 0.9510565162951535312, 1.000000000000000000, 0.9510565162951535312, 1.000000000000000000, 0.9510565162951535312, 1.000000000000000000, 0.9510565162951535312, 1.000000000000000000, 0.9510565162951535312, 1.000000000000000000, 0.9510565162951535312, 1.000000000000000000, 0.9510565162951535312, 1.000000000000000000, 0.9510565162951535312, 1.000000000000000000, 0.9510565162951535312, 1.000000000000000000, 0.9510565162951535312, 1.000000000000000000, 0.9510565162951535312, 1.000000000000000000, 0.9510565162951535312, 1.000000000000000000, 0.9510565162951535312, 1.000000000000000000, 0.9510565162951535312, 1.000000000000000000, 0.9510565162951535312, 1.000000000000000000, 0.9510565162951535312, 1.000000000000000000, 0.9510565162951535312, 1.000000000000000000, 0.9510565162951535312, 1.000000000000000000, 0.9510565162951535312, 1.000000000000000000, 0.9510565162951535312, 1.000000000000000000, 0.9510565162951535312, 1.000000000000000000, 0.9510565162951535312, 1.000000000000000000, 0.9510565162951535312, 1.000000000000000000, 0.9510565162951535312, 1.000000000000000000, 0.9510565162951535312, 1.000000000000000000, 0.9510565162951535312, 1.000000000000000000, 0.9510565162951535312, 1.000000000000000000, 0.9510565162951535312, 1.000000000000000000, 0.9510565162951535312, 1.000000000000000000, 0.9510565162951535312, 1.000000000000000000, 0.9510565162951535312, 1.000000000000000000, 0.9510565162951535312, 1.000000000000000000, 0.9510565162951535312, 1.000000000000000000, 0.9510565162951535312, 1.000000000000000000, 0.9510565162951535312, 1.000000000000000000, 0.9510565162951535312, 1.000000000000000000, 0.9510565162951535312, 1.000000000000000000, 0.9510565162951535312, 1.000000000000000000, 0.9510565162951535312, 1.000000000000000000, 0.9510565162951535312, 1.000000000000000000, 0.9510565162951535312, 1.000000000000000000, 0.9510565162951535312, 1.000000000000000000, 0.9510565162951535312, 1.000000000000000000, 0.9510565162951535312, 1.000000000000000000, 0.9510565162951535312, 1.000000000000000000, 0.9510565162951535312, 1.000000000000000000, 0.9510565162951535312, 1.000000000000000000, 0.9510565162951535312, 1.000000000000000000, 0.9510565162951535312, 1.000000000000000000, 0.9510565162951535312, 1.000000000000000000, 0.9510565162951535312, 1.000000000000000000, 0.9510565162951535312, 1.000000000000000000, 0.9510565162951535312, 1.000000000000000000, 0.9510565162951535312, 1.000000000000000000, 0.9510565162951535312, 1.000000000000000000, 0.9510565162951535312, 1.000000000000000000, 0.9510565162951535312, 1.000000000000000000, 0.9510565162951535312, 1.000000000000000000, 0.9510565162951535312, 1.000000000000000000, 0.9510565162951535312, 1.000000000000000000, 0.9510565162951535312, 1.000000000000000000, 0.9510565162951535312, 1.000000000000000000, 0.9510565162951535312, 1.000000000000000000, 0.9510565162951535312, 1.000000000000000000, 0.9510565162951535312, 1.000000000000000000, 0.9510565162951535312, 1.000000000000000000, 0.9510565162951535312, 1.000000000000000000, 0.9510565162951535312, 1.000000000000000000, 0.9510565162951535312, 1.000000000000000000, 0.9510565162951535312, 1.000000000000000000, 0.9510565162951535312, 1.000000000000000000, 0.9510565162951535312, 1.000000000000000000, 0.9510565162951535312, 1.000000000000000000, 0.9510565162951535312, 1.000000000000000000, 0.9510565162951535312, 1.000000000000000000, 0.9510565162951535312, 1.000000000000000000, 0.9510565162951535312, 1.000000000000000000, 0.9510565162951535312, 1.000000000000000000, 0.9510565162951535312, 1.000000000000000000, 0.9510565162951535312, 1.000000000000000000, 0.9510565162951535312, 1.000000000000000000, 0.9510565162951535312, 1.000000000000000000, 0.9510565162951535312, 1.000000000000000000, 0.9510565162951535312, 1.000000000000000000, 0.9510565162951535312, 1.000000000000000000, 0.9510565162951535312, 1.000000000000000000, 0.9510565162951535312, 1.000000000000000000, 0.9510565162951535312, 1.000000000000000000, 0.9510565162951535312, 1.000000000000000000, 0.9510565162951535312, 1.000000000000000000, 0.9510565162951535312, 1.000000000000000000, 0.9510565162951535312, 1.000000000000000000, 0.9510565162951535312, 1.000000000000000000, 0.9510565162951535312, 1.000000000000000000, 0.9510565162951535312, 1.000000000000000000, 0.9510565162951535312, 1.000000000000000000, 0.9510565162951535312, 1.000000000000000000, 0.9510565162951535312, 1.000000000000000000, 0.9510565162951535312, 1.000000000000000000, 0.9510565162951535312, 1.000000000000000000, 0.9510565162951535312, 1.000000000000000000, 0.9510565162951535312, 1.000000000000000000, 0.9510565162951535312, 1.000000000000000000, 0.9510565162951535312, 1.000000000000000000, 0.9510565162951535312, 1.000000000000000000, 0.9510565162951535312, 1.000000000000000000, 0.9510565162951535312, 1.000000000000000000, 0.9510565162951535312, 1.000000000000000000, 0.9510565162951535312, 1.000000000000000000, 0.9510565162951535312, 1.000000000000000000, 0.9510565162951535312, 1.000000000000000000, 0.9510565162951535312, 1.000000000000000000, 0.9510565162951535312, 1.000000000000000000, 0.9510565162951535312, 1.000000000000000000, 0.9510565162951535312, 1.000000000000000000, 0.9510565162951535312, 1.000000000000000000, 0.9510565162951535312, 1.000000000000000000, 0.9510565162951535312, 1.000000000000000000, 0.9510565162951535312, 1.000000000000000000, 0.9510565162951535312, 1.000000000000000000, 0.9510565162951535312, 1.000000000000000000, 0.9510565162951535312, 1.000000000000000000, 0.9510565162951535312, 1.000000000000000000, 0.9510565162951535312, 1.000000000000000000, 0.9510565162951535312, 1.000000000000000000, 0.9510565162951535312, 1.000000000000000000, 0.9510565162951535312, 1.000000000000000000, 0.9510565162951535312, 1.000000000000000000, 0.9510565162951535312, 1.000000000000000000, 0.9510565162951535312, 1.000000000000000000, 0.9510565162951535312, 1.000000000000000000, 0.9510565162951535312, 1.000000000000000000, 0.9510565162951535312, 1.000000000000000000, 0.9510565162951535312, 1.000000000000000000, 0.9510565162951535312, 1.000000000000000000, 0.9510565162951535312, 1.000000000000000000, 0.9510565162951535312, 1.000000000000000000, 0.9510565162951535312, 1.000000000000000000, 0.9510565162951535312, 1.000000000000000000, 0.9510565162951535312, 1.000000000000000000, 0.9510565162951535312, 1.000000000000000000, 0.9510565162951535312, 1.000000000000000000, 0.9510565162951535312, 1.000000000000000000, 0.9510565162951535312, 1.000000000000000000, 0.9510565162951535312, 1.000000000000000000, 0.9510565162951535312, 1.000000000000000000, 0.9510565162951535312, 1.000000000000000000, 0.9510565162951535312, 1.000000000000000000, 0.9510565162951535312, 1.000000000000000000, 0.9510565162951535312, 1.000000000000000000, 0.9510565162951535312, 1.000000000000000000, 0.9510565162951535312, 1.000000000000000000, 0.9510565162951535312, 1.000000000000000000, 0.9510565162951535312, 1.000000000000000000, 0.9510565162951535312, 1.000000000000000000, 0.9510565162951535312, 1.000000000000000000, 0.9510565162951535312, 1.000000000000000000, 0.9510565162951535312, 1.000000000000000000, 0.9510565162951535312, 1.000000000000000000, 0.9510565162951535312, 1.000000000000000000, 0.9510565162951535312, 1.000000000000000000, 0.9510565162951535312, 1.000000000000000000, 0.9510565162951535312, 1.000000000000000000, 0.9510565162951535312, 1.000000000000000000, 0.9510565162951535312, 1.000000000000000000, 0.9510565162951535312, 1.000000000000000000, 0.9510565162951535312, 1.000000000000000000, 0.9510565162951535312, 1.000000000000000000, 0.9510565162951535312, 1.000000000000000000, 0.9510565162951535312, 1.000000000000000000, 0.9510565162951535312, 1.000000000000000000, 0.9510565162951535312, 1.000000000000000000, 0.9510565162951535312, 1.000000000000000000, 0.9510565162951535312, 1.000000000000000000, 0.9510565162951535312, 1.000000000000000000, 0.9510565162951535312, 1.000000000000000000, 0.9510565162951535312, 1.000000000000000000, 0.9510565162951535312, 1.000000000000000000, 0.9510565162951535312, 1.000000000000000000, 0.9510565162951535312, 1.000000000000000000, 0.9510565162951535312, 1.000000000000000000, 0.9510565162951535312, 1.000000000000000000, 0.9510565162951535312, 1.000000000000000000, 0.9510565162951535312, 1.000000000000000000, 0.9510565162951535312, 1.000000000000000000, 0.9510565162951535312, 1.000000000000000000, 0.9510565162951535312, 1.000000000000000000, 0.9510565162951535312, 1.000000000000000000, 0.9510565162951535312, 1.000000000000000000, 0.9510565162951535312, 1.000000000000000000, 0.9510565162951535312, 1.000000000000000000, 0.9510565162951535312, 1.000000000000000000, 0.9510565162951535312, 1.000000000000000000, 0.9510565162951535312, 1.000000000000000000, 0.9510565162951535312, 1.000000000000000000, 0.9510565162951535312, 1.000000000000000000, 0.9510565162951535312, 1.000000000000000000, 0.9510565162951535312, 1.000000000000000000, 0.9510565162951535312, 1.000000000000000000, 0.9510565162951535312, 1.000000000000000000, 0.9510565162951535312, 1.000000000000000000, 0.9510565162951535312, 1.000000000000000000, 0.9510565162951535312, 1.000000000000000000, 0.9510565162951535312, 1.000000000000000000, 0.9510565162951535312, 1.000000000000000000, 0.9510565162951535312, 1.000000000000000000, 0.9510565162951535312, 1.000000000000000000, 0.9510565162951535312, 1.000000000000000000, 0.9510565162951535312, 1.000000000000000000, 0.9510565162951535312, 1.000000000000000000, 0.9510565162951535312, 1.000000000000000000, 0.9510565162951535312, 1.000000000000000000, 0.9510565162951535312, 1.000000000000000000, 0.9510565162951535312, 1.000000000000000000, 0.9510565162951535312, 1.000000000000000000, 0.9510565162951535312, 1.000000000000000000, 0.9510565162951535312, 1.000000000000000000, 0.9510565162951535312, 1.000000000000000000, 0.9510565162951535312, 1.000000000000000000, 0.9510565162951535312, 1.000000000000000000, 0.9510565162951535312, 1.000000000000000000, 0.9510565162951535312, 1.000000000000000000, 0.9510565162951535312, 1.000000000000000000, 0.9510565162951535312, 1.000000000000000000, 0.9510565162951535312, 1.000000000000000000, 0.9510565162951535312, 1.000000000000000000, 0.9510565162951535312, 1.000000000000000000, 0.9510565162951535312, 1.000000000000000000, 0.9510565162951535312, 1.000000000000000000, 1.000000000000000000, 1.000000000000000000),
 ( 0.3333333333333333703, 0.3170188387650512141, 0.3333333333333333703, 0.3170188387650512141, 0.3333333333333333703, 0.3170188387650512141, 0.3333333333333333703, 0.3170188387650512141, 0.3333333333333333703, 0.3170188387650512141, 0.3333333333333333703, 0.3170188387650512141, 0.3333333333333333703, 0.3170188387650512141, 0.3333333333333333703, 0.3170188387650512141, 0.3333333333333333703, 0.3170188387650512141, 0.3333333333333333703, 0.3170188387650512141, 0.3333333333333333703, 0.3170188387650512141, 0.3333333333333333703, 0.3170188387650512141, 0.3333333333333333703, 0.3170188387650512141, 0.3333333333333333703, 0.3170188387650512141, 0.3333333333333333703, 0.3170188387650512141, 0.3333333333333333703, 0.3170188387650512141, 0.3333333333333333703, 0.3170188387650512141, 0.3333333333333333703, 0.3170188387650512141, 0.3333333333333333703, 0.3170188387650512141, 0.3333333333333333703, 0.3170188387650512141, 0.3333333333333333703, 0.3170188387650512141, 0.3333333333333333703, 0.3170188387650512141, 0.3333333333333333703, 0.3170188387650512141, 0.3333333333333333703, 0.3170188387650512141, 0.3333333333333333703, 0.3170188387650512141, 0.3333333333333333703, 0.3170188387650512141, 0.3333333333333333703, 0.3170188387650512141, 0.3333333333333333703, 0.3170188387650512141, 0.3333333333333333703, 0.3170188387650512141, 0.3333333333333333703, 0.3170188387650512141, 0.3333333333333333703, 0.3170188387650512141, 0.3333333333333333703, 0.3170188387650512141, 0.3333333333333333703, 0.3170188387650512141, 0.3333333333333333703, 0.3170188387650512141, 0.3333333333333333703, 0.3170188387650512141, 0.3333333333333333703, 0.3170188387650512141, 0.3333333333333333703, 0.3170188387650512141, 0.3333333333333333703, 0.3170188387650512141, 0.3333333333333333703, 0.3170188387650512141, 0.3333333333333333703, 0.3170188387650512141, 0.3333333333333333703, 0.3170188387650512141, 0.3333333333333333703, 0.3170188387650512141, 0.3333333333333333703, 0.3170188387650512141, 0.3333333333333333703, 0.3170188387650512141, 0.3333333333333333703, 0.3170188387650512141, 0.3333333333333333703, 0.3170188387650512141, 0.3333333333333333703, 0.3170188387650512141, 0.3333333333333333703, 0.3170188387650512141, 0.3333333333333333703, 0.3170188387650512141, 0.3333333333333333703, 0.3170188387650512141, 0.3333333333333333703, 0.3170188387650512141, 0.3333333333333333703, 0.3170188387650512141, 0.3333333333333333703, 0.3170188387650512141, 0.3333333333333333703, 0.3170188387650512141, 0.3333333333333333703, 0.3170188387650512141, 0.3333333333333333703, 0.3170188387650512141, 0.3333333333333333703, 0.3170188387650512141, 0.3333333333333333703, 0.3170188387650512141, 0.3333333333333333703, 0.3170188387650512141, 0.3333333333333333703, 0.3170188387650512141, 0.3333333333333333703, 0.3170188387650512141, 0.3333333333333333703, 0.3170188387650512141, 0.3333333333333333703, 0.3170188387650512141, 0.3333333333333333703, 0.3170188387650512141, 0.3333333333333333703, 0.3170188387650512141, 0.3333333333333333703, 0.3170188387650512141, 0.3333333333333333703, 0.3170188387650512141, 0.3333333333333333703, 0.3170188387650512141, 0.3333333333333333703, 0.3170188387650512141, 0.3333333333333333703, 0.3170188387650512141, 0.3333333333333333703, 0.3170188387650512141, 0.3333333333333333703, 0.3170188387650512141, 0.3333333333333333703, 0.3170188387650512141, 0.3333333333333333703, 0.3170188387650512141, 0.3333333333333333703, 0.3170188387650512141, 0.3333333333333333703, 0.3170188387650512141, 0.3333333333333333703, 0.3170188387650512141, 0.3333333333333333703, 0.3170188387650512141, 0.3333333333333333703, 0.3170188387650512141, 0.3333333333333333703, 0.3170188387650512141, 0.3333333333333333703, 0.3170188387650512141, 0.3333333333333333703, 0.3170188387650512141, 0.3333333333333333703, 0.3170188387650512141, 0.3333333333333333703, 0.3170188387650512141, 0.3333333333333333703, 0.3170188387650512141, 0.3333333333333333703, 0.3170188387650512141, 0.3333333333333333703, 0.3170188387650512141, 0.3333333333333333703, 0.3170188387650512141, 0.3333333333333333703, 0.3170188387650512141, 0.3333333333333333703, 0.3170188387650512141, 0.3333333333333333703, 0.3170188387650512141, 0.3333333333333333703, 0.3170188387650512141, 0.3333333333333333703, 0.3170188387650512141, 0.3333333333333333703, 0.3170188387650512141, 0.3333333333333333703, 0.3170188387650512141, 0.3333333333333333703, 0.3170188387650512141, 0.3333333333333333703, 0.3170188387650512141, 0.3333333333333333703, 0.3170188387650512141, 0.3333333333333333703, 0.3170188387650512141, 0.3333333333333333703, 0.3170188387650512141, 0.3333333333333333703, 0.3170188387650512141, 0.3333333333333333703, 0.3170188387650512141, 0.3333333333333333703, 0.3170188387650512141, 0.3333333333333333703, 0.3170188387650512141, 0.3333333333333333703, 0.3170188387650512141, 0.3333333333333333703, 0.3170188387650512141, 0.3333333333333333703, 0.3170188387650512141, 0.3333333333333333703, 0.3170188387650512141, 0.3333333333333333703, 0.3170188387650512141, 0.3333333333333333703, 0.3170188387650512141, 0.3333333333333333703, 0.3170188387650512141, 0.3333333333333333703, 0.3170188387650512141, 0.3333333333333333703, 0.3170188387650512141, 0.3333333333333333703, 0.3170188387650512141, 0.3333333333333333703, 0.3170188387650512141, 0.3333333333333333703, 0.3170188387650512141, 0.3333333333333333703, 0.3170188387650512141, 0.3333333333333333703, 0.3170188387650512141, 0.3333333333333333703, 0.3170188387650512141, 0.3333333333333333703, 0.3170188387650512141, 0.3333333333333333703, 0.3170188387650512141, 0.3333333333333333703, 0.3170188387650512141, 0.3333333333333333703, 0.3170188387650512141, 0.3333333333333333703, 0.3170188387650512141, 0.3333333333333333703, 0.3170188387650512141, 0.3333333333333333703, 0.3170188387650512141, 0.3333333333333333703, 0.3170188387650512141, 0.3333333333333333703, 0.3170188387650512141, 0.3333333333333333703, 0.3170188387650512141, 0.3333333333333333703, 0.3170188387650512141, 0.3333333333333333703, 0.3170188387650512141, 0.3333333333333333703, 0.3170188387650512141, 0.3333333333333333703, 0.3170188387650512141, 0.3333333333333333703, 0.3170188387650512141, 0.3333333333333333703, 0.3170188387650512141, 0.3333333333333333703, 0.3170188387650512141, 0.3333333333333333703, 0.3170188387650512141, 0.3333333333333333703, 0.3170188387650512141, 0.3333333333333333703, 0.3170188387650512141, 0.3333333333333333703, 0.3170188387650512141, 0.3333333333333333703, 0.3170188387650512141, 0.3333333333333333703, 0.3170188387650512141, 0.3333333333333333703, 0.3170188387650512141, 0.3333333333333333703, 0.3170188387650512141, 0.3333333333333333703, 0.3170188387650512141, 0.3333333333333333703, 0.3170188387650512141, 0.3333333333333333703, 0.3170188387650512141, 0.3333333333333333703, 0.3170188387650512141, 0.3333333333333333703, 0.3170188387650512141, 0.3333333333333333703, 0.3170188387650512141, 0.3333333333333333703, 0.3170188387650512141, 0.3333333333333333703, 0.3170188387650512141, 0.3333333333333333703, 0.3170188387650512141, 0.3333333333333333703, 0.3170188387650512141, 0.3333333333333333703, 0.3170188387650512141, 0.3333333333333333703, 0.3170188387650512141, 0.3333333333333333703, 0.3170188387650512141, 0.3333333333333333703, 0.3170188387650512141, 0.3333333333333333703, 0.3170188387650512141, 0.3333333333333333703, 0.3170188387650512141, 0.3333333333333333703, 0.3170188387650512141, 0.3333333333333333703, 0.3170188387650512141, 0.3333333333333333703, 0.3170188387650512141, 0.3333333333333333703, 0.3170188387650512141, 0.3333333333333333703, 0.3170188387650512141, 0.3333333333333333703, 0.3170188387650512141, 0.3333333333333333703, 0.3170188387650512141, 0.3333333333333333703, 0.3170188387650512141, 0.3333333333333333703, 0.3170188387650512141, 0.3333333333333333703, 0.3170188387650512141, 0.3333333333333333703, 0.3170188387650512141, 0.3333333333333333703, 0.3170188387650512141, 0.3333333333333333703, 0.3170188387650512141, 0.3333333333333333703, 0.3170188387650512141, 0.3333333333333333703, 0.3170188387650512141, 0.3333333333333333703, 0.3170188387650512141, 0.3333333333333333703, 0.3170188387650512141, 0.3333333333333333703, 0.3170188387650512141, 0.3333333333333333703, 0.3170188387650512141, 0.3333333333333333703, 0.3170188387650512141, 0.3333333333333333703, 0.3170188387650512141, 0.3333333333333333703, 0.3170188387650512141, 0.3333333333333333703, 0.3170188387650512141, 0.3333333333333333703, 0.3170188387650512141, 0.3333333333333333703, 0.3170188387650512141, 0.3333333333333333703, 0.3170188387650512141, 0.3333333333333333703, 0.3170188387650512141, 0.3333333333333333703, 0.3170188387650512141, 0.3333333333333333703, 0.3170188387650512141, 0.3333333333333333703, 0.3170188387650512141, 0.3333333333333333703, 0.3170188387650512141, 0.3333333333333333703, 0.3170188387650512141, 0.3333333333333333703, 0.3170188387650512141, 0.3333333333333333703, 0.3170188387650512141, 0.3333333333333333703, 0.3170188387650512141, 0.3333333333333333703, 0.3170188387650512141, 0.3333333333333333703, 0.3170188387650512141, 0.3333333333333333703, 0.3170188387650512141, 0.3333333333333333703, 0.3170188387650512141, 0.3333333333333333703, 0.3170188387650512141, 0.3333333333333333703, 0.3170188387650512141, 0.3333333333333333703, 0.3170188387650512141, 0.3333333333333333703, 0.3170188387650512141, 0.3333333333333333703, 0.3170188387650512141, 0.3333333333333333703, 0.3170188387650512141, 0.3333333333333333703, 0.3170188387650512141, 0.3333333333333333703, 0.3170188387650512141, 0.3333333333333333703, 0.3170188387650512141, 0.3333333333333333703, 0.3170188387650512141, 0.3333333333333333703, 0.3170188387650512141, 0.3333333333333333703, 0.3170188387650512141, 0.3333333333333333703, 0.3170188387650512141, 0.3333333333333333703, 0.3170188387650512141, 0.3333333333333333703, 0.3170188387650512141, 0.3333333333333333703, 0.3170188387650512141, 0.3333333333333333703, 0.3170188387650512141, 0.3333333333333333703, 0.3170188387650512141, 0.3333333333333333703, 0.3170188387650512141, 0.3333333333333333703, 0.3170188387650512141, 0.3333333333333333703, 0.3170188387650512141, 0.3333333333333333703, 0.3170188387650512141, 0.3333333333333333703, 0.3170188387650512141, 0.3333333333333333703, 0.3170188387650512141, 0.3333333333333333703, 0.3170188387650512141, 0.3333333333333333703, 0.3170188387650512141, 0.3333333333333333703, 0.3170188387650512141, 0.3333333333333333703, 0.3170188387650512141, 0.3333333333333333703, 0.3170188387650512141, 0.3333333333333333703, 0.3170188387650512141, 0.3333333333333333703, 0.3170188387650512141, 0.3333333333333333703, 0.3170188387650512141, 0.3333333333333333703, 0.3170188387650512141, 0.3333333333333333703, 0.3170188387650512141, 0.3333333333333333703, 0.3170188387650512141, 0.3333333333333333703, 0.3170188387650512141, 0.3333333333333333703, 0.3170188387650512141, 0.3333333333333333703, 0.3170188387650512141, 0.3333333333333333703, 0.3170188387650512141, 0.3333333333333333703, 0.3170188387650512141, 0.3333333333333333703, 0.3170188387650512141, 0.3333333333333333703, 0.3170188387650512141, 0.3333333333333333703, 0.3170188387650512141, 0.3333333333333333703, 0.3170188387650512141, 0.3333333333333333703, 0.3170188387650512141, 0.3333333333333333703, 0.3170188387650512141, 0.3333333333333333703, 0.3170188387650512141, 0.3333333333333333703, 0.3170188387650512141, 0.3333333333333333703, 0.3170188387650512141, 0.3333333333333333703, 0.3170188387650512141, 0.3333333333333333703, 0.3170188387650512141, 0.3333333333333333703, 0.3170188387650512141, 0.3333333333333333703, 0.3170188387650512141, 0.3333333333333333703, 0.3170188387650512141, 0.3333333333333333703, 0.3170188387650512141, 0.3333333333333333703, 0.3170188387650512141, 0.3333333333333333703, 0.3170188387650512141, 0.3333333333333333703, 0.3170188387650512141, 0.3333333333333333703, 0.3170188387650512141, 0.3333333333333333703, 0.3170188387650512141, 0.3333333333333333703, 0.3170188387650512141, 0.3333333333333333703, 0.3170188387650512141, 0.3333333333333333703, 0.3170188387650512141, 0.3333333333333333703, 0.3170188387650512141, 0.3333333333333333703, 0.3170188387650512141, 0.3333333333333333703, 0.3170188387650512141, 0.3333333333333333703, 0.3170188387650512141, 0.3333333333333333703, 0.3170188387650512141, 0.3333333333333333703, 0.3170188387650512141, 0.3333333333333333703, 0.3170188387650512141, 0.3333333333333333703, 0.3170188387650512141, 0.3333333333333333703, 0.3170188387650512141, 0.3333333333333333703, 0.3170188387650512141, 0.3333333333333333703, 0.3170188387650512141, 0.3333333333333333703, 0.3170188387650512141, 0.3333333333333333703, 0.3170188387650512141, 0.3333333333333333703, 0.3170188387650512141, 0.3333333333333333703, 0.3170188387650512141, 0.3333333333333333703, 0.3170188387650512141, 0.3333333333333333703, 0.3170188387650512141, 0.3333333333333333703, 0.3170188387650512141, 0.3333333333333333703, 0.3170188387650512141, 0.3333333333333333703, 0.3170188387650512141, 0.3333333333333333703, 0.3170188387650512141, 0.3333333333333333703, 0.3170188387650512141, 0.3333333333333333703, 0.3170188387650512141, 0.3333333333333333703, 0.3170188387650512141, 0.3333333333333333703, 0.3170188387650512141, 0.3333333333333333703, 0.3170188387650512141, 0.3333333333333333703, 0.3170188387650512141, 0.3333333333333333703, 0.3170188387650512141, 0.3333333333333333703, 0.3170188387650512141, 0.3333333333333333703, 0.3170188387650512141, 0.3333333333333333703, 0.3170188387650512141, 0.3333333333333333703, 0.3170188387650512141, 0.3333333333333333703, 0.3170188387650512141, 0.3333333333333333703, 0.3170188387650512141, 0.3333333333333333703, 0.3170188387650512141, 0.3333333333333333703, 0.3170188387650512141, 0.3333333333333333703, 0.3170188387650512141, 0.3333333333333333703, 0.3170188387650512141, 0.3333333333333333703, 0.3170188387650512141, 0.3333333333333333703, 0.3170188387650512141, 0.3333333333333333703, 0.3170188387650512141, 0.3333333333333333703, 0.3170188387650512141, 0.3333333333333333703, 0.3170188387650512141, 0.3333333333333333703, 0.3170188387650512141, 0.3333333333333333703, 0.3170188387650512141, 0.3333333333333333703, 0.3170188387650512141, 0.3333333333333333703, 0.3170188387650512141, 0.3333333333333333703, 0.3170188387650512141, 0.3333333333333333703, 0.3170188387650512141, 0.3333333333333333703, 0.3170188387650512141, 0.3333333333333333703, 0.3170188387650512141, 0.3333333333333333703, 0.3170188387650512141, 0.3333333333333333703, 0.3170188387650512141, 0.3333333333333333703, 0.3170188387650512141, 0.3333333333333333703, 0.3170188387650512141, 0.3333333333333333703, 0.3170188387650512141, 0.3333333333333333703, 0.3170188387650512141, 0.3333333333333333703, 0.3170188387650512141, 0.3333333333333333703, 0.3170188387650512141, 0.3333333333333333703, 0.3170188387650512141, 0.3333333333333333703, 0.3170188387650512141, 0.3333333333333333703, 0.3170188387650512141, 0.3333333333333333703, 0.3170188387650512141, 0.3333333333333333703, 0.3170188387650512141, 0.3333333333333333703, 0.3170188387650512141, 0.3333333333333333703, 0.3170188387650512141, 0.3333333333333333703, 0.3170188387650512141, 0.3333333333333333703, 0.3170188387650512141, 0.3333333333333333703, 0.3170188387650512141, 0.3333333333333333703, 0.3170188387650512141, 0.3333333333333333703, 0.3170188387650512141, 0.3333333333333333703, 0.3170188387650512141, 0.3333333333333333703, 0.3170188387650512141, 0.3333333333333333703, 0.3170188387650512141, 0.3333333333333333703, 0.3170188387650512141, 0.3333333333333333703, 0.3170188387650512141, 0.3333333333333333703, 0.3170188387650512141, 0.3333333333333333703, 0.3170188387650512141, 0.3333333333333333703, 0.3170188387650512141, 0.3333333333333333703, 0.3170188387650512141, 0.3333333333333333703, 0.3170188387650512141, 0.3333333333333333703, 0.3170188387650512141, 0.3333333333333333703, 0.3170188387650512141, 0.3333333333333333703, 0.3333333333333333703, 0.3333333333333333703),
 ( 0.3333333333333333703, 0.3170188387650512141, 0.3333333333333333703, 0.3170188387650512141, 0.3333333333333333703, 0.3170188387650512141, 0.3333333333333333703, 0.3170188387650512141, 0.3333333333333333703, 0.3170188387650512141, 0.3333333333333333703, 0.3170188387650512141, 0.3333333333333333703, 0.3170188387650512141, 0.3333333333333333703, 0.3170188387650512141, 0.3333333333333333703, 0.3170188387650512141, 0.3333333333333333703, 0.3170188387650512141, 0.3333333333333333703, 0.3170188387650512141, 0.3333333333333333703, 0.3170188387650512141, 0.3333333333333333703, 0.3170188387650512141, 0.3333333333333333703, 0.3170188387650512141, 0.3333333333333333703, 0.3170188387650512141, 0.3333333333333333703, 0.3170188387650512141, 0.3333333333333333703, 0.3170188387650512141, 0.3333333333333333703, 0.3170188387650512141, 0.3333333333333333703, 0.3170188387650512141, 0.3333333333333333703, 0.3170188387650512141, 0.3333333333333333703, 0.3170188387650512141, 0.3333333333333333703, 0.3170188387650512141, 0.3333333333333333703, 0.3170188387650512141, 0.3333333333333333703, 0.3170188387650512141, 0.3333333333333333703, 0.3170188387650512141, 0.3333333333333333703, 0.3170188387650512141, 0.3333333333333333703, 0.3170188387650512141, 0.3333333333333333703, 0.3170188387650512141, 0.3333333333333333703, 0.3170188387650512141, 0.3333333333333333703, 0.3170188387650512141, 0.3333333333333333703, 0.3170188387650512141, 0.3333333333333333703, 0.3170188387650512141, 0.3333333333333333703, 0.3170188387650512141, 0.3333333333333333703, 0.3170188387650512141, 0.3333333333333333703, 0.3170188387650512141, 0.3333333333333333703, 0.3170188387650512141, 0.3333333333333333703, 0.3170188387650512141, 0.3333333333333333703, 0.3170188387650512141, 0.3333333333333333703, 0.3170188387650512141, 0.3333333333333333703, 0.3170188387650512141, 0.3333333333333333703, 0.3170188387650512141, 0.3333333333333333703, 0.3170188387650512141, 0.3333333333333333703, 0.3170188387650512141, 0.3333333333333333703, 0.3170188387650512141, 0.3333333333333333703, 0.3170188387650512141, 0.3333333333333333703, 0.3170188387650512141, 0.3333333333333333703, 0.3170188387650512141, 0.3333333333333333703, 0.3170188387650512141, 0.3333333333333333703, 0.3170188387650512141, 0.3333333333333333703, 0.3170188387650512141, 0.3333333333333333703, 0.3170188387650512141, 0.3333333333333333703, 0.3170188387650512141, 0.3333333333333333703, 0.3170188387650512141, 0.3333333333333333703, 0.3170188387650512141, 0.3333333333333333703, 0.3170188387650512141, 0.3333333333333333703, 0.3170188387650512141, 0.3333333333333333703, 0.3170188387650512141, 0.3333333333333333703, 0.3170188387650512141, 0.3333333333333333703, 0.3170188387650512141, 0.3333333333333333703, 0.3170188387650512141, 0.3333333333333333703, 0.3170188387650512141, 0.3333333333333333703, 0.3170188387650512141, 0.3333333333333333703, 0.3170188387650512141, 0.3333333333333333703, 0.3170188387650512141, 0.3333333333333333703, 0.3170188387650512141, 0.3333333333333333703, 0.3170188387650512141, 0.3333333333333333703, 0.3170188387650512141, 0.3333333333333333703, 0.3170188387650512141, 0.3333333333333333703, 0.3170188387650512141, 0.3333333333333333703, 0.3170188387650512141, 0.3333333333333333703, 0.3170188387650512141, 0.3333333333333333703, 0.3170188387650512141, 0.3333333333333333703, 0.3170188387650512141, 0.3333333333333333703, 0.3170188387650512141, 0.3333333333333333703, 0.3170188387650512141, 0.3333333333333333703, 0.3170188387650512141, 0.3333333333333333703, 0.3170188387650512141, 0.3333333333333333703, 0.3170188387650512141, 0.3333333333333333703, 0.3170188387650512141, 0.3333333333333333703, 0.3170188387650512141, 0.3333333333333333703, 0.3170188387650512141, 0.3333333333333333703, 0.3170188387650512141, 0.3333333333333333703, 0.3170188387650512141, 0.3333333333333333703, 0.3170188387650512141, 0.3333333333333333703, 0.3170188387650512141, 0.3333333333333333703, 0.3170188387650512141, 0.3333333333333333703, 0.3170188387650512141, 0.3333333333333333703, 0.3170188387650512141, 0.3333333333333333703, 0.3170188387650512141, 0.3333333333333333703, 0.3170188387650512141, 0.3333333333333333703, 0.3170188387650512141, 0.3333333333333333703, 0.3170188387650512141, 0.3333333333333333703, 0.3170188387650512141, 0.3333333333333333703, 0.3170188387650512141, 0.3333333333333333703, 0.3170188387650512141, 0.3333333333333333703, 0.3170188387650512141, 0.3333333333333333703, 0.3170188387650512141, 0.3333333333333333703, 0.3170188387650512141, 0.3333333333333333703, 0.3170188387650512141, 0.3333333333333333703, 0.3170188387650512141, 0.3333333333333333703, 0.3170188387650512141, 0.3333333333333333703, 0.3170188387650512141, 0.3333333333333333703, 0.3170188387650512141, 0.3333333333333333703, 0.3170188387650512141, 0.3333333333333333703, 0.3170188387650512141, 0.3333333333333333703, 0.3170188387650512141, 0.3333333333333333703, 0.3170188387650512141, 0.3333333333333333703, 0.3170188387650512141, 0.3333333333333333703, 0.3170188387650512141, 0.3333333333333333703, 0.3170188387650512141, 0.3333333333333333703, 0.3170188387650512141, 0.3333333333333333703, 0.3170188387650512141, 0.3333333333333333703, 0.3170188387650512141, 0.3333333333333333703, 0.3170188387650512141, 0.3333333333333333703, 0.3170188387650512141, 0.3333333333333333703, 0.3170188387650512141, 0.3333333333333333703, 0.3170188387650512141, 0.3333333333333333703, 0.3170188387650512141, 0.3333333333333333703, 0.3170188387650512141, 0.3333333333333333703, 0.3170188387650512141, 0.3333333333333333703, 0.3170188387650512141, 0.3333333333333333703, 0.3170188387650512141, 0.3333333333333333703, 0.3170188387650512141, 0.3333333333333333703, 0.3170188387650512141, 0.3333333333333333703, 0.3170188387650512141, 0.3333333333333333703, 0.3170188387650512141, 0.3333333333333333703, 0.3170188387650512141, 0.3333333333333333703, 0.3170188387650512141, 0.3333333333333333703, 0.3170188387650512141, 0.3333333333333333703, 0.3170188387650512141, 0.3333333333333333703, 0.3170188387650512141, 0.3333333333333333703, 0.3170188387650512141, 0.3333333333333333703, 0.3170188387650512141, 0.3333333333333333703, 0.3170188387650512141, 0.3333333333333333703, 0.3170188387650512141, 0.3333333333333333703, 0.3170188387650512141, 0.3333333333333333703, 0.3170188387650512141, 0.3333333333333333703, 0.3170188387650512141, 0.3333333333333333703, 0.3170188387650512141, 0.3333333333333333703, 0.3170188387650512141, 0.3333333333333333703, 0.3170188387650512141, 0.3333333333333333703, 0.3170188387650512141, 0.3333333333333333703, 0.3170188387650512141, 0.3333333333333333703, 0.3170188387650512141, 0.3333333333333333703, 0.3170188387650512141, 0.3333333333333333703, 0.3170188387650512141, 0.3333333333333333703, 0.3170188387650512141, 0.3333333333333333703, 0.3170188387650512141, 0.3333333333333333703, 0.3170188387650512141, 0.3333333333333333703, 0.3170188387650512141, 0.3333333333333333703, 0.3170188387650512141, 0.3333333333333333703, 0.3170188387650512141, 0.3333333333333333703, 0.3170188387650512141, 0.3333333333333333703, 0.3170188387650512141, 0.3333333333333333703, 0.3170188387650512141, 0.3333333333333333703, 0.3170188387650512141, 0.3333333333333333703, 0.3170188387650512141, 0.3333333333333333703, 0.3170188387650512141, 0.3333333333333333703, 0.3170188387650512141, 0.3333333333333333703, 0.3170188387650512141, 0.3333333333333333703, 0.3170188387650512141, 0.3333333333333333703, 0.3170188387650512141, 0.3333333333333333703, 0.3170188387650512141, 0.3333333333333333703, 0.3170188387650512141, 0.3333333333333333703, 0.3170188387650512141, 0.3333333333333333703, 0.3170188387650512141, 0.3333333333333333703, 0.3170188387650512141, 0.3333333333333333703, 0.3170188387650512141, 0.3333333333333333703, 0.3170188387650512141, 0.3333333333333333703, 0.3170188387650512141, 0.3333333333333333703, 0.3170188387650512141, 0.3333333333333333703, 0.3170188387650512141, 0.3333333333333333703, 0.3170188387650512141, 0.3333333333333333703, 0.3170188387650512141, 0.3333333333333333703, 0.3170188387650512141, 0.3333333333333333703, 0.3170188387650512141, 0.3333333333333333703, 0.3170188387650512141, 0.3333333333333333703, 0.3170188387650512141, 0.3333333333333333703, 0.3170188387650512141, 0.3333333333333333703, 0.3170188387650512141, 0.3333333333333333703, 0.3170188387650512141, 0.3333333333333333703, 0.3170188387650512141, 0.3333333333333333703, 0.3170188387650512141, 0.3333333333333333703, 0.3170188387650512141, 0.3333333333333333703, 0.3170188387650512141, 0.3333333333333333703, 0.3170188387650512141, 0.3333333333333333703, 0.3170188387650512141, 0.3333333333333333703, 0.3170188387650512141, 0.3333333333333333703, 0.3170188387650512141, 0.3333333333333333703, 0.3170188387650512141, 0.3333333333333333703, 0.3170188387650512141, 0.3333333333333333703, 0.3170188387650512141, 0.3333333333333333703, 0.3170188387650512141, 0.3333333333333333703, 0.3170188387650512141, 0.3333333333333333703, 0.3170188387650512141, 0.3333333333333333703, 0.3170188387650512141, 0.3333333333333333703, 0.3170188387650512141, 0.3333333333333333703, 0.3170188387650512141, 0.3333333333333333703, 0.3170188387650512141, 0.3333333333333333703, 0.3170188387650512141, 0.3333333333333333703, 0.3170188387650512141, 0.3333333333333333703, 0.3170188387650512141, 0.3333333333333333703, 0.3170188387650512141, 0.3333333333333333703, 0.3170188387650512141, 0.3333333333333333703, 0.3170188387650512141, 0.3333333333333333703, 0.3170188387650512141, 0.3333333333333333703, 0.3170188387650512141, 0.3333333333333333703, 0.3170188387650512141, 0.3333333333333333703, 0.3170188387650512141, 0.3333333333333333703, 0.3170188387650512141, 0.3333333333333333703, 0.3170188387650512141, 0.3333333333333333703, 0.3170188387650512141, 0.3333333333333333703, 0.3170188387650512141, 0.3333333333333333703, 0.3170188387650512141, 0.3333333333333333703, 0.3170188387650512141, 0.3333333333333333703, 0.3170188387650512141, 0.3333333333333333703, 0.3170188387650512141, 0.3333333333333333703, 0.3170188387650512141, 0.3333333333333333703, 0.3170188387650512141, 0.3333333333333333703, 0.3170188387650512141, 0.3333333333333333703, 0.3170188387650512141, 0.3333333333333333703, 0.3170188387650512141, 0.3333333333333333703, 0.3170188387650512141, 0.3333333333333333703, 0.3170188387650512141, 0.3333333333333333703, 0.3170188387650512141, 0.3333333333333333703, 0.3170188387650512141, 0.3333333333333333703, 0.3170188387650512141, 0.3333333333333333703, 0.3170188387650512141, 0.3333333333333333703, 0.3170188387650512141, 0.3333333333333333703, 0.3170188387650512141, 0.3333333333333333703, 0.3170188387650512141, 0.3333333333333333703, 0.3170188387650512141, 0.3333333333333333703, 0.3170188387650512141, 0.3333333333333333703, 0.3170188387650512141, 0.3333333333333333703, 0.3170188387650512141, 0.3333333333333333703, 0.3170188387650512141, 0.3333333333333333703, 0.3170188387650512141, 0.3333333333333333703, 0.3170188387650512141, 0.3333333333333333703, 0.3170188387650512141, 0.3333333333333333703, 0.3170188387650512141, 0.3333333333333333703, 0.3170188387650512141, 0.3333333333333333703, 0.3170188387650512141, 0.3333333333333333703, 0.3170188387650512141, 0.3333333333333333703, 0.3170188387650512141, 0.3333333333333333703, 0.3170188387650512141, 0.3333333333333333703, 0.3170188387650512141, 0.3333333333333333703, 0.3170188387650512141, 0.3333333333333333703, 0.3170188387650512141, 0.3333333333333333703, 0.3170188387650512141, 0.3333333333333333703, 0.3170188387650512141, 0.3333333333333333703, 0.3170188387650512141, 0.3333333333333333703, 0.3170188387650512141, 0.3333333333333333703, 0.3170188387650512141, 0.3333333333333333703, 0.3170188387650512141, 0.3333333333333333703, 0.3170188387650512141, 0.3333333333333333703, 0.3170188387650512141, 0.3333333333333333703, 0.3170188387650512141, 0.3333333333333333703, 0.3170188387650512141, 0.3333333333333333703, 0.3170188387650512141, 0.3333333333333333703, 0.3170188387650512141, 0.3333333333333333703, 0.3170188387650512141, 0.3333333333333333703, 0.3170188387650512141, 0.3333333333333333703, 0.3170188387650512141, 0.3333333333333333703, 0.3170188387650512141, 0.3333333333333333703, 0.3170188387650512141, 0.3333333333333333703, 0.3170188387650512141, 0.3333333333333333703, 0.3170188387650512141, 0.3333333333333333703, 0.3170188387650512141, 0.3333333333333333703, 0.3170188387650512141, 0.3333333333333333703, 0.3170188387650512141, 0.3333333333333333703, 0.3170188387650512141, 0.3333333333333333703, 0.3170188387650512141, 0.3333333333333333703, 0.3170188387650512141, 0.3333333333333333703, 0.3170188387650512141, 0.3333333333333333703, 0.3170188387650512141, 0.3333333333333333703, 0.3170188387650512141, 0.3333333333333333703, 0.3170188387650512141, 0.3333333333333333703, 0.3170188387650512141, 0.3333333333333333703, 0.3170188387650512141, 0.3333333333333333703, 0.3170188387650512141, 0.3333333333333333703, 0.3170188387650512141, 0.3333333333333333703, 0.3170188387650512141, 0.3333333333333333703, 0.3170188387650512141, 0.3333333333333333703, 0.3170188387650512141, 0.3333333333333333703, 0.3170188387650512141, 0.3333333333333333703, 0.3170188387650512141, 0.3333333333333333703, 0.3170188387650512141, 0.3333333333333333703, 0.3170188387650512141, 0.3333333333333333703, 0.3170188387650512141, 0.3333333333333333703, 0.3170188387650512141, 0.3333333333333333703, 0.3170188387650512141, 0.3333333333333333703, 0.3170188387650512141, 0.3333333333333333703, 0.3170188387650512141, 0.3333333333333333703, 0.3170188387650512141, 0.3333333333333333703, 0.3170188387650512141, 0.3333333333333333703, 0.3170188387650512141, 0.3333333333333333703, 0.3170188387650512141, 0.3333333333333333703, 0.3170188387650512141, 0.3333333333333333703, 0.3170188387650512141, 0.3333333333333333703, 0.3170188387650512141, 0.3333333333333333703, 0.3170188387650512141, 0.3333333333333333703, 0.3170188387650512141, 0.3333333333333333703, 0.3170188387650512141, 0.3333333333333333703, 0.3170188387650512141, 0.3333333333333333703, 0.3170188387650512141, 0.3333333333333333703, 0.3170188387650512141, 0.3333333333333333703, 0.3170188387650512141, 0.3333333333333333703, 0.3170188387650512141, 0.3333333333333333703, 0.3170188387650512141, 0.3333333333333333703, 0.3170188387650512141, 0.3333333333333333703, 0.3170188387650512141, 0.3333333333333333703, 0.3170188387650512141, 0.3333333333333333703, 0.3170188387650512141, 0.3333333333333333703, 0.3170188387650512141, 0.3333333333333333703, 0.3170188387650512141, 0.3333333333333333703, 0.3170188387650512141, 0.3333333333333333703, 0.3170188387650512141, 0.3333333333333333703, 0.3170188387650512141, 0.3333333333333333703, 0.3170188387650512141, 0.3333333333333333703, 0.3170188387650512141, 0.3333333333333333703, 0.3170188387650512141, 0.3333333333333333703, 0.3170188387650512141, 0.3333333333333333703, 0.3170188387650512141, 0.3333333333333333703, 0.3170188387650512141, 0.3333333333333333703, 0.3170188387650512141, 0.3333333333333333703, 0.3170188387650512141, 0.3333333333333333703, 0.3170188387650512141, 0.3333333333333333703, 0.3170188387650512141, 0.3333333333333333703, 0.3170188387650512141, 0.3333333333333333703, 0.3170188387650512141, 0.3333333333333333703, 0.3170188387650512141, 0.3333333333333333703, 0.3170188387650512141, 0.3333333333333333703, 0.3170188387650512141, 0.3333333333333333703, 0.3170188387650512141, 0.3333333333333333703, 0.3170188387650512141, 0.3333333333333333703, 0.3170188387650512141, 0.3333333333333333703, 0.3170188387650512141, 0.3333333333333333703, 0.3170188387650512141, 0.3333333333333333703, 0.3170188387650512141, 0.3333333333333333703, 0.3170188387650512141, 0.3333333333333333703, 0.3170188387650512141, 0.3333333333333333703, 0.3170188387650512141, 0.3333333333333333703, 0.3170188387650512141, 0.3333333333333333703, 0.3170188387650512141, 0.3333333333333333703, 0.3170188387650512141, 0.3333333333333333703, 0.3333333333333333703, 0.3333333333333333703),
 ( 1.000000000000000000, 0.9510565162951535312, 1.000000000000000000, 0.9510565162951535312, 1.000000000000000000, 0.9510565162951535312, 1.000000000000000000, 0.9510565162951535312, 1.000000000000000000, 0.9510565162951535312, 1.000000000000000000, 0.9510565162951535312, 1.000000000000000000, 0.9510565162951535312, 1.000000000000000000, 0.9510565162951535312, 1.000000000000000000, 0.9510565162951535312, 1.000000000000000000, 0.9510565162951535312, 1.000000000000000000, 0.9510565162951535312, 1.000000000000000000, 0.9510565162951535312, 1.000000000000000000, 0.9510565162951535312, 1.000000000000000000, 0.9510565162951535312, 1.000000000000000000, 0.9510565162951535312, 1.000000000000000000, 0.9510565162951535312, 1.000000000000000000, 0.9510565162951535312, 1.000000000000000000, 0.9510565162951535312, 1.000000000000000000, 0.9510565162951535312, 1.000000000000000000, 0.9510565162951535312, 1.000000000000000000, 0.9510565162951535312, 1.000000000000000000, 0.9510565162951535312, 1.000000000000000000, 0.9510565162951535312, 1.000000000000000000, 0.9510565162951535312, 1.000000000000000000, 0.9510565162951535312, 1.000000000000000000, 0.9510565162951535312, 1.000000000000000000, 0.9510565162951535312, 1.000000000000000000, 0.9510565162951535312, 1.000000000000000000, 0.9510565162951535312, 1.000000000000000000, 0.9510565162951535312, 1.000000000000000000, 0.9510565162951535312, 1.000000000000000000, 0.9510565162951535312, 1.000000000000000000, 0.9510565162951535312, 1.000000000000000000, 0.9510565162951535312, 1.000000000000000000, 0.9510565162951535312, 1.000000000000000000, 0.9510565162951535312, 1.000000000000000000, 0.9510565162951535312, 1.000000000000000000, 0.9510565162951535312, 1.000000000000000000, 0.9510565162951535312, 1.000000000000000000, 0.9510565162951535312, 1.000000000000000000, 0.9510565162951535312, 1.000000000000000000, 0.9510565162951535312, 1.000000000000000000, 0.9510565162951535312, 1.000000000000000000, 0.9510565162951535312, 1.000000000000000000, 0.9510565162951535312, 1.000000000000000000, 0.9510565162951535312, 1.000000000000000000, 0.9510565162951535312, 1.000000000000000000, 0.9510565162951535312, 1.000000000000000000, 0.9510565162951535312, 1.000000000000000000, 0.9510565162951535312, 1.000000000000000000, 0.9510565162951535312, 1.000000000000000000, 0.9510565162951535312, 1.000000000000000000, 0.9510565162951535312, 1.000000000000000000, 0.9510565162951535312, 1.000000000000000000, 0.9510565162951535312, 1.000000000000000000, 0.9510565162951535312, 1.000000000000000000, 0.9510565162951535312, 1.000000000000000000, 0.9510565162951535312, 1.000000000000000000, 0.9510565162951535312, 1.000000000000000000, 0.9510565162951535312, 1.000000000000000000, 0.9510565162951535312, 1.000000000000000000, 0.9510565162951535312, 1.000000000000000000, 0.9510565162951535312, 1.000000000000000000, 0.9510565162951535312, 1.000000000000000000, 0.9510565162951535312, 1.000000000000000000, 0.9510565162951535312, 1.000000000000000000, 0.9510565162951535312, 1.000000000000000000, 0.9510565162951535312, 1.000000000000000000, 0.9510565162951535312, 1.000000000000000000, 0.9510565162951535312, 1.000000000000000000, 0.9510565162951535312, 1.000000000000000000, 0.9510565162951535312, 1.000000000000000000, 0.9510565162951535312, 1.000000000000000000, 0.9510565162951535312, 1.000000000000000000, 0.9510565162951535312, 1.000000000000000000, 0.9510565162951535312, 1.000000000000000000, 0.9510565162951535312, 1.000000000000000000, 0.9510565162951535312, 1.000000000000000000, 0.9510565162951535312, 1.000000000000000000, 0.9510565162951535312, 1.000000000000000000, 0.9510565162951535312, 1.000000000000000000, 0.9510565162951535312, 1.000000000000000000, 0.9510565162951535312, 1.000000000000000000, 0.9510565162951535312, 1.000000000000000000, 0.9510565162951535312, 1.000000000000000000, 0.9510565162951535312, 1.000000000000000000, 0.9510565162951535312, 1.000000000000000000, 0.9510565162951535312, 1.000000000000000000, 0.9510565162951535312, 1.000000000000000000, 0.9510565162951535312, 1.000000000000000000, 0.9510565162951535312, 1.000000000000000000, 0.9510565162951535312, 1.000000000000000000, 0.9510565162951535312, 1.000000000000000000, 0.9510565162951535312, 1.000000000000000000, 0.9510565162951535312, 1.000000000000000000, 0.9510565162951535312, 1.000000000000000000, 0.9510565162951535312, 1.000000000000000000, 0.9510565162951535312, 1.000000000000000000, 0.9510565162951535312, 1.000000000000000000, 0.9510565162951535312, 1.000000000000000000, 0.9510565162951535312, 1.000000000000000000, 0.9510565162951535312, 1.000000000000000000, 0.9510565162951535312, 1.000000000000000000, 0.9510565162951535312, 1.000000000000000000, 0.9510565162951535312, 1.000000000000000000, 0.9510565162951535312, 1.000000000000000000, 0.9510565162951535312, 1.000000000000000000, 0.9510565162951535312, 1.000000000000000000, 0.9510565162951535312, 1.000000000000000000, 0.9510565162951535312, 1.000000000000000000, 0.9510565162951535312, 1.000000000000000000, 0.9510565162951535312, 1.000000000000000000, 0.9510565162951535312, 1.000000000000000000, 0.9510565162951535312, 1.000000000000000000, 0.9510565162951535312, 1.000000000000000000, 0.9510565162951535312, 1.000000000000000000, 0.9510565162951535312, 1.000000000000000000, 0.9510565162951535312, 1.000000000000000000, 0.9510565162951535312, 1.000000000000000000, 0.9510565162951535312, 1.000000000000000000, 0.9510565162951535312, 1.000000000000000000, 0.9510565162951535312, 1.000000000000000000, 0.9510565162951535312, 1.000000000000000000, 0.9510565162951535312, 1.000000000000000000, 0.9510565162951535312, 1.000000000000000000, 0.9510565162951535312, 1.000000000000000000, 0.9510565162951535312, 1.000000000000000000, 0.9510565162951535312, 1.000000000000000000, 0.9510565162951535312, 1.000000000000000000, 0.9510565162951535312, 1.000000000000000000, 0.9510565162951535312, 1.000000000000000000, 0.9510565162951535312, 1.000000000000000000, 0.9510565162951535312, 1.000000000000000000, 0.9510565162951535312, 1.000000000000000000, 0.9510565162951535312, 1.000000000000000000, 0.9510565162951535312, 1.000000000000000000, 0.9510565162951535312, 1.000000000000000000, 0.9510565162951535312, 1.000000000000000000, 0.9510565162951535312, 1.000000000000000000, 0.9510565162951535312, 1.000000000000000000, 0.9510565162951535312, 1.000000000000000000, 0.9510565162951535312, 1.000000000000000000, 0.9510565162951535312, 1.000000000000000000, 0.9510565162951535312, 1.000000000000000000, 0.9510565162951535312, 1.000000000000000000, 0.9510565162951535312, 1.000000000000000000, 0.9510565162951535312, 1.000000000000000000, 0.9510565162951535312, 1.000000000000000000, 0.9510565162951535312, 1.000000000000000000, 0.9510565162951535312, 1.000000000000000000, 0.9510565162951535312, 1.000000000000000000, 0.9510565162951535312, 1.000000000000000000, 0.9510565162951535312, 1.000000000000000000, 0.9510565162951535312, 1.000000000000000000, 0.9510565162951535312, 1.000000000000000000, 0.9510565162951535312, 1.000000000000000000, 0.9510565162951535312, 1.000000000000000000, 0.9510565162951535312, 1.000000000000000000, 0.9510565162951535312, 1.000000000000000000, 0.9510565162951535312, 1.000000000000000000, 0.9510565162951535312, 1.000000000000000000, 0.9510565162951535312, 1.000000000000000000, 0.9510565162951535312, 1.000000000000000000, 0.9510565162951535312, 1.000000000000000000, 0.9510565162951535312, 1.000000000000000000, 0.9510565162951535312, 1.000000000000000000, 0.9510565162951535312, 1.000000000000000000, 0.9510565162951535312, 1.000000000000000000, 0.9510565162951535312, 1.000000000000000000, 0.9510565162951535312, 1.000000000000000000, 0.9510565162951535312, 1.000000000000000000, 0.9510565162951535312, 1.000000000000000000, 0.9510565162951535312, 1.000000000000000000, 0.9510565162951535312, 1.000000000000000000, 0.9510565162951535312, 1.000000000000000000, 0.9510565162951535312, 1.000000000000000000, 0.9510565162951535312, 1.000000000000000000, 0.9510565162951535312, 1.000000000000000000, 0.9510565162951535312, 1.000000000000000000, 0.9510565162951535312, 1.000000000000000000, 0.9510565162951535312, 1.000000000000000000, 0.9510565162951535312, 1.000000000000000000, 0.9510565162951535312, 1.000000000000000000, 0.9510565162951535312, 1.000000000000000000, 0.9510565162951535312, 1.000000000000000000, 0.9510565162951535312, 1.000000000000000000, 0.9510565162951535312, 1.000000000000000000, 0.9510565162951535312, 1.000000000000000000, 0.9510565162951535312, 1.000000000000000000, 0.9510565162951535312, 1.000000000000000000, 0.9510565162951535312, 1.000000000000000000, 0.9510565162951535312, 1.000000000000000000, 0.9510565162951535312, 1.000000000000000000, 0.9510565162951535312, 1.000000000000000000, 0.9510565162951535312, 1.000000000000000000, 0.9510565162951535312, 1.000000000000000000, 0.9510565162951535312, 1.000000000000000000, 0.9510565162951535312, 1.000000000000000000, 0.9510565162951535312, 1.000000000000000000, 0.9510565162951535312, 1.000000000000000000, 0.9510565162951535312, 1.000000000000000000, 0.9510565162951535312, 1.000000000000000000, 0.9510565162951535312, 1.000000000000000000, 0.9510565162951535312, 1.000000000000000000, 0.9510565162951535312, 1.000000000000000000, 0.9510565162951535312, 1.000000000000000000, 0.9510565162951535312, 1.000000000000000000, 0.9510565162951535312, 1.000000000000000000, 0.9510565162951535312, 1.000000000000000000, 0.9510565162951535312, 1.000000000000000000, 0.9510565162951535312, 1.000000000000000000, 0.9510565162951535312, 1.000000000000000000, 0.9510565162951535312, 1.000000000000000000, 0.9510565162951535312, 1.000000000000000000, 0.9510565162951535312, 1.000000000000000000, 0.9510565162951535312, 1.000000000000000000, 0.9510565162951535312, 1.000000000000000000, 0.9510565162951535312, 1.000000000000000000, 0.9510565162951535312, 1.000000000000000000, 0.9510565162951535312, 1.000000000000000000, 0.9510565162951535312, 1.000000000000000000, 0.9510565162951535312, 1.000000000000000000, 0.9510565162951535312, 1.000000000000000000, 0.9510565162951535312, 1.000000000000000000, 0.9510565162951535312, 1.000000000000000000, 0.9510565162951535312, 1.000000000000000000, 0.9510565162951535312, 1.000000000000000000, 0.9510565162951535312, 1.000000000000000000, 0.9510565162951535312, 1.000000000000000000, 0.9510565162951535312, 1.000000000000000000, 0.9510565162951535312, 1.000000000000000000, 0.9510565162951535312, 1.000000000000000000, 0.9510565162951535312, 1.000000000000000000, 0.9510565162951535312, 1.000000000000000000, 0.9510565162951535312, 1.000000000000000000, 0.9510565162951535312, 1.000000000000000000, 0.9510565162951535312, 1.000000000000000000, 0.9510565162951535312, 1.000000000000000000, 0.9510565162951535312, 1.000000000000000000, 0.9510565162951535312, 1.000000000000000000, 0.9510565162951535312, 1.000000000000000000, 0.9510565162951535312, 1.000000000000000000, 0.9510565162951535312, 1.000000000000000000, 0.9510565162951535312, 1.000000000000000000, 0.9510565162951535312, 1.000000000000000000, 0.9510565162951535312, 1.000000000000000000, 0.9510565162951535312, 1.000000000000000000, 0.9510565162951535312, 1.000000000000000000, 0.9510565162951535312, 1.000000000000000000, 0.9510565162951535312, 1.000000000000000000, 0.9510565162951535312, 1.000000000000000000, 0.9510565162951535312, 1.000000000000000000, 0.9510565162951535312, 1.000000000000000000, 0.9510565162951535312, 1.000000000000000000, 0.9510565162951535312, 1.000000000000000000, 0.9510565162951535312, 1.000000000000000000, 0.9510565162951535312, 1.000000000000000000, 0.9510565162951535312, 1.000000000000000000, 0.9510565162951535312, 1.000000000000000000, 0.9510565162951535312, 1.000000000000000000, 0.9510565162951535312, 1.000000000000000000, 0.9510565162951535312, 1.000000000000000000, 0.9510565162951535312, 1.000000000000000000, 0.9510565162951535312, 1.000000000000000000, 0.9510565162951535312, 1.000000000000000000, 0.9510565162951535312, 1.000000000000000000, 0.9510565162951535312, 1.000000000000000000, 0.9510565162951535312, 1.000000000000000000, 0.9510565162951535312, 1.000000000000000000, 0.9510565162951535312, 1.000000000000000000, 0.9510565162951535312, 1.000000000000000000, 0.9510565162951535312, 1.000000000000000000, 0.9510565162951535312, 1.000000000000000000, 0.9510565162951535312, 1.000000000000000000, 0.9510565162951535312, 1.000000000000000000, 0.9510565162951535312, 1.000000000000000000, 0.9510565162951535312, 1.000000000000000000, 0.9510565162951535312, 1.000000000000000000, 0.9510565162951535312, 1.000000000000000000, 0.9510565162951535312, 1.000000000000000000, 0.9510565162951535312, 1.000000000000000000, 0.9510565162951535312, 1.000000000000000000, 0.9510565162951535312, 1.000000000000000000, 0.9510565162951535312, 1.000000000000000000, 0.9510565162951535312, 1.000000000000000000, 0.9510565162951535312, 1.000000000000000000, 0.9510565162951535312, 1.000000000000000000, 0.9510565162951535312, 1.000000000000000000, 0.9510565162951535312, 1.000000000000000000, 0.9510565162951535312, 1.000000000000000000, 0.9510565162951535312, 1.000000000000000000, 0.9510565162951535312, 1.000000000000000000, 0.9510565162951535312, 1.000000000000000000, 0.9510565162951535312, 1.000000000000000000, 0.9510565162951535312, 1.000000000000000000, 0.9510565162951535312, 1.000000000000000000, 0.9510565162951535312, 1.000000000000000000, 0.9510565162951535312, 1.000000000000000000, 0.9510565162951535312, 1.000000000000000000, 0.9510565162951535312, 1.000000000000000000, 0.9510565162951535312, 1.000000000000000000, 0.9510565162951535312, 1.000000000000000000, 0.9510565162951535312, 1.000000000000000000, 0.9510565162951535312, 1.000000000000000000, 0.9510565162951535312, 1.000000000000000000, 0.9510565162951535312, 1.000000000000000000, 0.9510565162951535312, 1.000000000000000000, 0.9510565162951535312, 1.000000000000000000, 0.9510565162951535312, 1.000000000000000000, 0.9510565162951535312, 1.000000000000000000, 0.9510565162951535312, 1.000000000000000000, 0.9510565162951535312, 1.000000000000000000, 0.9510565162951535312, 1.000000000000000000, 0.9510565162951535312, 1.000000000000000000, 0.9510565162951535312, 1.000000000000000000, 0.9510565162951535312, 1.000000000000000000, 0.9510565162951535312, 1.000000000000000000, 0.9510565162951535312, 1.000000000000000000, 0.9510565162951535312, 1.000000000000000000, 0.9510565162951535312, 1.000000000000000000, 0.9510565162951535312, 1.000000000000000000, 0.9510565162951535312, 1.000000000000000000, 0.9510565162951535312, 1.000000000000000000, 0.9510565162951535312, 1.000000000000000000, 0.9510565162951535312, 1.000000000000000000, 0.9510565162951535312, 1.000000000000000000, 0.9510565162951535312, 1.000000000000000000, 0.9510565162951535312, 1.000000000000000000, 0.9510565162951535312, 1.000000000000000000, 0.9510565162951535312, 1.000000000000000000, 0.9510565162951535312, 1.000000000000000000, 0.9510565162951535312, 1.000000000000000000, 0.9510565162951535312, 1.000000000000000000, 0.9510565162951535312, 1.000000000000000000, 0.9510565162951535312, 1.000000000000000000, 0.9510565162951535312, 1.000000000000000000, 0.9510565162951535312, 1.000000000000000000, 0.9510565162951535312, 1.000000000000000000, 0.9510565162951535312, 1.000000000000000000, 0.9510565162951535312, 1.000000000000000000, 0.9510565162951535312, 1.000000000000000000, 0.9510565162951535312, 1.000000000000000000, 0.9510565162951535312, 1.000000000000000000, 0.9510565162951535312, 1.000000000000000000, 0.9510565162951535312, 1.000000000000000000, 1.000000000000000000, 1.000000000000000000) ) ) 
 REPRESENTATION_ITEM ( '' )  SURFACE ( )  );
#30712 = ORIENTED_EDGE ( 'NONE', *, *, #3126, .T. ) ;
#30713 = CARTESIAN_POINT ( 'NONE',  ( 6.500168698208244500, 202.3363017425938324, 22.29886208192143826 ) ) ;
#30714 =( GEOMETRIC_REPRESENTATION_CONTEXT ( 3 ) GLOBAL_UNCERTAINTY_ASSIGNED_CONTEXT ( ( #28815 ) ) GLOBAL_UNIT_ASSIGNED_CONTEXT ( ( #20951, #21605, #174 ) ) REPRESENTATION_CONTEXT ( 'NONE', 'WORKASPACE' ) );
#30715 = LINE ( 'NONE', #1576, #26837 ) ;
#30716 = ORIENTED_EDGE ( 'NONE', *, *, #14160, .F. ) ;
#30717 = CARTESIAN_POINT ( 'NONE',  ( 6.444103211791042618, 202.2591342207267644, -0.6988620819214341751 ) ) ;
#30718 = CARTESIAN_POINT ( 'NONE',  ( -11.98450388067341876, 203.0532714938636047, 86.34886208192143897 ) ) ;
#30719 = CARTESIAN_POINT ( 'NONE',  ( 35.67499999726880588, 168.2552932293087906, -9.630534252274387086 ) ) ;
#30720 = VERTEX_POINT ( 'NONE', #29879 ) ;
#30721 = CARTESIAN_POINT ( 'NONE',  ( 46.52499999726881441, 140.1801316387863778, 4.815267126137185549 ) ) ;
#30722 = CARTESIAN_POINT ( 'NONE',  ( 122.3560003530527638, 4.587378538859887556, 35.00001199999999812 ) ) ;
#30723 = CARTESIAN_POINT ( 'NONE',  ( -6.139770520408369237, 215.5359834540460042, 0.9511379180785658471 ) ) ;
#30724 = CARTESIAN_POINT ( 'NONE',  ( -3.044812012439970683, 197.4746971517856196, 73.89886208192143613 ) ) ;
#30725 = CARTESIAN_POINT ( 'NONE',  ( 49.87499999726880162, 171.3844434931184253, -7.942151717890132712E-15 ) ) ;
#30726 = CARTESIAN_POINT ( 'NONE',  ( -67.50001199999996970, 146.4804385394329245, 14.75313718340011881 ) ) ;
#30727 = CARTESIAN_POINT ( 'NONE',  ( 6.220909254589536808, 215.4770327129947702, 13.55113791807856849 ) ) ;
#30728 = CARTESIAN_POINT ( 'NONE',  ( -19.55945325266600676, -20.46160920480082979, -0.4491195576436824433 ) ) ;
#30729 = CARTESIAN_POINT ( 'NONE',  ( 68.90000000000000568, 168.7903194862797420, -4.480746418436745593 ) ) ;
#30730 = CARTESIAN_POINT ( 'NONE',  ( 6.220909254589536808, 215.4770327129947702, 88.55113791807853829 ) ) ;
#30731 = CARTESIAN_POINT ( 'NONE',  ( 115.4999999999999858, 126.0449016395812691, -103.9084171661922227 ) ) ;
#30732 = CARTESIAN_POINT ( 'NONE',  ( 3.135527875058820690, 216.4958274776887492, 73.40113791807857524 ) ) ;
#30733 = LINE ( 'NONE', #9947, #16176 ) ;
#30734 = DIRECTION ( 'NONE',  ( -1.000000000000000000, 0.000000000000000000, 0.000000000000000000 ) ) ;
#30735 = CARTESIAN_POINT ( 'NONE',  ( -9.736236675708031640, 214.0148392665760753, 89.79886208192142760 ) ) ;
#30736 = EDGE_CURVE ( 'NONE', #18219, #19921, #22258, .T. ) ;
#30737 = CARTESIAN_POINT ( 'NONE',  ( 61.42499999726882010, 168.2552932293087906, -9.630534252274385310 ) ) ;
#30739 = VERTEX_POINT ( 'NONE', #14375 ) ;
#30738 = CARTESIAN_POINT ( 'NONE',  ( 6.220909254589536808, 215.4770327129947987, 25.55113791807857027 ) ) ;
#30740 = CARTESIAN_POINT ( 'NONE',  ( -60.66959905230670103, 194.9806057094332346, 1.252942659870247555 ) ) ;
#30741 = CARTESIAN_POINT ( 'NONE',  ( 36.79999999453762882, 163.5228861582408797, 11.73074641843673049 ) ) ;
#30742 = CARTESIAN_POINT ( 'NONE',  ( -7.456977232089304408, 196.8216656703010301, 99.05113791807858092 ) ) ;
#30743 = PLANE ( 'NONE',  #8833 ) ;
#30744 = ORIENTED_EDGE ( 'NONE', *, *, #20214, .T. ) ;
#30745 = CARTESIAN_POINT ( 'NONE',  ( -10.01549611932659545, 210.2015048109875011, 83.64886208192145034 ) ) ;
#30746 = CARTESIAN_POINT ( 'NONE',  ( -11.98450388067341876, 203.0532714938636047, 20.34886208192143542 ) ) ;
#30747 = CARTESIAN_POINT ( 'NONE',  ( 104.9083388212530537, 155.0000000000000000, 0.000000000000000000 ) ) ;
#30748 = CARTESIAN_POINT ( 'NONE',  ( -8.062137200540920645, 212.9164362838581894, 30.80113791807856671 ) ) ;
#30749 = CARTESIAN_POINT ( 'NONE',  ( 66.58867513459482268, 146.1832212156128890, -12.13525491562423042 ) ) ;
#30750 = CARTESIAN_POINT ( 'NONE',  ( 6.220909254589681581, 198.5229672870052582, 100.4488620819214475 ) ) ;
#30751 = LINE ( 'NONE', #9454, #10524 ) ;
#30752 = ORIENTED_EDGE ( 'NONE', *, *, #19153, .T. ) ;
#30753 = CARTESIAN_POINT ( 'NONE',  ( 8.000000000000000000, 0.000000000000000000, 6.500000000000000000 ) ) ;
#30754 = CARTESIAN_POINT ( 'NONE',  ( 4.984841277089891776, 200.2242689037093726, 82.44886208192144750 ) ) ;
#30755 = ORIENTED_EDGE ( 'NONE', *, *, #17013, .F. ) ;
#30756 = CARTESIAN_POINT ( 'NONE',  ( 38.78867513459481842, 155.0000000000000000, -15.00000000000002487 ) ) ;
#30757 = ORIENTED_EDGE ( 'NONE', *, *, #12320, .F. ) ;
#30758 = CARTESIAN_POINT ( 'NONE',  ( 80.71132485994280614, 155.0000000000000000, 15.00000000000001243 ) ) ;
#30759 = CARTESIAN_POINT ( 'NONE',  ( -2.426778023690262742, 214.6231898156240163, 64.10113791807857808 ) ) ;
#30760 =( BOUNDED_CURVE ( )  B_SPLINE_CURVE ( 2, ( #28116, #7350, #14828, #25058, #30173, #9724, #30339, #32547, #14488, #27774, #15172 ),
 .UNSPECIFIED., .F., .T. ) 
 B_SPLINE_CURVE_WITH_KNOTS ( ( 3, 2, 2, 2, 2, 3 ),
 ( 0.3035714285714283256, 0.3071428571428568843, 0.3107142857142855541, 0.3142857142857141128, 0.3178571428571426716, 0.3214285714285712303 ),
 .UNSPECIFIED. ) 
 CURVE ( )  GEOMETRIC_REPRESENTATION_ITEM ( )  RATIONAL_B_SPLINE_CURVE ( ( 1.000000000000002220, 0.9510565162951510887, 1.000000000000000000, 0.9510565162951534202, 1.000000000000000000, 0.9510565162951534202, 1.000000000000000000, 0.9510565162951534202, 1.000000000000000000, 0.9510565162951557516, 0.9999999999999976685 ) ) 
 REPRESENTATION_ITEM ( '' )  );
#30761 = ADVANCED_FACE ( 'NONE', ( #14530 ), #32591, .F. ) ;
#30762 = CARTESIAN_POINT ( 'NONE',  ( 80.02499999726882152, 160.0630714827496206, 15.58253174999999402 ) ) ;
#30763 = DIRECTION ( 'NONE',  ( 0.000000000000000000, -0.4999999999999990563, 0.8660254037844391517 ) ) ;
#30764 = CARTESIAN_POINT ( 'NONE',  ( -4.984841277089726574, 200.2242689037092305, 78.05113791807858092 ) ) ;
#30765 = CARTESIAN_POINT ( 'NONE',  ( -31.74999999999995737, 0.000000000000000000, 2.000000000000000888 ) ) ;
#30766 = CARTESIAN_POINT ( 'NONE',  ( 38.69999999999999574, 163.5228861582408797, -11.73074641843674470 ) ) ;
#30767 = CARTESIAN_POINT ( 'NONE',  ( 2.426778023690075337, 214.6231898156240447, 66.39886208192143613 ) ) ;
#30768 = ADVANCED_FACE ( 'NONE', ( #16916 ), #6403, .F. ) ;
#30769 = DIRECTION ( 'NONE',  ( -1.000000000000000000, 0.000000000000000000, 0.000000000000000000 ) ) ;
#30770 = FACE_OUTER_BOUND ( 'NONE', #16525, .T. ) ;
#30771 = CARTESIAN_POINT ( 'NONE',  ( 0.000000000000000000, 0.000000000000000000, 0.000000000000000000 ) ) ;
#30772 = CARTESIAN_POINT ( 'NONE',  ( 57.62499999726880873, 171.3844434931184253, -7.942151717890134290E-15 ) ) ;
#30773 = CARTESIAN_POINT ( 'NONE',  ( 70.67499999726881299, 141.7447067706911810, 9.630534252274376428 ) ) ;
#30774 = CARTESIAN_POINT ( 'NONE',  ( -12.01549611932652972, 203.1486557965464499, 69.35113791807857808 ) ) ;
#30775 = CARTESIAN_POINT ( 'NONE',  ( 127.5000000000000000, 155.0000000000000000, -6.938893903907228378E-15 ) ) ;
#30776 = CARTESIAN_POINT ( 'NONE',  ( -9.736236675707914401, 199.9851607334237542, 12.20113791807856707 ) ) ;
#30777 = CARTESIAN_POINT ( 'NONE',  ( 8.118202686958039038, 212.8392687619912635, 88.70113791807857240 ) ) ;
#30778 = ADVANCED_FACE ( 'NONE', ( #9083 ), #24931, .T. ) ;
#30779 = CARTESIAN_POINT ( 'NONE',  ( 11.98450388067341876, 210.9467285061363953, 42.84886208192143187 ) ) ;
#30780 = CARTESIAN_POINT ( 'NONE',  ( 8.118202686958138514, 201.1607312380088501, 61.29886208192143471 ) ) ;
#30781 = PLANE ( 'NONE',  #21540 ) ;
#30782 = CARTESIAN_POINT ( 'NONE',  ( 0.05014649552807549926, 219.6175466908591716, 94.25113791807859798 ) ) ;
#30783 = DIRECTION ( 'NONE',  ( -2.312964634635740985E-16, 1.000000000000000000, 0.000000000000000000 ) ) ;
#30784 = CARTESIAN_POINT ( 'NONE',  ( -8.118202686958039038, 201.1607312380087080, 3.201137918078566180 ) ) ;
#30785 = CARTESIAN_POINT ( 'NONE',  ( -9.984503880673420539, 203.7031108863293980, 71.34886208192142476 ) ) ;
#30786 = DIRECTION ( 'NONE',  ( 0.000000000000000000, 0.000000000000000000, 1.000000000000000000 ) ) ;
#30787 = ORIENTED_EDGE ( 'NONE', *, *, #1411, .T. ) ;
#30788 = CARTESIAN_POINT ( 'NONE',  ( -12.01549611932659722, 210.8513442034533227, 68.64886208192142192 ) ) ;
#30789 = CARTESIAN_POINT ( 'NONE',  ( -0.05014649552810635652, 196.4853777576173002, 92.75113791807858377 ) ) ;
#30790 = EDGE_LOOP ( 'NONE', ( #1648, #4383, #3087 ) ) ;
#30791 = CARTESIAN_POINT ( 'NONE',  ( 78.77499999726880731, 140.1801316387863778, 4.815267126137185549 ) ) ;
#30792 = CARTESIAN_POINT ( 'NONE',  ( 0.05014649552828262524, 198.5883022060938572, 52.74886208192144466 ) ) ;
#30793 = EDGE_LOOP ( 'NONE', ( #2879, #22316, #3805, #23750 ) ) ;
#30794 = EDGE_CURVE ( 'NONE', #16934, #854, #23893, .T. ) ;
#30795 = CARTESIAN_POINT ( 'NONE',  ( 69.32499999726881867, 164.1591823560292198, -12.60653300113719766 ) ) ;
#30796 = CARTESIAN_POINT ( 'NONE',  ( 6.500000000000000888, 1.333904739168207065, -6.094327662196326933 ) ) ;
#30797 = CARTESIAN_POINT ( 'NONE',  ( -58.17468396801123731, 194.9227987135369062, -2.484183799773476142 ) ) ;
#30798 = EDGE_CURVE ( 'NONE', #33389, #31608, #33101, .T. ) ;
#30799 = CARTESIAN_POINT ( 'NONE',  ( 66.12499999726881583, 155.0000000000000000, 15.58253174999999402 ) ) ;
#30800 = DIRECTION ( 'NONE',  ( 0.000000000000000000, 0.000000000000000000, 1.000000000000000000 ) ) ;
#30801 = CARTESIAN_POINT ( 'NONE',  ( -8.062137200540822946, 201.0835637161416400, 50.19886208192144039 ) ) ;
#30802 = VERTEX_POINT ( 'NONE', #22365 ) ;
#30803 = CARTESIAN_POINT ( 'NONE',  ( 13.75000000000002487, 23.81569860407205397, -18.00000000000000000 ) ) ;
#30804 = SURFACE_STYLE_USAGE ( .BOTH. , #33358 ) ;
#30805 = CARTESIAN_POINT ( 'NONE',  ( 57.78867513459481842, 155.0000000000000000, 15.00000000000001243 ) ) ;
#30806 = CARTESIAN_POINT ( 'NONE',  ( 0.000000000000000000, 0.000000000000000000, -9.226681596905677907 ) ) ;
#30807 = CARTESIAN_POINT ( 'NONE',  ( -4.984841277089891776, 213.7757310962905990, 23.94886208192143684 ) ) ;
#30808 = CARTESIAN_POINT ( 'NONE',  ( -6.139770520408369237, 215.5359834540460042, 66.95113791807858661 ) ) ;
#30809 = CYLINDRICAL_SURFACE ( 'NONE', #16929, 100.0000000000000000 ) ;
#30810 = CARTESIAN_POINT ( 'NONE',  ( -6.220909254589537696, 198.5229672870051161, 54.05113791807856671 ) ) ;
#30811 = CARTESIAN_POINT ( 'NONE',  ( 10.01549611932653860, 210.2015048109876716, 25.85113791807856742 ) ) ;
#30812 = CARTESIAN_POINT ( 'NONE',  ( -0.05014649552807731031, 198.5883022060938572, 2.751137918078566003 ) ) ;
#30813 = CARTESIAN_POINT ( 'NONE',  ( 86.77499999726882152, 140.1801316387863778, 4.815267126137185549 ) ) ;
#30814 = CARTESIAN_POINT ( 'NONE',  ( 1.156317065392248100, -3.373851915354654896, -0.02993401039715992348 ) ) ;
#30815 = CARTESIAN_POINT ( 'NONE',  ( 38.52499999726881441, 140.1801316387863778, 4.815267126137185549 ) ) ;
#30816 = CARTESIAN_POINT ( 'NONE',  ( -3.662846001190052991, 218.4274158808045740, 34.10113791807857098 ) ) ;
#30817 = DIRECTION ( 'NONE',  ( 1.000000000000000000, 0.000000000000000000, 0.000000000000000000 ) ) ;
#30818 = CARTESIAN_POINT ( 'NONE',  ( -3.044812012440131443, 216.5253028482142952, 85.10113791807857808 ) ) ;
#30819 = CARTESIAN_POINT ( 'NONE',  ( 3.044812012440130555, 197.4746971517856764, 47.60113791807857098 ) ) ;
#30820 = DIRECTION ( 'NONE',  ( 0.000000000000000000, 0.000000000000000000, -1.000000000000000000 ) ) ;
#30821 = CARTESIAN_POINT ( 'NONE',  ( 3.662846001189864698, 218.4274158808046593, 12.39886208192143613 ) ) ;
#30822 = CARTESIAN_POINT ( 'NONE',  ( -0.05014649552828402690, 217.5146222423826714, 30.24886208192143755 ) ) ;
#30823 = CARTESIAN_POINT ( 'NONE',  ( 71.69999999453763451, 142.6655632788954620, -8.961492836873480528 ) ) ;
#30824 = EDGE_LOOP ( 'NONE', ( #12844, #5097, #7376 ) ) ;
#30825 = CARTESIAN_POINT ( 'NONE',  ( -0.05014649552807705357, 194.3824533091408000, 59.75113791807856245 ) ) ;
#30826 = CARTESIAN_POINT ( 'NONE',  ( -4.903702542908602524, 213.8346818373418898, 81.95113791807858661 ) ) ;
#30827 = EDGE_CURVE ( 'NONE', #20612, #20656, #24278, .T. ) ;
#30828 = CARTESIAN_POINT ( 'NONE',  ( -9.984503880673420539, 203.7031108863293980, 41.34886208192143897 ) ) ;
#30829 = EDGE_CURVE ( 'NONE', #11134, #15698, #27812, .T. ) ;
#30830 = AXIS2_PLACEMENT_3D ( 'NONE', #28317, #26097, #4637 ) ;
#30831 = PLANE ( 'NONE',  #27569 ) ;
#30832 = ORIENTED_EDGE ( 'NONE', *, *, #7885, .T. ) ;
#30833 = CARTESIAN_POINT ( 'NONE',  ( 12.00000000000000711, 207.0476921513415220, 45.99886208192143755 ) ) ;
#30834 = ORIENTED_EDGE ( 'NONE', *, *, #1654, .F. ) ;
#30835 = PRODUCT_RELATED_PRODUCT_CATEGORY ( 'part', '', ( #16751 ) ) ;
#30836 = EDGE_LOOP ( 'NONE', ( #31126, #21446 ) ) ;
#30837 = ADVANCED_FACE ( 'NONE', ( #22545 ), #24766, .T. ) ;
#30838 = CIRCLE ( 'NONE', #20498, 112.0000000000000711 ) ;
#30839 = DIRECTION ( 'NONE',  ( -1.000000000000000000, -0.000000000000000000, -0.000000000000000000 ) ) ;
#30840 = CARTESIAN_POINT ( 'NONE',  ( 56.28867513459483263, 139.2280666364260071, -4.041636747397287284E-15 ) ) ;
#30841 = EDGE_LOOP ( 'NONE', ( #23161, #9878, #29403, #998 ) ) ;
#30842 = CARTESIAN_POINT ( 'NONE',  ( 6.444103211791042618, 202.2591342207267644, 35.30113791807856671 ) ) ;
#30843 = EDGE_CURVE ( 'NONE', #13603, #6436, #6706, .T. ) ;
#30844 = CARTESIAN_POINT ( 'NONE',  ( 4.000000000000000000, 3.500000000000000000, 0.000000000000000000 ) ) ;
#30845 = CARTESIAN_POINT ( 'NONE',  ( 6.139770520408223575, 215.5359834540460611, 15.54886208192143293 ) ) ;
#30846 = CARTESIAN_POINT ( 'NONE',  ( 54.67499999726881299, 141.7447067706911810, 9.630534252274376428 ) ) ;
#30847 = EDGE_LOOP ( 'NONE', ( #14225, #24909, #31543, #14215 ) ) ;
#30848 = CARTESIAN_POINT ( 'NONE',  ( 6.500168698208129925, 211.6636982574063381, 58.70113791807857240 ) ) ;
#30849 = CARTESIAN_POINT ( 'NONE',  ( 68.28867513459482552, 139.2280666364260071, -4.041636747397287284E-15 ) ) ;
#30850 = DIRECTION ( 'NONE',  ( -0.5000000000000008882, -0.8660254037844382635, 0.000000000000000000 ) ) ;
#30851 = CARTESIAN_POINT ( 'NONE',  ( 6.220909254589681581, 198.5229672870052582, 100.4488620819214475 ) ) ;
#30852 = CARTESIAN_POINT ( 'NONE',  ( 66.37499999726881583, 155.0000000000000000, 15.58253174999999402 ) ) ;
#30853 = CARTESIAN_POINT ( 'NONE',  ( -6.220909254589537696, 198.5229672870051161, 39.05113791807856671 ) ) ;
#30854 = DIRECTION ( 'NONE',  ( 1.000000000000000000, 0.000000000000000000, 0.000000000000000000 ) ) ;
#30855 = CARTESIAN_POINT ( 'NONE',  ( -6.220909254589537696, 198.5229672870051161, 30.05113791807856671 ) ) ;
#30856 = DIRECTION ( 'NONE',  ( 0.000000000000000000, 0.000000000000000000, -1.000000000000000000 ) ) ;
#30857 = AXIS2_PLACEMENT_3D ( 'NONE', #22986, #2209, #22822 ) ;
#30858 = SHAPE_DEFINITION_REPRESENTATION ( #19481, #18505 ) ;
#30859 = VECTOR ( 'NONE', #7072, 1000.000000000000000 ) ;
#30860 = CARTESIAN_POINT ( 'NONE',  ( 86.99999999999998579, 170.2462022514548323, -7.872454543227099337E-15 ) ) ;
#30861 = CARTESIAN_POINT ( 'NONE',  ( 0.000000000000000000, 0.000000000000000000, -25.03750572909317285 ) ) ;
#30862 = CARTESIAN_POINT ( 'NONE',  ( 32.50000000000000000, 155.0000000000000000, -15.00000000000002487 ) ) ;
#30863 = CARTESIAN_POINT ( 'NONE',  ( -7.456977232089304408, 196.8216656703010301, 3.051137918078566269 ) ) ;
#30864 = CARTESIAN_POINT ( 'NONE',  ( 47.98867513459481415, 146.1832212156128890, 12.13525491562421976 ) ) ;
#30865 = CARTESIAN_POINT ( 'NONE',  ( 50.47499999726880304, 149.9369285172503510, 15.58253174999999580 ) ) ;
#30866 = CARTESIAN_POINT ( 'NONE',  ( 8.118202686958039038, 212.8392687619912635, 46.70113791807857240 ) ) ;
#30867 = B_SPLINE_CURVE_WITH_KNOTS ( 'NONE', 3,
 ( #5514, #29191, #2471, #13516, #81, #23246 ),
 .UNSPECIFIED., .F., .F.,
 ( 4, 2, 4 ),
 ( 0.002044882221487520201, 0.003063384235218495882, 0.004081886248949471996 ),
 .UNSPECIFIED. ) ;
#30868 = CIRCLE ( 'NONE', #3628, 70.00000000000000000 ) ;
#30869 = CARTESIAN_POINT ( 'NONE',  ( 88.12499999726880162, 155.0000000000000000, 15.58253174999999402 ) ) ;
#30870 = CARTESIAN_POINT ( 'NONE',  ( 77.81132485994280046, 159.8737954434936057, -15.00000000000002665 ) ) ;
#30871 = CARTESIAN_POINT ( 'NONE',  ( 8.000000000000000000, 7.960204194457795477E-16, -6.500000000000000000 ) ) ;
#30872 = CARTESIAN_POINT ( 'NONE',  ( 53.19999999453762740, 146.4771138417591203, 11.73074641843673227 ) ) ;
#30873 = ORIENTED_EDGE ( 'NONE', *, *, #16655, .F. ) ;
#30874 = CARTESIAN_POINT ( 'NONE',  ( -0.05014649552807705357, 194.3824533091408000, 29.75113791807856956 ) ) ;
#30875 = CARTESIAN_POINT ( 'NONE',  ( 7.342598717236928252, 0.000000000000000000, 0.000000000000000000 ) ) ;
#30876 = CARTESIAN_POINT ( 'NONE',  ( 0.05014649552828275708, 196.4853777576173002, 13.74886208192143400 ) ) ;
#30877 = CARTESIAN_POINT ( 'NONE',  ( 72.99495483890930814, 155.0000000000000000, 15.50000000000000355 ) ) ;
#30878 = EDGE_LOOP ( 'NONE', ( #32665, #24621, #7242, #9120 ) ) ;
#30879 = CARTESIAN_POINT ( 'NONE',  ( 3.044812012440130555, 197.4746971517856764, 11.60113791807856742 ) ) ;
#30880 = CARTESIAN_POINT ( 'NONE',  ( 6.139770520408368348, 198.4640165459539674, 74.45113791807857240 ) ) ;
#30881 = VECTOR ( 'NONE', #22661, 1000.000000000000000 ) ;
#30882 = VERTEX_POINT ( 'NONE', #14868 ) ;
#30883 = CARTESIAN_POINT ( 'NONE',  ( 2.426778023690075337, 214.6231898156240447, 33.39886208192144323 ) ) ;
#30884 = STYLED_ITEM ( 'NONE', ( #658 ), #789 ) ;
#30885 = CARTESIAN_POINT ( 'NONE',  ( -2.466666666666999408, 3.653529617456472921E-16, 3.099999999999998757 ) ) ;
#30886 = ORIENTED_EDGE ( 'NONE', *, *, #14363, .F. ) ;
#30887 = CARTESIAN_POINT ( 'NONE',  ( 7.984503880673485376, 204.3529502787953902, 8.151137918078566358 ) ) ;
#30888 = CARTESIAN_POINT ( 'NONE',  ( -3.662846001189865142, 195.5725841191952838, 85.89886208192143613 ) ) ;
#30889 = CARTESIAN_POINT ( 'NONE',  ( 37.97499999726881015, 169.8198683612136222, 4.815267126137181997 ) ) ;
#30891 = ORIENTED_EDGE ( 'NONE', *, *, #32268, .T. ) ;
#30890 = VECTOR ( 'NONE', #1427, 1000.000000000000000 ) ;
#30892 = CARTESIAN_POINT ( 'NONE',  ( 41.92499999726881299, 164.1591823560292198, 12.60653300113718167 ) ) ;
#30893 = CARTESIAN_POINT ( 'NONE',  ( 120.8017490774095251, 3.226370279868335800, 35.00001199999999102 ) ) ;
#30894 = CARTESIAN_POINT ( 'NONE',  ( 6.139770520408368348, 198.4640165459539674, 5.451137918078567068 ) ) ;
#30895 = CARTESIAN_POINT ( 'NONE',  ( -9.984503880673420539, 203.7031108863293980, 74.34886208192143897 ) ) ;
#30896 = CARTESIAN_POINT ( 'NONE',  ( 47.67499999726880588, 168.2552932293087906, -9.630534252274385310 ) ) ;
#30897 = CARTESIAN_POINT ( 'NONE',  ( -67.50001199999998391, 153.8873526018535927, 17.00000000000001066 ) ) ;
#30898 = CARTESIAN_POINT ( 'NONE',  ( -8.062137200540920645, 212.9164362838581894, 9.801137918078566713 ) ) ;
#30899 = CARTESIAN_POINT ( 'NONE',  ( -67.50000000000000000, 155.0000000000000000, -37.00000000000000000 ) ) ;
#30900 = CARTESIAN_POINT ( 'NONE',  ( 68.79999999999999716, 167.3344367211045096, -8.961492836873482304 ) ) ;
#30901 = CARTESIAN_POINT ( 'NONE',  ( 10.01549611932653860, 210.2015048109876716, 94.85113791807857808 ) ) ;
#30902 = DIRECTION ( 'NONE',  ( -1.000000000000000000, -1.776356839400250465E-15, 0.000000000000000000 ) ) ;
#30903 = CARTESIAN_POINT ( 'NONE',  ( -6.139770520408369237, 215.5359834540460042, 75.95113791807857240 ) ) ;
#30904 = AXIS2_PLACEMENT_3D ( 'NONE', #27226, #7123, #27554 ) ;
#30905 = CARTESIAN_POINT ( 'NONE',  ( 3.500000000000004441, 1.362959798491822250, -0.1397344949837900085 ) ) ;
#30906 = CARTESIAN_POINT ( 'NONE',  ( 33.77499999726880731, 169.8198683612136222, -4.815267126137197984 ) ) ;
#30907 = CARTESIAN_POINT ( 'NONE',  ( -3.662846001189865142, 195.5725841191952838, 88.89886208192143613 ) ) ;
#30908 = AXIS2_PLACEMENT_3D ( 'NONE', #3085, #32197, #24370 ) ;
#30909 = CARTESIAN_POINT ( 'NONE',  ( 73.32499999726880446, 164.1591823560292198, -12.60653300113719766 ) ) ;
#30910 = ORIENTED_EDGE ( 'NONE', *, *, #14399, .T. ) ;
#30911 = CARTESIAN_POINT ( 'NONE',  ( -60.98379214578430663, 194.9989775857802385, -0.3278793750673599239 ) ) ;
#30912 = CARTESIAN_POINT ( 'NONE',  ( 37.19999999453762740, 146.4771138417591203, 11.73074641843673227 ) ) ;
#30913 = CARTESIAN_POINT ( 'NONE',  ( 11.98450388067348271, 203.0532714938637753, 95.15113791807856103 ) ) ;
#30914 =( BOUNDED_CURVE ( )  B_SPLINE_CURVE ( 2, ( #4682, #1959, #2300, #9971, #2137, #27680, #15068, #12522, #33304, #12685, #18432 ),
 .UNSPECIFIED., .F., .F. ) 
 B_SPLINE_CURVE_WITH_KNOTS ( ( 3, 2, 2, 2, 2, 3 ),
 ( 0.6428571428571427937, 0.6464285714285713524, 0.6499999999999999112, 0.6535714285714285809, 0.6571428571428571397, 0.6607142857142856984 ),
 .UNSPECIFIED. ) 
 CURVE ( )  GEOMETRIC_REPRESENTATION_ITEM ( )  RATIONAL_B_SPLINE_CURVE ( ( 1.000000000000001554, 0.9510565162951518658, 1.000000000000000000, 0.9510565162951534202, 1.000000000000000000, 0.9510565162951534202, 1.000000000000000000, 0.9510565162951534202, 1.000000000000000000, 0.9510565162951534202, 1.000000000000000000 ) ) 
 REPRESENTATION_ITEM ( '' )  );
#30915 = CARTESIAN_POINT ( 'NONE',  ( 4.200000000000001954, 0.000000000000000000, 2.000000000000000888 ) ) ;
#30916 = AXIS2_PLACEMENT_3D ( 'NONE', #29169, #6507, #16378 ) ;
#30917 = EDGE_LOOP ( 'NONE', ( #6685, #33088, #9525, #18122 ) ) ;
#30918 = CARTESIAN_POINT ( 'NONE',  ( 10.00000000000000711, 207.0476921513415220, 87.99886208192144466 ) ) ;
#30919 = CARTESIAN_POINT ( 'NONE',  ( 3.662846001189864698, 218.4274158808046593, 27.39886208192143613 ) ) ;
#30920 = DIRECTION ( 'NONE',  ( -1.000000000000000000, -0.000000000000000000, -0.000000000000000000 ) ) ;
#30921 = CARTESIAN_POINT ( 'NONE',  ( -3.044812012440131443, 216.5253028482142952, 40.10113791807857098 ) ) ;
#30922 = VERTEX_POINT ( 'NONE', #30384 ) ;
#30923 = CARTESIAN_POINT ( 'NONE',  ( -6.220909254589682469, 215.4770327129946850, 101.9488620819214333 ) ) ;
#30924 = CARTESIAN_POINT ( 'NONE',  ( 92.60208470531341618, 155.0000000000000000, -32.00000000000001421 ) ) ;
#30925 = EDGE_LOOP ( 'NONE', ( #18263, #5307, #1963, #28778 ) ) ;
#30926 = CARTESIAN_POINT ( 'NONE',  ( 8.000000000000008882, 207.0476921513415220, 78.99886208192144466 ) ) ;
#30927 = CONICAL_SURFACE ( 'NONE', #14024, 6.500000000000000888, 0.8987552595851582282 ) ;
#30928 = VERTEX_POINT ( 'NONE', #7045 ) ;
#30929 = ADVANCED_FACE ( 'NONE', ( #9425 ), #19819, .F. ) ;
#30930 = AXIS2_PLACEMENT_3D ( 'NONE', #23459, #7633, #33133 ) ;
#30931 = DIRECTION ( 'NONE',  ( -1.000000000000000000, 0.000000000000000000, 0.000000000000000000 ) ) ;
#30932 = ORIENTED_EDGE ( 'NONE', *, *, #23699, .F. ) ;
#30933 = DIRECTION ( 'NONE',  ( 1.000000000000000000, 0.000000000000000000, 0.000000000000000000 ) ) ;
#30934 = CARTESIAN_POINT ( 'NONE',  ( -0.05014649552807731031, 198.5883022060938572, 56.75113791807857666 ) ) ;
#30935 = CARTESIAN_POINT ( 'NONE',  ( 82.02499999726879309, 160.0630714827496206, 15.58253174999999402 ) ) ;
#30936 = FACE_OUTER_BOUND ( 'NONE', #30147, .T. ) ;
#30937 = CARTESIAN_POINT ( 'NONE',  ( -7.984503880673488041, 209.6470497212046098, 84.65113791807856103 ) ) ;
#30938 = CARTESIAN_POINT ( 'NONE',  ( 2.459698528280935825, -7.240146430416073642, -0.09933465333851955459 ) ) ;
#30939 = AXIS2_PLACEMENT_3D ( 'NONE', #15973, #31644, #11196 ) ;
#30940 = CARTESIAN_POINT ( 'NONE',  ( 45.80000000000000426, 142.6655632788954620, 8.961492836873471646 ) ) ;
#30941 = CARTESIAN_POINT ( 'NONE',  ( 2.517493886309087436, 199.4062855549015865, 64.59886208192142476 ) ) ;
#30942 = CARTESIAN_POINT ( 'NONE',  ( -9.984503880673475606, 210.2968891136704315, 3.651137918078565470 ) ) ;
#30943 = CARTESIAN_POINT ( 'NONE',  ( -6.250000000000000888, 5.051814855409225480, -7.198902722707429369 ) ) ;
#30944 = DIRECTION ( 'NONE',  ( 0.000000000000000000, 0.000000000000000000, 1.000000000000000000 ) ) ;
#30945 = CARTESIAN_POINT ( 'NONE',  ( 59.12499999726881583, 155.0000000000000000, -15.58253175000000823 ) ) ;
#30946 = CARTESIAN_POINT ( 'NONE',  ( 72.77499999726882152, 140.1801316387863778, 4.815267126137185549 ) ) ;
#30947 = CARTESIAN_POINT ( 'NONE',  ( -12.00000000000000711, 207.0476921513413515, 66.50113791807856956 ) ) ;
#30948 = ADVANCED_FACE ( 'NONE', ( #1930 ), #10167, .F. ) ;
#30949 = FACE_BOUND ( 'NONE', #12429, .T. ) ;
#30950 = VECTOR ( 'NONE', #24472, 1000.000000000000000 ) ;
#30951 = PRODUCT_DEFINITION_SHAPE ( 'NONE', 'NONE',  #33690 ) ;
#30952 = CARTESIAN_POINT ( 'NONE',  ( -12.00000000000000711, 207.0476921513413515, 12.50113791807856600 ) ) ;
#30953 = CARTESIAN_POINT ( 'NONE',  ( 10.01549611932653860, 210.2015048109876716, 88.85113791807857808 ) ) ;
#30954 = CONICAL_SURFACE ( 'NONE', #20614, 32.00000000000002842, 0.1047197551196784177 ) ;
#30955 = AXIS2_PLACEMENT_3D ( 'NONE', #15078, #25474, #28205 ) ;
#30956 = CARTESIAN_POINT ( 'NONE',  ( 7.456977232089471386, 196.8216656703012006, 55.44886208192143329 ) ) ;
#30957 = CARTESIAN_POINT ( 'NONE',  ( -6.139770520408224463, 198.4640165459539105, 56.04886208192142760 ) ) ;
#30958 = CARTESIAN_POINT ( 'NONE',  ( -54.50000000000002132, 0.000000000000000000, 270.4495957273638282 ) ) ;
#30959 = CARTESIAN_POINT ( 'NONE',  ( 7.456977232089302632, 217.1783343296989131, 94.55113791807855250 ) ) ;
#30960 = CARTESIAN_POINT ( 'NONE',  ( 34.68867513459483831, 150.1262045565065364, -15.00000000000012434 ) ) ;
#30961 = CARTESIAN_POINT ( 'NONE',  ( 8.062137200540920645, 201.0835637161417822, -0.6988620819214342861 ) ) ;
#30962 = CARTESIAN_POINT ( 'NONE',  ( 6.139770520408223575, 215.5359834540460611, 69.54886208192142760 ) ) ;
#30963 = AXIS2_PLACEMENT_3D ( 'NONE', #26326, #16263, #5866 ) ;
#30964 = ORIENTED_EDGE ( 'NONE', *, *, #14300, .T. ) ;
#30965 = CARTESIAN_POINT ( 'NONE',  ( -9.736236675708031640, 214.0148392665760753, 77.79886208192142760 ) ) ;
#30966 = CARTESIAN_POINT ( 'NONE',  ( 0.05014649552810505201, 217.5146222423826714, 88.25113791807858377 ) ) ;
#30967 = ORIENTED_EDGE ( 'NONE', *, *, #24920, .T. ) ;
#30968 = CARTESIAN_POINT ( 'NONE',  ( 77.37499999726881583, 155.0000000000000000, -15.58253175000000823 ) ) ;
#30969 = CARTESIAN_POINT ( 'NONE',  ( -0.05014649552828365914, 215.4116977939061144, 54.24886208192144466 ) ) ;
#30970 = ORIENTED_EDGE ( 'NONE', *, *, #9401, .T. ) ;
#30971 = EDGE_CURVE ( 'NONE', #6381, #3669, #7594, .T. ) ;
#30972 = CARTESIAN_POINT ( 'NONE',  ( 73.82499999726880446, 168.2552932293087906, 9.630534252274372875 ) ) ;
#30973 = FACE_OUTER_BOUND ( 'NONE', #13155, .T. ) ;
#30974 = DIRECTION ( 'NONE',  ( 1.000000000000000000, 0.000000000000000000, 0.000000000000000000 ) ) ;
#30975 = AXIS2_PLACEMENT_3D ( 'NONE', #13870, #3150, #24436 ) ;
#30976 = CARTESIAN_POINT ( 'NONE',  ( 62.52499999726882152, 140.1801316387863778, 4.815267126137185549 ) ) ;
#30977 = CYLINDRICAL_SURFACE ( 'NONE', #2600, 13.00000000000001776 ) ;
#30978 = CARTESIAN_POINT ( 'NONE',  ( 9.984503880673420539, 210.2968891136705167, 51.84886208192143897 ) ) ;
#30979 = VERTEX_POINT ( 'NONE', #23393 ) ;
#30980 = CARTESIAN_POINT ( 'NONE',  ( 115.4999999999999858, 129.0854607986834139, -100.8678580070901063 ) ) ;
#30981 = EDGE_CURVE ( 'NONE', #28157, #12982, #12999, .T. ) ;
#30982 = CIRCLE ( 'NONE', #13546, 7.500000000000001776 ) ;
#30983 = FACE_OUTER_BOUND ( 'NONE', #19306, .T. ) ;
#30984 = CARTESIAN_POINT ( 'NONE',  ( 92.60208470531341618, 155.0000000000000000, -31.00000000000000000 ) ) ;
#30985 = CARTESIAN_POINT ( 'NONE',  ( -4.903702542908436435, 200.1653181626580249, 32.04886208192144181 ) ) ;
#30986 = CARTESIAN_POINT ( 'NONE',  ( -8.062137200540920645, 212.9164362838581894, 66.80113791807858092 ) ) ;
#30987 = CARTESIAN_POINT ( 'NONE',  ( 62.78867513459482552, 155.0000000000000000, -15.00000000000002487 ) ) ;
#30988 = CARTESIAN_POINT ( 'NONE',  ( 8.118202686958039038, 212.8392687619912635, 58.70113791807857240 ) ) ;
#30989 = CARTESIAN_POINT ( 'NONE',  ( 6.139770520408368348, 198.4640165459539674, 29.45113791807856529 ) ) ;
#30990 = CARTESIAN_POINT ( 'NONE',  ( -6.444103211791042618, 211.7408657792732356, 15.80113791807856849 ) ) ;
#30991 = DIRECTION ( 'NONE',  ( 0.000000000000000000, -0.7071067811865411334, 0.7071067811865540120 ) ) ;
#30992 = CARTESIAN_POINT ( 'NONE',  ( 115.4999999999999858, 255.8678580070898363, -25.91453920131763056 ) ) ;
#30993 = CARTESIAN_POINT ( 'NONE',  ( 39.12499999726880873, 155.0000000000000000, -15.58253175000000823 ) ) ;
#30994 = CARTESIAN_POINT ( 'NONE',  ( 0.05014649552807549926, 219.6175466908591716, 34.25113791807857666 ) ) ;
#30995 = LINE ( 'NONE', #10209, #12442 ) ;
#30996 = EDGE_CURVE ( 'NONE', #18396, #30404, #25504, .T. ) ;
#30997 = CARTESIAN_POINT ( 'NONE',  ( 8.118202686958039038, 212.8392687619912635, 82.70113791807857240 ) ) ;
#30998 = CARTESIAN_POINT ( 'NONE',  ( -6.220909254589537696, 198.5229672870051445, 57.05113791807857382 ) ) ;
#30999 = CARTESIAN_POINT ( 'NONE',  ( 32.50000000000000000, 155.0000000000000000, -15.00000000000002487 ) ) ;
#31000 = CARTESIAN_POINT ( 'NONE',  ( -3.753561863808878130, 218.3979405102790281, 24.09886208192143897 ) ) ;
#31001 = CARTESIAN_POINT ( 'NONE',  ( 6.220909254589680693, 198.5229672870052582, 31.44886208192142973 ) ) ;
#31002 = CARTESIAN_POINT ( 'NONE',  ( 70.39999999453763735, 168.7903194862797420, -4.480746418436745593 ) ) ;
#31003 = ORIENTED_EDGE ( 'NONE', *, *, #31847, .F. ) ;
#31004 = CARTESIAN_POINT ( 'NONE',  ( 9.680171189290831535, 199.9079932115568852, 65.30113791807858092 ) ) ;
#31005 = VECTOR ( 'NONE', #1723, 1000.000000000000000 ) ;
#31006 = CARTESIAN_POINT ( 'NONE',  ( 8.000000000000008882, 206.9523078486586485, 80.00113791807856956 ) ) ;
#31007 = EDGE_CURVE ( 'NONE', #27265, #7110, #33003, .T. ) ;
#31008 = CARTESIAN_POINT ( 'NONE',  ( 8.118202686958138514, 201.1607312380088501, 43.29886208192143471 ) ) ;
#31009 = DIRECTION ( 'NONE',  ( 0.000000000000000000, 0.000000000000000000, -1.000000000000000000 ) ) ;
#31010 = ORIENTED_EDGE ( 'NONE', *, *, #27884, .T. ) ;
#31011 = CARTESIAN_POINT ( 'NONE',  ( -12.01549611932659722, 210.8513442034533227, 53.64886208192142902 ) ) ;
#31012 = VERTEX_POINT ( 'NONE', #12826 ) ;
#31013 = ORIENTED_EDGE ( 'NONE', *, *, #29333, .T. ) ;
#31014 = DIRECTION ( 'NONE',  ( 0.000000000000000000, 0.000000000000000000, -1.000000000000000000 ) ) ;
#31015 = CARTESIAN_POINT ( 'NONE',  ( -119.7500000000000000, 0.000000000000000000, -35.00000000000000000 ) ) ;
#31016 = ORIENTED_EDGE ( 'NONE', *, *, #17916, .F. ) ;
#31017 = CARTESIAN_POINT ( 'NONE',  ( -8.015496119326531499, 204.4483345814780364, 42.35113791807857098 ) ) ;
#31018 = CARTESIAN_POINT ( 'NONE',  ( -8.118202686958138514, 212.8392687619910930, 26.79886208192143826 ) ) ;
#31019 = CARTESIAN_POINT ( 'NONE',  ( 61.67499999726881299, 168.2552932293087906, -9.630534252274387086 ) ) ;
#31020 = ORIENTED_EDGE ( 'NONE', *, *, #15948, .T. ) ;
#31021 = DIRECTION ( 'NONE',  ( -1.000000000000000000, 0.000000000000000000, 0.000000000000000000 ) ) ;
#31022 = FILL_AREA_STYLE_COLOUR ( '', #22505 ) ;
#31023 = DIRECTION ( 'NONE',  ( 1.000000000000000000, 0.000000000000000000, 0.000000000000000000 ) ) ;
#31024 = CARTESIAN_POINT ( 'NONE',  ( -8.000000000000008882, 206.9523078486584780, 2.498862081921435330 ) ) ;
#31025 = CARTESIAN_POINT ( 'NONE',  ( -0.05014649552810635652, 196.4853777576173002, 44.75113791807858377 ) ) ;
#31026 = CARTESIAN_POINT ( 'NONE',  ( 79.50000000000000000, 155.0000000000000000, -6.938893903907228378E-15 ) ) ;
#31027 = EDGE_CURVE ( 'NONE', #25327, #14208, #31338, .T. ) ;
#31028 = CARTESIAN_POINT ( 'NONE',  ( -8.118202686958039038, 201.1607312380087080, 27.20113791807856884 ) ) ;
#31029 = CARTESIAN_POINT ( 'NONE',  ( 9.984503880673420539, 210.2968891136705736, 102.8488620819214390 ) ) ;
#31030 = CARTESIAN_POINT ( 'NONE',  ( -8.000000000000008882, 206.9523078486584780, 83.49886208192144466 ) ) ;
#31031 = CARTESIAN_POINT ( 'NONE',  ( 34.72499999726881015, 140.1801316387863778, -4.815267126137194431 ) ) ;
#31032 = CARTESIAN_POINT ( 'NONE',  ( -2.352990130084580066E-16, 8.660254037844390851, -7.422398894150034288 ) ) ;
#31033 = DIRECTION ( 'NONE',  ( 1.000000000000000000, 0.000000000000000000, 0.000000000000000000 ) ) ;
#31034 = CARTESIAN_POINT ( 'NONE',  ( 0.05014649552807549926, 219.6175466908591716, 10.25113791807856600 ) ) ;
#31035 = CARTESIAN_POINT ( 'NONE',  ( 53.67499999726879878, 168.2552932293087906, -9.630534252274385310 ) ) ;
#31036 = EDGE_CURVE ( 'NONE', #5762, #13676, #25938, .T. ) ;
#31037 = CARTESIAN_POINT ( 'NONE',  ( -6.139770520408369237, 215.5359834540460042, 60.95113791807857950 ) ) ;
#31038 = CARTESIAN_POINT ( 'NONE',  ( 34.78867513459482552, 155.0000000000000000, -15.00000000000002487 ) ) ;
#31039 = CARTESIAN_POINT ( 'NONE',  ( 78.51132485994280330, 163.8167787843871110, 12.13525491562421621 ) ) ;
#31040 = DIRECTION ( 'NONE',  ( 1.000000000000000000, 0.000000000000000000, 0.000000000000000000 ) ) ;
#31041 = CARTESIAN_POINT ( 'NONE',  ( 56.49999999453761745, 170.2462022514548323, -7.872454543227099337E-15 ) ) ;
#31042 = ORIENTED_EDGE ( 'NONE', *, *, #6007, .T. ) ;
#31043 = CARTESIAN_POINT ( 'NONE',  ( 3.662846001190051659, 195.5725841191953691, 38.60113791807855677 ) ) ;
#31044 = EDGE_CURVE ( 'NONE', #25169, #5147, #24837, .T. ) ;
#31045 = CARTESIAN_POINT ( 'NONE',  ( 4.000000000000000000, 3.518949890710768802, -4.770489558936219510E-15 ) ) ;
#31046 = CARTESIAN_POINT ( 'NONE',  ( -9.984503880673420539, 203.7031108863293980, 11.34886208192143187 ) ) ;
#31047 = CARTESIAN_POINT ( 'NONE',  ( 60.71132485994280614, 155.0000000000000000, 15.00000000000001243 ) ) ;
#31048 = EDGE_LOOP ( 'NONE', ( #3249, #26535, #11461, #11348 ) ) ;
#31049 = CARTESIAN_POINT ( 'NONE',  ( 10.00000000000000711, 206.9523078486586201, 8.001137918078566003 ) ) ;
#31050 = CARTESIAN_POINT ( 'NONE',  ( 8.118202686958039038, 212.8392687619912635, 67.70113791807858661 ) ) ;
#31051 = EDGE_LOOP ( 'NONE', ( #11246, #8697, #21347, #15411 ) ) ;
#31052 = CARTESIAN_POINT ( 'NONE',  ( 2.426778023690075337, 214.6231898156240447, 30.39886208192143613 ) ) ;
#31053 = DIRECTION ( 'NONE',  ( -1.000000000000000000, 0.000000000000000000, 0.000000000000000000 ) ) ;
#31054 = CARTESIAN_POINT ( 'NONE',  ( 77.87499999726883004, 171.3844434931184253, -7.942151717890134290E-15 ) ) ;
#31055 = VERTEX_POINT ( 'NONE', #20324 ) ;
#31056 = CARTESIAN_POINT ( 'NONE',  ( -2.426778023690262742, 214.6231898156240163, 10.10113791807856742 ) ) ;
#31057 = CARTESIAN_POINT ( 'NONE',  ( 7.375838497908012492, 217.2372850707501186, 99.54886208192144181 ) ) ;
#31058 = CARTESIAN_POINT ( 'NONE',  ( 38.27499999726881441, 160.0630714827496206, 15.58253174999999224 ) ) ;
#31059 = VERTEX_POINT ( 'NONE', #15039 ) ;
#31060 = CARTESIAN_POINT ( 'NONE',  ( 49.22499999726881725, 160.0630714827496206, -15.58253175000000823 ) ) ;
#31061 = DIRECTION ( 'NONE',  ( -1.000000000000000000, -0.000000000000000000, -0.000000000000000000 ) ) ;
#31062 = CARTESIAN_POINT ( 'NONE',  ( -9.984503880673473830, 210.2968891136704315, 6.651137918078564581 ) ) ;
#31063 = AXIS2_PLACEMENT_3D ( 'NONE', #26718, #19057, #833 ) ;
#31064 = CARTESIAN_POINT ( 'NONE',  ( 10.00000000000000711, 207.0476921513415220, 75.99886208192144466 ) ) ;
#31065 = CARTESIAN_POINT ( 'NONE',  ( 45.87499999726880162, 171.3844434931184253, -7.942151717890132712E-15 ) ) ;
#31066 = CARTESIAN_POINT ( 'NONE',  ( -67.50001199999999812, 141.4831703651136081, -10.36982646209944470 ) ) ;
#31067 = CARTESIAN_POINT ( 'NONE',  ( -0.05014649552810635652, 196.4853777576173002, 14.75113791807856245 ) ) ;
#31068 = CARTESIAN_POINT ( 'NONE',  ( -65.25000000000000000, -6.704941225331758039E-15, 35.00000000000000000 ) ) ;
#31069 = EDGE_CURVE ( 'NONE', #17976, #7786, #1087, .T. ) ;
#31070 = CARTESIAN_POINT ( 'NONE',  ( 65.99999999999998579, 139.7537977485451393, -4.138211985947621020E-15 ) ) ;
#31071 = CARTESIAN_POINT ( 'NONE',  ( -8.062137200540920645, 212.9164362838581894, 99.80113791807858092 ) ) ;
#31072 = CARTESIAN_POINT ( 'NONE',  ( -27.50000000000000000, -9.324699302609168683, -0.8718021930569370692 ) ) ;
#31073 = CARTESIAN_POINT ( 'NONE',  ( -3.135527875058821579, 197.5041725223112223, 86.90113791807857524 ) ) ;
#31074 = CARTESIAN_POINT ( 'NONE',  ( -65.20000000000000284, -7.347880794884118356E-15, -19.30000000000003979 ) ) ;
#31075 = CYLINDRICAL_SURFACE ( 'NONE', #4205, 12.10452846326765020 ) ;
#31076 = EDGE_CURVE ( 'NONE', #21262, #9926, #24330, .T. ) ;
#31077 = CARTESIAN_POINT ( 'NONE',  ( 7.456977232089471386, 196.8216656703012006, 100.4488620819214475 ) ) ;
#31078 = CARTESIAN_POINT ( 'NONE',  ( 68.32499999726881867, 145.8408176439707802, 12.60653300113718345 ) ) ;
#31079 = ORIENTED_EDGE ( 'NONE', *, *, #18559, .T. ) ;
#31080 = CARTESIAN_POINT ( 'NONE',  ( 65.25000000000000000, 7.347880794884118356E-15, 35.00000000000000000 ) ) ;
#31081 = CARTESIAN_POINT ( 'NONE',  ( 37.69999999453763451, 142.6655632788954620, -8.961492836873480528 ) ) ;
#31082 = CARTESIAN_POINT ( 'NONE',  ( 3.753561863808689836, 218.3979405102790565, 100.4011379180785895 ) ) ;
#31083 = LINE ( 'NONE', #23409, #11566 ) ;
#31084 = ORIENTED_EDGE ( 'NONE', *, *, #29071, .T. ) ;
#31085 = CARTESIAN_POINT ( 'NONE',  ( 3.044812012439969795, 216.5253028482143520, 84.39886208192143613 ) ) ;
#31086 = AXIS2_PLACEMENT_3D ( 'NONE', #31478, #6361, #28912 ) ;
#31087 = CARTESIAN_POINT ( 'NONE',  ( -0.05014649552828442242, 219.6175466908591716, 21.24886208192143755 ) ) ;
#31088 = CARTESIAN_POINT ( 'NONE',  ( 85.71132485994282035, 155.0000000000000000, -15.00000000000002487 ) ) ;
#31089 = CARTESIAN_POINT ( 'NONE',  ( 3.135527875058820690, 216.4958274776887492, 40.40113791807857524 ) ) ;
#31090 = ORIENTED_EDGE ( 'NONE', *, *, #13726, .F. ) ;
#31091 = CARTESIAN_POINT ( 'NONE',  ( -4.903702542908436435, 200.1653181626580249, 5.048862081921433820 ) ) ;
#31092 = CARTESIAN_POINT ( 'NONE',  ( 127.5000000000000000, 231.4735983853249763, -73.43303922622311575 ) ) ;
#31093 = ORIENTED_EDGE ( 'NONE', *, *, #29387, .F. ) ;
#31094 = CARTESIAN_POINT ( 'NONE',  ( 4.984841277089891776, 200.2242689037093726, 85.44886208192144750 ) ) ;
#31095 = ORIENTED_EDGE ( 'NONE', *, *, #13935, .F. ) ;
#31096 = CARTESIAN_POINT ( 'NONE',  ( 0.05014649552807626948, 215.4116977939061144, 34.25113791807857666 ) ) ;
#31097 = CARTESIAN_POINT ( 'NONE',  ( 8.331345277524542681, 0.000000000000000000, -8.000000000000000000 ) ) ;
#31098 = ORIENTED_EDGE ( 'NONE', *, *, #15338, .F. ) ;
#31099 = CARTESIAN_POINT ( 'NONE',  ( 80.72499999726881015, 140.1801316387863778, -4.815267126137194431 ) ) ;
#31100 = DIRECTION ( 'NONE',  ( 0.000000000000000000, 0.000000000000000000, 1.000000000000000000 ) ) ;
#31101 = CARTESIAN_POINT ( 'NONE',  ( 8.015496119326531499, 209.5516654185219636, 85.85113791807857808 ) ) ;
#31102 = CYLINDRICAL_SURFACE ( 'NONE', #14073, 31.00000000000000000 ) ;
#31103 = AXIS2_PLACEMENT_3D ( 'NONE', #27487, #17433, #4142 ) ;
#31104 = CARTESIAN_POINT ( 'NONE',  ( 51.10000000000000853, 168.7903194862797420, 4.480746418436729606 ) ) ;
#31105 = CARTESIAN_POINT ( 'NONE',  ( -4.903702542908436435, 200.1653181626580249, 59.04886208192144181 ) ) ;
#31106 = DIRECTION ( 'NONE',  ( -0.1461455375466716444, 0.9854922318508084755, -0.08629335326029916042 ) ) ;
#31107 = EDGE_CURVE ( 'NONE', #28318, #13425, #19564, .T. ) ;
#31108 = CARTESIAN_POINT ( 'NONE',  ( 54.22499999726881015, 149.9369285172503510, 15.58253174999999580 ) ) ;
#31109 = CARTESIAN_POINT ( 'NONE',  ( -6.139770520408368348, 215.5359834540460042, 3.951137918078565736 ) ) ;
#31110 = CARTESIAN_POINT ( 'NONE',  ( -65.20000000000000284, 0.9203920079924583497, -19.30000000000004690 ) ) ;
#31111 = CARTESIAN_POINT ( 'NONE',  ( 60.22499999726880304, 149.9369285172503510, 15.58253174999999580 ) ) ;
#31112 = CARTESIAN_POINT ( 'NONE',  ( 68.77499999726880731, 140.1801316387863778, 4.815267126137185549 ) ) ;
#31113 = CARTESIAN_POINT ( 'NONE',  ( 11.98450388067348271, 203.0532714938637753, 68.15113791807856103 ) ) ;
#31114 = CARTESIAN_POINT ( 'NONE',  ( 46.61132485994281893, 159.8737954434935489, 15.00000000000006040 ) ) ;
#31115 = CARTESIAN_POINT ( 'NONE',  ( 11.98450388067348271, 203.0532714938637753, 8.151137918078566358 ) ) ;
#31116 = CARTESIAN_POINT ( 'NONE',  ( -9.984503880673475606, 210.2968891136704315, 87.65113791807856103 ) ) ;
#31117 = CARTESIAN_POINT ( 'NONE',  ( 3.753561863808876797, 195.6020594897209719, 49.59886208192143897 ) ) ;
#31118 = CARTESIAN_POINT ( 'NONE',  ( -10.01549611932659545, 210.2015048109875011, 53.64886208192142902 ) ) ;
#31119 = CARTESIAN_POINT ( 'NONE',  ( -3.662846001190052991, 218.4274158808045740, 100.1011379180785781 ) ) ;
#31120 = PLANE ( 'NONE',  #18100 ) ;
#31121 = CARTESIAN_POINT ( 'NONE',  ( -6.220909254589537696, 198.5229672870051161, 12.05113791807856671 ) ) ;
#31122 = CARTESIAN_POINT ( 'NONE',  ( -8.118202686958138514, 212.8392687619910930, 83.79886208192144181 ) ) ;
#31123 = ORIENTED_EDGE ( 'NONE', *, *, #13543, .F. ) ;
#31124 = CARTESIAN_POINT ( 'NONE',  ( 7.375838497908012492, 217.2372850707501186, 78.54886208192142760 ) ) ;
#31125 = CARTESIAN_POINT ( 'NONE',  ( 9.984503880673470277, 203.7031108863295401, 95.15113791807854682 ) ) ;
#31126 = ORIENTED_EDGE ( 'NONE', *, *, #31198, .T. ) ;
#31127 = CARTESIAN_POINT ( 'NONE',  ( 77.47499999726878173, 160.0630714827496206, -15.58253175000000823 ) ) ;
#31128 = CARTESIAN_POINT ( 'NONE',  ( 2.517493886309087436, 199.4062855549015865, 52.59886208192143897 ) ) ;
#31129 = VERTEX_POINT ( 'NONE', #24505 ) ;
#31130 = CARTESIAN_POINT ( 'NONE',  ( 68.82499999726880446, 141.7447067706911810, -9.630534252274387086 ) ) ;
#31131 = DIRECTION ( 'NONE',  ( 0.000000000000000000, 0.000000000000000000, -1.000000000000000000 ) ) ;
#31132 = CARTESIAN_POINT ( 'NONE',  ( -58.50000000000002132, 194.9217985566782829, 2.500000000000000000 ) ) ;
#31133 = CARTESIAN_POINT ( 'NONE',  ( 61.32499999726881157, 164.1591823560292198, -12.60653300113719766 ) ) ;
#31134 = CARTESIAN_POINT ( 'NONE',  ( -7.500000000000000000, -3.882691789160215290, -7.781695678273567118 ) ) ;
#31135 = CARTESIAN_POINT ( 'NONE',  ( 8.062137200540822946, 212.9164362838583315, 48.69886208192144039 ) ) ;
#31136 = ORIENTED_EDGE ( 'NONE', *, *, #622, .T. ) ;
#31137 = PLANE ( 'NONE',  #19455 ) ;
#31138 = LINE ( 'NONE', #26028, #29196 ) ;
#31139 = CARTESIAN_POINT ( 'NONE',  ( -0.05014649552828365914, 215.4116977939061144, 36.24886208192143755 ) ) ;
#31140 = CARTESIAN_POINT ( 'NONE',  ( -9.984503880673473830, 210.2968891136704315, 72.65113791807857524 ) ) ;
#31141 = CARTESIAN_POINT ( 'NONE',  ( 45.38867513459482694, 169.2658477444273331, 4.635254915624208216 ) ) ;
#31142 = CARTESIAN_POINT ( 'NONE',  ( 3.135527875058820690, 216.4958274776887492, 58.40113791807857524 ) ) ;
#31143 = PRODUCT_DEFINITION_FORMATION_WITH_SPECIFIED_SOURCE ( 'ANY', '', #22483, .NOT_KNOWN. ) ;
#31144 = CARTESIAN_POINT ( 'NONE',  ( -10.01549611932653860, 203.7984951890123284, 24.35113791807855677 ) ) ;
#31145 = CARTESIAN_POINT ( 'NONE',  ( -4.984841277089726574, 200.2242689037092305, 15.05113791807856849 ) ) ;
#31146 = CARTESIAN_POINT ( 'NONE',  ( -105.0000000000000142, 2.449293598294705330E-15, 20.00000000000000000 ) ) ;
#31147 = CYLINDRICAL_SURFACE ( 'NONE', #17628, 2.149999999999999023 ) ;
#31148 = CARTESIAN_POINT ( 'NONE',  ( 35.02499999726880020, 149.9369285172503510, -15.58253175000000823 ) ) ;
#31149 = CARTESIAN_POINT ( 'NONE',  ( -3.662846001190052991, 218.4274158808045740, 43.10113791807857098 ) ) ;
#31150 = CARTESIAN_POINT ( 'NONE',  ( 2.837346585668845567, -6.232092946297389524, -6.171287963165198676 ) ) ;
#31151 = CARTESIAN_POINT ( 'NONE',  ( -10.01549611932653860, 203.7984951890123284, 84.35113791807856387 ) ) ;
#31152 = EDGE_CURVE ( 'NONE', #11884, #5188, #9000, .T. ) ;
#31153 = CARTESIAN_POINT ( 'NONE',  ( -8.118202686958039038, 201.1607312380087080, 54.20113791807857240 ) ) ;
#31154 = DIRECTION ( 'NONE',  ( 1.000000000000000000, -0.000000000000000000, -0.000000000000000000 ) ) ;
#31155 = CARTESIAN_POINT ( 'NONE',  ( -7.456977232089471386, 217.1783343296987709, 23.94886208192143684 ) ) ;
#31156 = CARTESIAN_POINT ( 'NONE',  ( 9.984503880673420539, 210.2968891136705736, 27.84886208192143187 ) ) ;
#31157 = CARTESIAN_POINT ( 'NONE',  ( 76.99999999453763166, 155.0000000000000000, 14.49999999999999467 ) ) ;
#31158 = CARTESIAN_POINT ( 'NONE',  ( -12.00000000000000711, 207.0476921513413515, 72.50113791807856956 ) ) ;
#31159 = CARTESIAN_POINT ( 'NONE',  ( 7.984503880673485376, 204.3529502787953902, 86.15113791807856103 ) ) ;
#31160 = VECTOR ( 'NONE', #4159, 1000.000000000000000 ) ;
#31161 = CARTESIAN_POINT ( 'NONE',  ( -8.062137200540822946, 201.0835637161416400, 41.19886208192144039 ) ) ;
#31162 = DIRECTION ( 'NONE',  ( 0.1045284632676472814, 1.217938055844715641E-16, 0.9945218953682740670 ) ) ;
#31163 = VERTEX_POINT ( 'NONE', #1002 ) ;
#31164 = CARTESIAN_POINT ( 'NONE',  ( 12.00000000000000711, 207.0476921513415220, 54.99886208192144466 ) ) ;
#31165 = ORIENTED_EDGE ( 'NONE', *, *, #4518, .T. ) ;
#31166 = VERTEX_POINT ( 'NONE', #21945 ) ;
#31167 = CARTESIAN_POINT ( 'NONE',  ( 6.815830331203685866, 0.6619522098568483282, -6.171384342982615401 ) ) ;
#31168 = CARTESIAN_POINT ( 'NONE',  ( -7.897850199329715437, 1.533397866934075759, -7.634054012537968781 ) ) ;
#31169 = ORIENTED_EDGE ( 'NONE', *, *, #2461, .T. ) ;
#31170 = CARTESIAN_POINT ( 'NONE',  ( -4.984841277089726574, 200.2242689037092305, 39.05113791807855961 ) ) ;
#31171 = CARTESIAN_POINT ( 'NONE',  ( 82.31132485994280046, 169.2658477444273331, 4.635254915624208216 ) ) ;
#31172 = APPLICATION_CONTEXT ( 'automotive_design' ) ;
#31173 = CARTESIAN_POINT ( 'NONE',  ( -8.062137200540822946, 201.0835637161416400, 26.19886208192143684 ) ) ;
#31174 = CARTESIAN_POINT ( 'NONE',  ( 60.17499999726881299, 164.1591823560292198, 12.60653300113718167 ) ) ;
#31175 = ORIENTED_EDGE ( 'NONE', *, *, #6640, .T. ) ;
#31176 = DIRECTION ( 'NONE',  ( 0.5559124511712782990, 1.006869472843640094E-17, 0.8312408475482547798 ) ) ;
#31177 = VECTOR ( 'NONE', #14743, 1000.000000000000000 ) ;
#31178 = FILL_AREA_STYLE ('',( #31022 ) ) ;
#31179 = DIRECTION ( 'NONE',  ( 1.000000000000000000, 0.000000000000000000, 0.000000000000000000 ) ) ;
#31180 = CARTESIAN_POINT ( 'NONE',  ( -2.426778023690076225, 199.3768101843759553, 4.898862081921435241 ) ) ;
#31181 = EDGE_CURVE ( 'NONE', #29684, #22734, #31554, .T. ) ;
#31182 = VECTOR ( 'NONE', #27678, 1000.000000000000000 ) ;
#31183 = CARTESIAN_POINT ( 'NONE',  ( -6.220909254589537696, 198.5229672870051161, 45.05113791807855961 ) ) ;
#31184 = CARTESIAN_POINT ( 'NONE',  ( 79.81132485994281467, 159.8737954434937478, -14.99999999999993072 ) ) ;
#31185 = CARTESIAN_POINT ( 'NONE',  ( 6.139770520408368348, 198.4640165459539674, 26.45113791807856884 ) ) ;
#31186 = CARTESIAN_POINT ( 'NONE',  ( 10.00000000000000711, 207.0476921513415220, 102.9988620819214447 ) ) ;
#31187 = CIRCLE ( 'NONE', #5088, 11.99999999999998224 ) ;
#31188 = B_SPLINE_CURVE_WITH_KNOTS ( 'NONE', 3,
 ( #16127, #24296, #21247, #964, #11364, #29088 ),
 .UNSPECIFIED., .F., .F.,
 ( 4, 2, 4 ),
 ( 0.003605240635278502120, 0.004627368318297491422, 0.005649496001316481157 ),
 .UNSPECIFIED. ) ;
#31189 = APPLICATION_PROTOCOL_DEFINITION ( 'draft international standard', 'automotive_design', 1998, #28141 ) ;
#31190 = CARTESIAN_POINT ( 'NONE',  ( 8.000000000000008882, 207.0476921513415220, 96.99886208192143044 ) ) ;
#31191 = CARTESIAN_POINT ( 'NONE',  ( 86.20000000000000284, 142.6655632788954620, -8.961492836873480528 ) ) ;
#31192 = CARTESIAN_POINT ( 'NONE',  ( -5.047120108843199837, 5.746297884371392328, -0.1007566405101777279 ) ) ;
#31193 = CARTESIAN_POINT ( 'NONE',  ( 115.4999999999999858, 52.61186241335891367, 27.43481878086798176 ) ) ;
#31194 = CARTESIAN_POINT ( 'NONE',  ( 7.375838497908181246, 196.7627149292499666, 5.451137918078566180 ) ) ;
#31195 = CARTESIAN_POINT ( 'NONE',  ( 2.000000000000000000, 0.8865213383406723713, 1.535499999999998755 ) ) ;
#31196 = CARTESIAN_POINT ( 'NONE',  ( 55.97499999726881015, 169.8198683612136222, 4.815267126137181997 ) ) ;
#31197 = CARTESIAN_POINT ( 'NONE',  ( 10.00000000000000711, 206.9523078486586201, 56.00113791807856956 ) ) ;
#31198 = EDGE_CURVE ( 'NONE', #17833, #8245, #2555, .T. ) ;
#31199 = DIRECTION ( 'NONE',  ( -1.000000000000000000, 0.000000000000000000, 0.000000000000000000 ) ) ;
#31200 = AXIS2_PLACEMENT_3D ( 'NONE', #27349, #4015, #12190 ) ;
#31201 = CARTESIAN_POINT ( 'NONE',  ( 42.71132485994280614, 155.0000000000000000, 15.00000000000001243 ) ) ;
#31202 = CARTESIAN_POINT ( 'NONE',  ( 65.11132485994281183, 140.7341522555726669, 4.635254915624211769 ) ) ;
#31203 = CARTESIAN_POINT ( 'NONE',  ( 55.39999999453763024, 141.2096805137202580, 4.480746418436733158 ) ) ;
#31204 = ORIENTED_EDGE ( 'NONE', *, *, #13973, .T. ) ;
#31205 = CARTESIAN_POINT ( 'NONE',  ( -11.98450388067348804, 210.9467285061362247, 36.65113791807856103 ) ) ;
#31206 = CYLINDRICAL_SURFACE ( 'NONE', #14882, 2.149999999999985256 ) ;
#31207 = CARTESIAN_POINT ( 'NONE',  ( 9.984503880673420539, 210.2968891136705167, 9.848862081921435419 ) ) ;
#31208 = CARTESIAN_POINT ( 'NONE',  ( 6.938893903907228378E-15, 31.75426480542944319, -2.456200930618646971 ) ) ;
#31209 = VERTEX_POINT ( 'NONE', #29957 ) ;
#31210 = EDGE_CURVE ( 'NONE', #21928, #24566, #18851, .T. ) ;
#31211 = VECTOR ( 'NONE', #28835, 1000.000000000000000 ) ;
#31212 = CARTESIAN_POINT ( 'NONE',  ( -8.118202686958039038, 201.1607312380087080, 12.20113791807856707 ) ) ;
#31213 = CARTESIAN_POINT ( 'NONE',  ( -9.984503880673473830, 210.2968891136704315, 72.65113791807857524 ) ) ;
#31214 = AXIS2_PLACEMENT_3D ( 'NONE', #17585, #33259, #9925 ) ;
#31215 = ORIENTED_EDGE ( 'NONE', *, *, #14305, .F. ) ;
#31216 = CARTESIAN_POINT ( 'NONE',  ( 2.517493886309087436, 199.4062855549015865, 34.59886208192143897 ) ) ;
#31217 = CIRCLE ( 'NONE', #25215, 5.249999999999991118 ) ;
#31218 = CARTESIAN_POINT ( 'NONE',  ( 13.16654248868335664, -24.15255795529146710, -17.99999999999998579 ) ) ;
#31219 = VERTEX_POINT ( 'NONE', #3722 ) ;
#31220 = CARTESIAN_POINT ( 'NONE',  ( 8.000000000000008882, 206.9523078486586485, 11.00113791807856600 ) ) ;
#31221 = ADVANCED_FACE ( 'NONE', ( #28833 ), #16833, .F. ) ;
#31222 = CARTESIAN_POINT ( 'NONE',  ( -12.01549611932659722, 210.8513442034533227, 98.64886208192146455 ) ) ;
#31223 = CARTESIAN_POINT ( 'NONE',  ( 44.07499999726881157, 168.2552932293087906, 9.630534252274372875 ) ) ;
#31224 = ORIENTED_EDGE ( 'NONE', *, *, #12220, .F. ) ;
#31225 = CARTESIAN_POINT ( 'NONE',  ( 48.72499999726881725, 140.1801316387863778, -4.815267126137194431 ) ) ;
#31226 = CARTESIAN_POINT ( 'NONE',  ( 121.7736297201317370, 4.198250922590482048, 35.00001200000001234 ) ) ;
#31227 = CARTESIAN_POINT ( 'NONE',  ( 10.01549611932653860, 210.2015048109876716, 10.85113791807856387 ) ) ;
#31228 =( GEOMETRIC_REPRESENTATION_CONTEXT ( 3 ) GLOBAL_UNCERTAINTY_ASSIGNED_CONTEXT ( ( #31469 ) ) GLOBAL_UNIT_ASSIGNED_CONTEXT ( ( #23349, #10246, #33050 ) ) REPRESENTATION_CONTEXT ( 'NONE', 'WORKASPACE' ) );
#31229 = CARTESIAN_POINT ( 'NONE',  ( -8.062137200540822946, 201.0835637161416400, 83.19886208192143329 ) ) ;
#31230 = ADVANCED_FACE ( 'NONE', ( #3883 ), #9616, .T. ) ;
#31231 = CARTESIAN_POINT ( 'NONE',  ( 51.97499999726881725, 169.8198683612136222, 4.815267126137181997 ) ) ;
#31232 = CARTESIAN_POINT ( 'NONE',  ( -67.50001199999996970, 140.2468628165999007, -8.519561460567018685 ) ) ;
#31233 = CARTESIAN_POINT ( 'NONE',  ( 10.00000000000000711, 206.9523078486586201, 14.00113791807856600 ) ) ;
#31234 = LINE ( 'NONE', #21321, #31729 ) ;
#31235 = CARTESIAN_POINT ( 'NONE',  ( 64.79999999999998295, 167.3344367211045096, -8.961492836873482304 ) ) ;
#31236 = LINE ( 'NONE', #15883, #17065 ) ;
#31237 = DIRECTION ( 'NONE',  ( -1.000000000000000000, 0.000000000000000000, 0.000000000000000000 ) ) ;
#31238 = CARTESIAN_POINT ( 'NONE',  ( -8.062137200540920645, 212.9164362838581894, 81.80113791807858092 ) ) ;
#31239 = DIRECTION ( 'NONE',  ( 0.9945218953682747332, 1.280104479605073142E-17, 0.1045284632676402453 ) ) ;
#31240 = AXIS2_PLACEMENT_3D ( 'NONE', #3372, #32156, #29108 ) ;
#31241 = DIRECTION ( 'NONE',  ( -1.000000000000000000, -0.000000000000000000, -0.000000000000000000 ) ) ;
#31242 = CARTESIAN_POINT ( 'NONE',  ( 11.98450388067341876, 210.9467285061363953, 96.84886208192143897 ) ) ;
#31243 = CARTESIAN_POINT ( 'NONE',  ( 70.92499999726881299, 145.8408176439707802, -12.60653300113719588 ) ) ;
#31244 = EDGE_LOOP ( 'NONE', ( #6733, #5714 ) ) ;
#31245 = LINE ( 'NONE', #18288, #32049 ) ;
#31246 = CARTESIAN_POINT ( 'NONE',  ( 88.07499999726879025, 168.2552932293087906, 9.630534252274372875 ) ) ;
#31247 = CARTESIAN_POINT ( 'NONE',  ( -9.680171189290831535, 214.0920067884431148, 93.80113791807858092 ) ) ;
#31248 = FACE_OUTER_BOUND ( 'NONE', #3439, .T. ) ;
#31249 = ORIENTED_EDGE ( 'NONE', *, *, #8459, .T. ) ;
#31250 = CARTESIAN_POINT ( 'NONE',  ( -8.118202686958138514, 212.8392687619910930, 86.79886208192142760 ) ) ;
#31251 = CARTESIAN_POINT ( 'NONE',  ( -0.05014649552828442242, 219.6175466908591716, 24.24886208192144110 ) ) ;
#31252 = DIRECTION ( 'NONE',  ( 0.000000000000000000, 0.000000000000000000, -1.000000000000000000 ) ) ;
#31253 = CARTESIAN_POINT ( 'NONE',  ( -6.139770520408369237, 215.5359834540460042, 45.95113791807857950 ) ) ;
#31254 = EDGE_LOOP ( 'NONE', ( #6001, #20409, #7754 ) ) ;
#31255 = CARTESIAN_POINT ( 'NONE',  ( -6.444103211790928043, 202.2591342207265939, 5.198862081921435063 ) ) ;
#31256 = EDGE_CURVE ( 'NONE', #18960, #4076, #31372, .T. ) ;
#31257 = ADVANCED_FACE ( 'NONE', ( #27058 ), #26467, .T. ) ;
#31258 = CARTESIAN_POINT ( 'NONE',  ( 125.5000000000000000, 78.52640161467553526, 73.43303922622362734 ) ) ;
#31259 = ORIENTED_EDGE ( 'NONE', *, *, #32404, .T. ) ;
#31260 = CARTESIAN_POINT ( 'NONE',  ( 6.444103211790928043, 211.7408657792734061, 90.69886208192143329 ) ) ;
#31261 = VECTOR ( 'NONE', #22789, 1000.000000000000227 ) ;
#31262 = ORIENTED_EDGE ( 'NONE', *, *, #24317, .T. ) ;
#31263 = PRODUCT_DEFINITION ( 'UNKNOWN', '', #21887, #32239 ) ;
#31264 = EDGE_CURVE ( 'NONE', #24271, #7757, #11558, .T. ) ;
#31265 = CARTESIAN_POINT ( 'NONE',  ( 6.444103211791042618, 202.2591342207267644, 26.30113791807856316 ) ) ;
#31266 = ORIENTED_EDGE ( 'NONE', *, *, #32471, .T. ) ;
#31267 = PLANE ( 'NONE',  #13427 ) ;
#31268 = EDGE_CURVE ( 'NONE', #21649, #17667, #19226, .T. ) ;
#31269 = CARTESIAN_POINT ( 'NONE',  ( 85.62499999726880162, 171.3844434931184253, -7.942151717890132712E-15 ) ) ;
#31270 = DIRECTION ( 'NONE',  ( 1.000000000000000000, 0.000000000000000000, 0.000000000000000000 ) ) ;
#31271 = CARTESIAN_POINT ( 'NONE',  ( 2.517493886308900919, 214.5937144450984420, 91.40113791807857524 ) ) ;
#31272 = DIRECTION ( 'NONE',  ( 1.000000000000000000, 0.000000000000000000, 0.000000000000000000 ) ) ;
#31273 = PRESENTATION_LAYER_ASSIGNMENT (  '', '', ( #17666 ) ) ;
#31274 = SURFACE_STYLE_FILL_AREA ( #2656 ) ;
#31275 = CARTESIAN_POINT ( 'NONE',  ( 46.50000000000000000, 155.0000000000000000, -14.50000000000000711 ) ) ;
#31276 = CARTESIAN_POINT ( 'NONE',  ( -6.444103211790928043, 202.2591342207265939, 59.19886208192144750 ) ) ;
#31277 = FACE_OUTER_BOUND ( 'NONE', #4500, .T. ) ;
#31278 = CARTESIAN_POINT ( 'NONE',  ( 49.72499999726881725, 169.8198683612136222, 4.815267126137181997 ) ) ;
#31279 = CARTESIAN_POINT ( 'NONE',  ( 10.01549611932653860, 210.2015048109876716, 4.851137918078564759 ) ) ;
#31280 = CARTESIAN_POINT ( 'NONE',  ( 0.000000000000000000, 0.000000000000000000, -10.00000000000000000 ) ) ;
#31281 = CARTESIAN_POINT ( 'NONE',  ( 58.72499999726881015, 140.1801316387863778, -4.815267126137194431 ) ) ;
#31282 = CARTESIAN_POINT ( 'NONE',  ( 67.27499999726879309, 149.9369285172503510, -15.58253175000000823 ) ) ;
#31283 = CARTESIAN_POINT ( 'NONE',  ( -7.456977232089304408, 196.8216656703010301, 72.05113791807858092 ) ) ;
#31284 = CARTESIAN_POINT ( 'NONE',  ( 32.50000000000000000, 155.0000000000000000, -6.938893903907228378E-15 ) ) ;
#31285 = CARTESIAN_POINT ( 'NONE',  ( -9.736236675707914401, 199.9851607334237542, 6.201137918078565292 ) ) ;
#31286 = CARTESIAN_POINT ( 'NONE',  ( 10.01549611932653860, 210.2015048109876716, 91.85113791807856387 ) ) ;
#31287 = DIRECTION ( 'NONE',  ( 0.000000000000000000, 0.000000000000000000, 1.000000000000000000 ) ) ;
#31288 = CARTESIAN_POINT ( 'NONE',  ( -0.05014649552828442242, 219.6175466908591716, 51.24886208192143755 ) ) ;
#31289 = CARTESIAN_POINT ( 'NONE',  ( -3.044812012439970683, 197.4746971517856196, 61.89886208192143613 ) ) ;
#31290 = CARTESIAN_POINT ( 'NONE',  ( 12.01549611932652972, 210.8513442034534933, 91.85113791807857808 ) ) ;
#31291 = CARTESIAN_POINT ( 'NONE',  ( -67.50001199999999812, 171.1317437780266459, -5.477666192157138347 ) ) ;
#31292 = CARTESIAN_POINT ( 'NONE',  ( 6.220909254589536808, 215.4770327129947702, 10.55113791807856138 ) ) ;
#31293 = CARTESIAN_POINT ( 'NONE',  ( 6.220909254589681581, 198.5229672870052582, 82.44886208192141908 ) ) ;
#31294 = VERTEX_POINT ( 'NONE', #16998 ) ;
#31295 = CARTESIAN_POINT ( 'NONE',  ( -9.680171189290716072, 199.9079932115567146, 80.19886208192143329 ) ) ;
#31296 = CARTESIAN_POINT ( 'NONE',  ( -9.984503880673473830, 210.2968891136704315, 99.65113791807853261 ) ) ;
#31297 = ORIENTED_EDGE ( 'NONE', *, *, #978, .T. ) ;
#31298 = DIRECTION ( 'NONE',  ( 0.000000000000000000, 0.000000000000000000, 1.000000000000000000 ) ) ;
#31299 = CARTESIAN_POINT ( 'NONE',  ( 2.517493886309087436, 199.4062855549015865, 61.59886208192145318 ) ) ;
#31300 = ORIENTED_EDGE ( 'NONE', *, *, #5768, .T. ) ;
#31301 = CARTESIAN_POINT ( 'NONE',  ( 76.82499999726881867, 141.7447067706911810, -9.630534252274387086 ) ) ;
#31302 = CARTESIAN_POINT ( 'NONE',  ( 0.000000000000000000, 0.000000000000000000, -2.899999999999999911 ) ) ;
#31303 = CARTESIAN_POINT ( 'NONE',  ( -57.84141927132884575, 194.9260988872778171, 2.433575273292319707 ) ) ;
#31304 = CARTESIAN_POINT ( 'NONE',  ( 62.62499999726881583, 138.6155565068815463, -3.929120461958505118E-15 ) ) ;
#31305 = CARTESIAN_POINT ( 'NONE',  ( -7.894955577759523280, 1.603085139988202901, -7.593799241562120272 ) ) ;
#31306 = CARTESIAN_POINT ( 'NONE',  ( -3.044812012439970683, 197.4746971517856196, 55.89886208192143613 ) ) ;
#31307 = ORIENTED_EDGE ( 'NONE', *, *, #3214, .T. ) ;
#31308 = DIRECTION ( 'NONE',  ( -0.000000000000000000, -0.000000000000000000, -1.000000000000000000 ) ) ;
#31309 =( NAMED_UNIT ( * ) PLANE_ANGLE_UNIT ( ) SI_UNIT ( $, .RADIAN. ) );
#31310 = LINE ( 'NONE', #15626, #31909 ) ;
#31311 = CARTESIAN_POINT ( 'NONE',  ( 8.000000000000008882, 207.0476921513415220, 36.99886208192143044 ) ) ;
#31312 = CARTESIAN_POINT ( 'NONE',  ( 9.984503880673470277, 203.7031108863295401, 77.15113791807857524 ) ) ;
#31313 = DIRECTION ( 'NONE',  ( 0.1045284632676479336, 1.217938055844715641E-16, 0.9945218953682739560 ) ) ;
#31314 = CARTESIAN_POINT ( 'NONE',  ( -3.044812012440131443, 216.5253028482142952, 61.10113791807857098 ) ) ;
#31315 = CARTESIAN_POINT ( 'NONE',  ( 10.01549611932653860, 210.2015048109876716, 28.85113791807855677 ) ) ;
#31316 = CARTESIAN_POINT ( 'NONE',  ( -4.903702542908602524, 213.8346818373418898, 18.95113791807856529 ) ) ;
#31317 = CARTESIAN_POINT ( 'NONE',  ( 43.78867513459481842, 155.0000000000000000, 15.00000000000001243 ) ) ;
#31318 = CARTESIAN_POINT ( 'NONE',  ( 54.30000000000001137, -88.00000000000000000, -20.00000000000000000 ) ) ;
#31319 = CARTESIAN_POINT ( 'NONE',  ( 35.42499999726880588, 168.2552932293087906, -9.630534252274387086 ) ) ;
#31320 = CARTESIAN_POINT ( 'NONE',  ( 0.05014649552807549926, 219.6175466908591716, 43.25113791807856245 ) ) ;
#31321 = CYLINDRICAL_SURFACE ( 'NONE', #1008, 18.00000000000000355 ) ;
#31322 = CARTESIAN_POINT ( 'NONE',  ( -8.118202686958039038, 201.1607312380087080, 87.20113791807858661 ) ) ;
#31323 = CARTESIAN_POINT ( 'NONE',  ( 9.984503880673473830, 203.7031108863295401, 56.15113791807856813 ) ) ;
#31324 = CARTESIAN_POINT ( 'NONE',  ( -12.01549611932659722, 210.8513442034533227, 23.64886208192143968 ) ) ;
#31325 = CARTESIAN_POINT ( 'NONE',  ( -6.220909254589682469, 215.4770327129947134, 23.94886208192143329 ) ) ;
#31326 = CARTESIAN_POINT ( 'NONE',  ( 81.49999999453761745, 139.7537977485451393, -4.138211985947621020E-15 ) ) ;
#31327 = CARTESIAN_POINT ( 'NONE',  ( -12.00000000000000711, 207.0476921513413515, 66.50113791807856956 ) ) ;
#31328 = CARTESIAN_POINT ( 'NONE',  ( -0.05014649552807731031, 198.5883022060938572, 89.75113791807858377 ) ) ;
#31329 = CARTESIAN_POINT ( 'NONE',  ( 6.220909254589681581, 198.5229672870052582, 52.44886208192143329 ) ) ;
#31330 = DIRECTION ( 'NONE',  ( -1.000000000000000000, 0.000000000000000000, 0.000000000000000000 ) ) ;
#31331 = ORIENTED_EDGE ( 'NONE', *, *, #18464, .F. ) ;
#31332 = CARTESIAN_POINT ( 'NONE',  ( -3.662846001189865142, 195.5725841191952838, 55.89886208192143613 ) ) ;
#31333 = VERTEX_POINT ( 'NONE', #14445 ) ;
#31334 = ORIENTED_EDGE ( 'NONE', *, *, #12823, .T. ) ;
#31335 = CYLINDRICAL_SURFACE ( 'NONE', #11849, 12.00000000000000355 ) ;
#31336 = DIRECTION ( 'NONE',  ( -0.000000000000000000, -0.000000000000000000, 1.000000000000000000 ) ) ;
#31337 = CARTESIAN_POINT ( 'NONE',  ( 4.984841277089725686, 213.7757310962907411, 40.55113791807856671 ) ) ;
#31338 =( BOUNDED_CURVE ( )  B_SPLINE_CURVE ( 2, ( #12652, #2782, #15713, #20671, #18110, #15546, #4655, #26114, #7894, #5158, #18275 ),
 .UNSPECIFIED., .F., .T. ) 
 B_SPLINE_CURVE_WITH_KNOTS ( ( 3, 2, 2, 2, 2, 3 ),
 ( 0.8035714285714286031, 0.8071428571428571619, 0.8107142857142857206, 0.8142857142857143904, 0.8178571428571429491, 0.8214285714285715079 ),
 .UNSPECIFIED. ) 
 CURVE ( )  GEOMETRIC_REPRESENTATION_ITEM ( )  RATIONAL_B_SPLINE_CURVE ( ( 1.000000000000000000, 0.9510565162951534202, 1.000000000000000000, 0.9510565162951534202, 1.000000000000000000, 0.9510565162951534202, 1.000000000000000000, 0.9510565162951534202, 1.000000000000000000, 0.9510565162951518658, 1.000000000000001554 ) ) 
 REPRESENTATION_ITEM ( '' )  );
#31339 = CARTESIAN_POINT ( 'NONE',  ( 77.50000000000000000, 155.0000000000000000, -6.938893903907228378E-15 ) ) ;
#31340 = EDGE_CURVE ( 'NONE', #19849, #12770, #24839, .T. ) ;
#31341 = CARTESIAN_POINT ( 'NONE',  ( 3.135527875058981895, 197.5041725223112792, 25.59886208192143897 ) ) ;
#31342 = CARTESIAN_POINT ( 'NONE',  ( 64.27499999726880731, 160.0630714827496206, 15.58253174999999224 ) ) ;
#31343 = ORIENTED_EDGE ( 'NONE', *, *, #8640, .T. ) ;
#31344 = DIRECTION ( 'NONE',  ( 1.000000000000000000, -0.000000000000000000, -0.000000000000000000 ) ) ;
#31345 =( NAMED_UNIT ( * ) PLANE_ANGLE_UNIT ( ) SI_UNIT ( $, .RADIAN. ) );
#31346 = CYLINDRICAL_SURFACE ( 'NONE', #3845, 15.00000000000001776 ) ;
#31347 = CARTESIAN_POINT ( 'NONE',  ( -2.517493886309087880, 214.5937144450984135, 9.098862081921435419 ) ) ;
#31348 = CARTESIAN_POINT ( 'NONE',  ( -8.118202686958039038, 201.1607312380087080, 45.20113791807857240 ) ) ;
#31349 = FACE_OUTER_BOUND ( 'NONE', #31734, .T. ) ;
#31350 = CARTESIAN_POINT ( 'NONE',  ( 3.135527875058820690, 216.4958274776887492, 31.40113791807857524 ) ) ;
#31351 = CYLINDRICAL_SURFACE ( 'NONE', #23346, 0.9999999999999953371 ) ;
#31352 = PRODUCT_CONTEXT ( 'NONE', #23568, 'mechanical' ) ;
#31353 = CARTESIAN_POINT ( 'NONE',  ( -2.517493886309087880, 214.5937144450984135, 93.09886208192145318 ) ) ;
#31354 = CARTESIAN_POINT ( 'NONE',  ( 84.80000000000001137, 167.3344367211045096, -8.961492836873482304 ) ) ;
#31355 =( NAMED_UNIT ( * ) SI_UNIT ( $, .STERADIAN. ) SOLID_ANGLE_UNIT ( ) );
#31356 = DIRECTION ( 'NONE',  ( 0.000000000000000000, 0.000000000000000000, 1.000000000000000000 ) ) ;
#31357 = CARTESIAN_POINT ( 'NONE',  ( 9.736236675707914401, 214.0148392665762458, 7.701137918078567068 ) ) ;
#31358 = CARTESIAN_POINT ( 'NONE',  ( 63.78867513459482552, 155.0000000000000000, 15.00000000000001243 ) ) ;
#31359 = CARTESIAN_POINT ( 'NONE',  ( 56.67499999726881299, 141.7447067706911810, 9.630534252274376428 ) ) ;
#31360 = CARTESIAN_POINT ( 'NONE',  ( 3.135527875058820690, 216.4958274776887492, 58.40113791807857524 ) ) ;
#31361 = CARTESIAN_POINT ( 'NONE',  ( -0.05014649552810635652, 196.4853777576173002, 26.75113791807856956 ) ) ;
#31362 = AXIS2_PLACEMENT_3D ( 'NONE', #1598, #21866, #4145 ) ;
#31363 = CARTESIAN_POINT ( 'NONE',  ( 87.12499999726880162, 155.0000000000000000, -15.58253175000000823 ) ) ;
#31364 = CIRCLE ( 'NONE', #25372, 37.00000000000000711 ) ;
#31365 = CARTESIAN_POINT ( 'NONE',  ( 54.78867513459483263, 155.0000000000000000, -15.00000000000002487 ) ) ;
#31366 = CARTESIAN_POINT ( 'NONE',  ( 3.044812012439969795, 216.5253028482143520, 3.398862081921434797 ) ) ;
#31367 = CARTESIAN_POINT ( 'NONE',  ( 59.09999999453762598, 150.2886644046228639, 14.49999999999999645 ) ) ;
#31368 = ORIENTED_EDGE ( 'NONE', *, *, #1176, .F. ) ;
#31369 = CARTESIAN_POINT ( 'NONE',  ( 12.00000000000000711, 206.9523078486586485, 38.00113791807857666 ) ) ;
#31370 = CARTESIAN_POINT ( 'NONE',  ( -9.984503880673420539, 203.7031108863293980, 23.34886208192142831 ) ) ;
#31371 = CARTESIAN_POINT ( 'NONE',  ( 32.50000000000000000, 155.0000000000000000, -6.938893903907228378E-15 ) ) ;
#31372 = CIRCLE ( 'NONE', #4165, 5.249999999999997335 ) ;
#31373 = EDGE_LOOP ( 'NONE', ( #7790, #29691, #33626, #1744 ) ) ;
#31374 = CARTESIAN_POINT ( 'NONE',  ( 6.139770520408368348, 198.4640165459539674, 71.45113791807857240 ) ) ;
#31375 = ORIENTED_EDGE ( 'NONE', *, *, #18979, .T. ) ;
#31376 = CARTESIAN_POINT ( 'NONE',  ( -10.00000000000019362, 205.9534653805592654, 104.4507591396482127 ) ) ;
#31377 = DIRECTION ( 'NONE',  ( 1.000000000000000000, -0.000000000000000000, -0.000000000000000000 ) ) ;
#31378 = ORIENTED_EDGE ( 'NONE', *, *, #31107, .T. ) ;
#31379 = CARTESIAN_POINT ( 'NONE',  ( 6.444103211791042618, 202.2591342207267644, 17.30113791807856671 ) ) ;
#31380 = EDGE_CURVE ( 'NONE', #889, #1694, #25941, .T. ) ;
#31381 = PRESENTATION_LAYER_ASSIGNMENT (  '', '', ( #12336 ) ) ;
#31382 = CARTESIAN_POINT ( 'NONE',  ( -3.753561863808878130, 218.3979405102790281, 99.09886208192145318 ) ) ;
#31383 = CARTESIAN_POINT ( 'NONE',  ( 44.77499999726881441, 140.1801316387863778, 4.815267126137185549 ) ) ;
#31384 = EDGE_LOOP ( 'NONE', ( #22747, #20096, #15540, #31499 ) ) ;
#31385 = CARTESIAN_POINT ( 'NONE',  ( 53.32499999726881157, 164.1591823560292198, -12.60653300113719766 ) ) ;
#31386 = LINE ( 'NONE', #33609, #12616 ) ;
#31387 = CARTESIAN_POINT ( 'NONE',  ( -6.139770520408369237, 215.5359834540460042, 3.951137918078566180 ) ) ;
#31388 = VECTOR ( 'NONE', #19051, 1000.000000000000000 ) ;
#31389 = CARTESIAN_POINT ( 'NONE',  ( 8.118202686958138514, 201.1607312380088501, 85.29886208192144181 ) ) ;
#31390 = CARTESIAN_POINT ( 'NONE',  ( 50.47499999726880304, 149.9369285172503510, 15.58253174999999580 ) ) ;
#31391 = DIRECTION ( 'NONE',  ( 1.000000000000000000, -0.000000000000000000, -0.000000000000000000 ) ) ;
#31392 = CARTESIAN_POINT ( 'NONE',  ( 3.135527875058820690, 216.4958274776887492, 10.40113791807856636 ) ) ;
#31393 = CARTESIAN_POINT ( 'NONE',  ( 43.88867513459482694, 150.1262045565064227, 15.00000000000001599 ) ) ;
#31394 = AXIS2_PLACEMENT_3D ( 'NONE', #32790, #32120, #27345 ) ;
#31395 = ADVANCED_FACE ( 'NONE', ( #25172 ), #17345, .F. ) ;
#31396 = CARTESIAN_POINT ( 'NONE',  ( 66.10000000000000853, 141.2096805137202580, -4.480746418436742040 ) ) ;
#31397 = CARTESIAN_POINT ( 'NONE',  ( -10.01549611932653860, 203.7984951890123284, 99.35113791807857808 ) ) ;
#31398 = CARTESIAN_POINT ( 'NONE',  ( -58.50000000000002132, 185.0000000000000000, 2.500000000000000000 ) ) ;
#31399 = CARTESIAN_POINT ( 'NONE',  ( 3.044812012440130555, 197.4746971517856764, 80.60113791807857808 ) ) ;
#31400 = CARTESIAN_POINT ( 'NONE',  ( 85.78867513459481131, 155.0000000000000000, 15.00000000000001243 ) ) ;
#31401 = CARTESIAN_POINT ( 'NONE',  ( 39.37499999726880873, 155.0000000000000000, -15.58253175000000823 ) ) ;
#31402 = CARTESIAN_POINT ( 'NONE',  ( 9.680171189290716072, 214.0920067884432854, 93.69886208192144750 ) ) ;
#31403 = CARTESIAN_POINT ( 'NONE',  ( 71.92499999726881299, 164.1591823560292198, 12.60653300113718167 ) ) ;
#31404 = ORIENTED_EDGE ( 'NONE', *, *, #5404, .T. ) ;
#31405 = DIRECTION ( 'NONE',  ( 0.000000000000000000, 0.000000000000000000, -1.000000000000000000 ) ) ;
#31406 = CARTESIAN_POINT ( 'NONE',  ( 41.69999999453762740, 142.6655632788954620, -8.961492836873480528 ) ) ;
#31407 = CARTESIAN_POINT ( 'NONE',  ( 7.375838497908012492, 217.2372850707501186, 3.548862081921434264 ) ) ;
#31408 = AXIS2_PLACEMENT_3D ( 'NONE', #9101, #29897, #19100 ) ;
#31409 = EDGE_CURVE ( 'NONE', #10267, #2381, #4704, .T. ) ;
#31410 = DIRECTION ( 'NONE',  ( 0.000000000000000000, -1.224646799147353207E-16, 1.000000000000000000 ) ) ;
#31411 = CONICAL_SURFACE ( 'NONE', #30857, 32.00000000000000000, 0.1047197551197016768 ) ;
#31412 = VERTEX_POINT ( 'NONE', #9333 ) ;
#31413 = CARTESIAN_POINT ( 'NONE',  ( -3.135527875058982783, 216.4958274776886924, 96.09886208192143897 ) ) ;
#31414 = CARTESIAN_POINT ( 'NONE',  ( 11.98450388067341876, 210.9467285061363953, 18.84886208192143187 ) ) ;
#31415 = LINE ( 'NONE', #8084, #31685 ) ;
#31416 = CARTESIAN_POINT ( 'NONE',  ( 8.062137200540920645, 201.0835637161417822, 38.30113791807857382 ) ) ;
#31417 = ADVANCED_FACE ( 'NONE', ( #17682 ), #28943, .F. ) ;
#31418 = VERTEX_POINT ( 'NONE', #20412 ) ;
#31419 = CARTESIAN_POINT ( 'NONE',  ( -10.00000000000000711, 206.9523078486584495, 104.4988620819214447 ) ) ;
#31420 = AXIS2_PLACEMENT_3D ( 'NONE', #18947, #13832, #8885 ) ;
#31421 = DIRECTION ( 'NONE',  ( 0.000000000000000000, 0.000000000000000000, -1.000000000000000000 ) ) ;
#31422 = ORIENTED_EDGE ( 'NONE', *, *, #15438, .F. ) ;
#31423 = CARTESIAN_POINT ( 'NONE',  ( 6.444103211790928043, 211.7408657792734061, 93.69886208192144750 ) ) ;
#31424 = CARTESIAN_POINT ( 'NONE',  ( 7.984503880673485376, 204.3529502787953902, 32.15113791807857524 ) ) ;
#31425 = CARTESIAN_POINT ( 'NONE',  ( 56.11132485994280472, 169.2658477444273331, -4.635254915624224203 ) ) ;
#31426 = ORIENTED_EDGE ( 'NONE', *, *, #2946, .F. ) ;
#31427 = DIRECTION ( 'NONE',  ( 0.000000000000000000, 0.000000000000000000, -1.000000000000000000 ) ) ;
#31428 = AXIS2_PLACEMENT_3D ( 'NONE', #6611, #19723, #27389 ) ;
#31429 = CARTESIAN_POINT ( 'NONE',  ( 36.37499999726881583, 155.0000000000000000, 15.58253174999999402 ) ) ;
#31430 = DIRECTION ( 'NONE',  ( 0.000000000000000000, 0.000000000000000000, 1.000000000000000000 ) ) ;
#31431 = CARTESIAN_POINT ( 'NONE',  ( 6.444103211791042618, 202.2591342207267644, 89.30113791807858092 ) ) ;
#31432 = CIRCLE ( 'NONE', #16728, 2.428571428571428381 ) ;
#31433 = FILL_AREA_STYLE_COLOUR ( '', #21406 ) ;
#31434 = CARTESIAN_POINT ( 'NONE',  ( 50.29999999999999716, 146.4771138417591203, -11.73074641843674470 ) ) ;
#31435 = CARTESIAN_POINT ( 'NONE',  ( -8.015496119326597224, 209.5516654185217362, 59.64886208192145034 ) ) ;
#31436 = FACE_OUTER_BOUND ( 'NONE', #15567, .T. ) ;
#31437 = AXIS2_PLACEMENT_3D ( 'NONE', #4479, #19651, #30041 ) ;
#31438 = ADVANCED_FACE ( 'NONE', ( #30288 ), #1840, .T. ) ;
#31439 = EDGE_CURVE ( 'NONE', #1785, #21688, #22650, .T. ) ;
#31440 = AXIS2_PLACEMENT_3D ( 'NONE', #32349, #26906, #16013 ) ;
#31441 = CARTESIAN_POINT ( 'NONE',  ( 50.32499999726881157, 145.8408176439707802, 12.60653300113718345 ) ) ;
#31442 = DIRECTION ( 'NONE',  ( 1.000000000000000000, -0.000000000000000000, -0.000000000000000000 ) ) ;
#31443 = CARTESIAN_POINT ( 'NONE',  ( -6.874999999999995559, 4.690970937165706900, -7.298562697733101068 ) ) ;
#31444 = CARTESIAN_POINT ( 'NONE',  ( 66.22499999726879594, 149.9369285172503510, 15.58253174999999580 ) ) ;
#31445 = CARTESIAN_POINT ( 'NONE',  ( 70.37499999726881583, 155.0000000000000000, 15.58253174999999402 ) ) ;
#31446 = CARTESIAN_POINT ( 'NONE',  ( -12.00000000000000711, 207.0476921513413515, 69.50113791807856956 ) ) ;
#31447 = CARTESIAN_POINT ( 'NONE',  ( 49.31132485994280756, 140.7341522555726669, -4.635254915624220651 ) ) ;
#31448 = EDGE_CURVE ( 'NONE', #26131, #30720, #28249, .T. ) ;
#31449 = CARTESIAN_POINT ( 'NONE',  ( 6.220909254589536808, 215.4770327129947987, 85.55113791807856671 ) ) ;
#31450 = DIRECTION ( 'NONE',  ( 0.000000000000000000, 0.000000000000000000, -1.000000000000000000 ) ) ;
#31451 = CARTESIAN_POINT ( 'NONE',  ( -9.736236675708031640, 214.0148392665760753, 50.79886208192143471 ) ) ;
#31452 = CARTESIAN_POINT ( 'NONE',  ( 8.062137200540822946, 212.9164362838583315, 63.69886208192143329 ) ) ;
#31453 = CARTESIAN_POINT ( 'NONE',  ( 3.662846001190051659, 195.5725841191953691, 92.60113791807857808 ) ) ;
#31454 = CARTESIAN_POINT ( 'NONE',  ( 68.51132485994280330, 163.8167787843871110, 12.13525491562421621 ) ) ;
#31455 = CIRCLE ( 'NONE', #20016, 37.00000000000000711 ) ;
#31456 = CARTESIAN_POINT ( 'NONE',  ( 10.00000000000000711, 206.9523078486586201, 14.00113791807856600 ) ) ;
#31457 = ADVANCED_FACE ( 'NONE', ( #7125 ), #33188, .F. ) ;
#31458 = CARTESIAN_POINT ( 'NONE',  ( -10.00000000000000711, 206.9523078486584495, 77.49886208192144466 ) ) ;
#31459 = CIRCLE ( 'NONE', #9118, 2.149999999999985256 ) ;
#31460 = ORIENTED_EDGE ( 'NONE', *, *, #24920, .F. ) ;
#31461 = CARTESIAN_POINT ( 'NONE',  ( -10.00000000000000711, 207.0476921513413515, 96.50113791807856956 ) ) ;
#31462 = ORIENTED_EDGE ( 'NONE', *, *, #25842, .F. ) ;
#31463 = CARTESIAN_POINT ( 'NONE',  ( -2.517493886309087880, 214.5937144450984135, 57.09886208192145318 ) ) ;
#31464 = ORIENTED_EDGE ( 'NONE', *, *, #17275, .F. ) ;
#31465 = VECTOR ( 'NONE', #10163, 1000.000000000000000 ) ;
#31466 = CARTESIAN_POINT ( 'NONE',  ( 76.32499999726881867, 145.8408176439707802, 12.60653300113718345 ) ) ;
#31467 = CARTESIAN_POINT ( 'NONE',  ( 4.000000000000000000, -1.759474945355381958, 3.047500000000001208 ) ) ;
#31468 = FACE_OUTER_BOUND ( 'NONE', #19835, .T. ) ;
#31469 = UNCERTAINTY_MEASURE_WITH_UNIT (LENGTH_MEASURE( 1.000000000000000082E-05 ), #23349, 'distance_accuracy_value', 'NONE');
#31470 = CARTESIAN_POINT ( 'NONE',  ( 69.42499999726881299, 168.2552932293087906, -9.630534252274385310 ) ) ;
#31471 = CARTESIAN_POINT ( 'NONE',  ( -2.517493886308901807, 199.4062855549015012, 56.90113791807858235 ) ) ;
#31472 =( NAMED_UNIT ( * ) SI_UNIT ( $, .STERADIAN. ) SOLID_ANGLE_UNIT ( ) );
#31473 = CARTESIAN_POINT ( 'NONE',  ( 107.5000000000000000, 155.0000000000000000, -6.938893903907228378E-15 ) ) ;
#31474 = CARTESIAN_POINT ( 'NONE',  ( 92.60756280994512224, 155.0000000000000000, 12.10452846326762177 ) ) ;
#31475 = CARTESIAN_POINT ( 'NONE',  ( -0.05014649552828365914, 215.4116977939061144, 33.24886208192144466 ) ) ;
#31476 = CONICAL_SURFACE ( 'NONE', #27119, 7.500000000000001776, 0.8594454914424796144 ) ;
#31477 = CARTESIAN_POINT ( 'NONE',  ( 3.135527875058820690, 216.4958274776887492, 76.40113791807857524 ) ) ;
#31478 = CARTESIAN_POINT ( 'NONE',  ( 0.000000000000000000, 0.000000000000000000, 0.000000000000000000 ) ) ;
#31479 = CARTESIAN_POINT ( 'NONE',  ( 6.139770520408368348, 198.4640165459539674, 59.45113791807855819 ) ) ;
#31480 = EDGE_CURVE ( 'NONE', #5010, #5750, #11899, .T. ) ;
#31481 = CIRCLE ( 'NONE', #32530, 0.9999999999999941158 ) ;
#31482 = CARTESIAN_POINT ( 'NONE',  ( -8.118202686958039038, 201.1607312380087080, 30.20113791807856884 ) ) ;
#31483 = CARTESIAN_POINT ( 'NONE',  ( 6.500168698208129925, 211.6636982574063381, 10.70113791807856529 ) ) ;
#31484 = CARTESIAN_POINT ( 'NONE',  ( 120.8017490774095535, -3.226370279868274515, 35.00001200000000523 ) ) ;
#31485 = CARTESIAN_POINT ( 'NONE',  ( -5.619193549421041212, 4.261310591078285803, -5.875704392894027350 ) ) ;
#31486 = CARTESIAN_POINT ( 'NONE',  ( 42.42499999726881299, 141.7447067706911810, 9.630534252274376428 ) ) ;
#31487 = CARTESIAN_POINT ( 'NONE',  ( -0.05014649552807705357, 194.3824533091408000, 35.75113791807857666 ) ) ;
#31488 = CARTESIAN_POINT ( 'NONE',  ( 5.000000000000001776, 6.123233995736768255E-16, -9.974600000000000577 ) ) ;
#31489 = CARTESIAN_POINT ( 'NONE',  ( -0.05014649552810635652, 196.4853777576173002, 83.75113791807856956 ) ) ;
#31490 = CARTESIAN_POINT ( 'NONE',  ( -8.062137200540920645, 212.9164362838581894, 60.80113791807857382 ) ) ;
#31491 = CIRCLE ( 'NONE', #14601, 19.99999999999998934 ) ;
#31492 = CARTESIAN_POINT ( 'NONE',  ( 7.456977232089471386, 196.8216656703012006, 25.44886208192143684 ) ) ;
#31493 = CARTESIAN_POINT ( 'NONE',  ( -10.01549611932659545, 210.2015048109875011, 26.64886208192143258 ) ) ;
#31494 = CARTESIAN_POINT ( 'NONE',  ( 81.29999999453762882, 142.6655632788954620, 8.961492836873471646 ) ) ;
#31495 = CARTESIAN_POINT ( 'NONE',  ( 0.05014649552807549926, 219.6175466908591716, 64.25113791807856956 ) ) ;
#31496 = CARTESIAN_POINT ( 'NONE',  ( 2.517493886308900919, 214.5937144450984420, 85.40113791807856103 ) ) ;
#31497 = CARTESIAN_POINT ( 'NONE',  ( -0.05014649552828403384, 217.5146222423826714, 54.24886208192142334 ) ) ;
#31498 = CARTESIAN_POINT ( 'NONE',  ( 49.68867513459482410, 159.8737954434933499, 15.00000000000019895 ) ) ;
#31499 = ORIENTED_EDGE ( 'NONE', *, *, #5023, .T. ) ;
#31500 = CARTESIAN_POINT ( 'NONE',  ( -9.736236675708031640, 214.0148392665760753, 56.79886208192143471 ) ) ;
#31501 = VERTEX_POINT ( 'NONE', #9852 ) ;
#31502 = ORIENTED_EDGE ( 'NONE', *, *, #30827, .F. ) ;
#31503 = LINE ( 'NONE', #8330, #6988 ) ;
#31504 = VECTOR ( 'NONE', #9545, 1000.000000000000000 ) ;
#31505 = CARTESIAN_POINT ( 'NONE',  ( -7.894787914004607998, 0.7647108141804108694, -7.591390474663421095 ) ) ;
#31506 = CARTESIAN_POINT ( 'NONE',  ( 0.05014649552807626948, 215.4116977939061144, 40.25113791807856956 ) ) ;
#31507 = CARTESIAN_POINT ( 'NONE',  ( 64.50000000000000000, -73.00000000000000000, 30.00000000000000000 ) ) ;
#31508 = CARTESIAN_POINT ( 'NONE',  ( 0.05014649552828275708, 196.4853777576173002, 19.74886208192143044 ) ) ;
#31509 = CARTESIAN_POINT ( 'NONE',  ( 64.97499999726881015, 140.1801316387863778, -4.815267126137194431 ) ) ;
#31511 = VERTEX_POINT ( 'NONE', #30805 ) ;
#31510 = CIRCLE ( 'NONE', #24967, 3.047499999999999876 ) ;
#31512 = CARTESIAN_POINT ( 'NONE',  ( -6.500000000000000000, -3.752776749732573247, -0.8000000000000003775 ) ) ;
#31513 = FACE_OUTER_BOUND ( 'NONE', #31763, .T. ) ;
#31514 = CARTESIAN_POINT ( 'NONE',  ( 7.984503880673422316, 209.6470497212048372, 6.848862081921435419 ) ) ;
#31515 = CARTESIAN_POINT ( 'NONE',  ( 3.044812012440130555, 197.4746971517856764, 50.60113791807857808 ) ) ;
#31516 = CARTESIAN_POINT ( 'NONE',  ( -3.135527875058821579, 197.5041725223112223, 23.90113791807856813 ) ) ;
#31517 = CARTESIAN_POINT ( 'NONE',  ( 81.47499999726879594, 160.0630714827496206, -15.58253175000000823 ) ) ;
#31518 = CONTEXT_DEPENDENT_SHAPE_REPRESENTATION ( #724, #13609 ) ;
#31519 = CARTESIAN_POINT ( 'NONE',  ( 0.05014649552828262524, 198.5883022060938572, 88.74886208192143044 ) ) ;
#31520 = CARTESIAN_POINT ( 'NONE',  ( 35.62499999726880873, 171.3844434931184253, -7.942151717890132712E-15 ) ) ;
#31521 = CARTESIAN_POINT ( 'NONE',  ( 52.71132485994279904, 155.0000000000000000, 15.00000000000001243 ) ) ;
#31522 = DIRECTION ( 'NONE',  ( 0.000000000000000000, 0.000000000000000000, -1.000000000000000000 ) ) ;
#31523 = CARTESIAN_POINT ( 'NONE',  ( 12.01549611932652972, 210.8513442034534933, 10.85113791807856565 ) ) ;
#31524 = AXIS2_PLACEMENT_3D ( 'NONE', #3440, #8234, #31405 ) ;
#31525 = CARTESIAN_POINT ( 'NONE',  ( 64.08867513459483689, 142.2402378747194405, 9.270509831248432420 ) ) ;
#31526 = CARTESIAN_POINT ( 'NONE',  ( 57.47499999726879594, 160.0630714827496206, -15.58253175000000823 ) ) ;
#31527 = CARTESIAN_POINT ( 'NONE',  ( 3.044812012440130555, 197.4746971517856764, 53.60113791807857098 ) ) ;
#31528 = CARTESIAN_POINT ( 'NONE',  ( -10.01549611932653860, 203.7984951890123000, 30.35113791807856742 ) ) ;
#31529 = CARTESIAN_POINT ( 'NONE',  ( 0.000000000000000000, -3.518949890710769246, 3.686287386450715076E-15 ) ) ;
#31530 = DIRECTION ( 'NONE',  ( -0.9945218953682777308, 0.000000000000000000, 0.1045284632676128089 ) ) ;
#31531 = CARTESIAN_POINT ( 'NONE',  ( 63.59999999453764019, 141.2096805137202580, -4.480746418436742040 ) ) ;
#31532 = ORIENTED_EDGE ( 'NONE', *, *, #6031, .T. ) ;
#31533 = CARTESIAN_POINT ( 'NONE',  ( -0.05014649552807705357, 194.3824533091408000, 41.75113791807856245 ) ) ;
#31534 = CARTESIAN_POINT ( 'NONE',  ( 5.000000000000000000, -4.685197434473814759, 3.903127820947815962E-15 ) ) ;
#31535 = EDGE_CURVE ( 'NONE', #22189, #17462, #4904, .T. ) ;
#31536 = CARTESIAN_POINT ( 'NONE',  ( 3.044812012439969795, 216.5253028482143520, 24.39886208192143613 ) ) ;
#31537 = CARTESIAN_POINT ( 'NONE',  ( 115.4999999999999858, 102.0000000000001990, 93.94869280115064214 ) ) ;
#31538 = ORIENTED_EDGE ( 'NONE', *, *, #9176, .F. ) ;
#31539 =( BOUNDED_CURVE ( )  B_SPLINE_CURVE ( 2, ( #18326, #15091, #20886, #105, #22767, #5209, #5045, #28388, #15435, #31114, #20546 ),
 .UNSPECIFIED., .F., .T. ) 
 B_SPLINE_CURVE_WITH_KNOTS ( ( 3, 2, 2, 2, 2, 3 ),
 ( 0.2142857142857143293, 0.2178571428571429158, 0.2214285714285714746, 0.2250000000000000611, 0.2285714285714286198, 0.2321428571428572063 ),
 .UNSPECIFIED. ) 
 CURVE ( )  GEOMETRIC_REPRESENTATION_ITEM ( )  RATIONAL_B_SPLINE_CURVE ( ( 0.9999999999999992228, 0.9510565162951541973, 1.000000000000000000, 0.9510565162951534202, 1.000000000000000000, 0.9510565162951534202, 1.000000000000000000, 0.9510565162951534202, 1.000000000000000000, 0.9510565162951526430, 1.000000000000000666 ) ) 
 REPRESENTATION_ITEM ( '' )  );
#31540 = CARTESIAN_POINT ( 'NONE',  ( -8.062137200540920645, 212.9164362838581894, 69.80113791807856671 ) ) ;
#31541 = ORIENTED_EDGE ( 'NONE', *, *, #16321, .T. ) ;
#31542 = CARTESIAN_POINT ( 'NONE',  ( 44.01132485994281751, 167.7597621252805880, -9.270509831248443078 ) ) ;
#31543 = ORIENTED_EDGE ( 'NONE', *, *, #16594, .T. ) ;
#31544 = CARTESIAN_POINT ( 'NONE',  ( -4.984841277089726574, 200.2242689037092305, 18.05113791807856316 ) ) ;
#31545 = VECTOR ( 'NONE', #21792, 1000.000000000000000 ) ;
#31546 = CARTESIAN_POINT ( 'NONE',  ( -3.662846001189865142, 195.5725841191952838, 100.8988620819214361 ) ) ;
#31547 = CARTESIAN_POINT ( 'NONE',  ( 45.87499999726880162, 171.3844434931184253, -7.942151717890134290E-15 ) ) ;
#31548 = VERTEX_POINT ( 'NONE', #25685 ) ;
#31549 = CARTESIAN_POINT ( 'NONE',  ( 48.82499999726880446, 141.7447067706911810, -9.630534252274385310 ) ) ;
#31550 = CARTESIAN_POINT ( 'NONE',  ( -67.50000000000000000, 0.000000000000000000, 17.00000000000001421 ) ) ;
#31551 = CARTESIAN_POINT ( 'NONE',  ( -8.062137200540920645, 212.9164362838581894, 3.801137918078565825 ) ) ;
#31552 = CARTESIAN_POINT ( 'NONE',  ( -3.135527875058982783, 216.4958274776886924, 84.09886208192143897 ) ) ;
#31553 = CARTESIAN_POINT ( 'NONE',  ( 52.07499999726881157, 168.2552932293087906, 9.630534252274372875 ) ) ;
#31554 = LINE ( 'NONE', #29446, #24291 ) ;
#31555 = CARTESIAN_POINT ( 'NONE',  ( -6.220909254589537696, 198.5229672870051161, 24.05113791807855961 ) ) ;
#31556 = CARTESIAN_POINT ( 'NONE',  ( -68.50000000000000000, 215.0000000000000000, 0.000000000000000000 ) ) ;
#31557 = CARTESIAN_POINT ( 'NONE',  ( 76.09999999999999432, 141.2096805137202580, -4.480746418436742040 ) ) ;
#31558 = CARTESIAN_POINT ( 'NONE',  ( -3.135527875058821579, 197.5041725223112223, 98.90113791807857524 ) ) ;
#31559 = DIRECTION ( 'NONE',  ( 0.000000000000000000, 0.000000000000000000, -1.000000000000000000 ) ) ;
#31560 = CARTESIAN_POINT ( 'NONE',  ( -10.01549611932653860, 203.7984951890123284, 84.35113791807856387 ) ) ;
#31561 = CARTESIAN_POINT ( 'NONE',  ( 57.38867513459481984, 169.2658477444273331, 4.635254915624208216 ) ) ;
#31562 = CARTESIAN_POINT ( 'NONE',  ( 40.67499999726880588, 141.7447067706911810, 9.630534252274376428 ) ) ;
#31563 = CARTESIAN_POINT ( 'NONE',  ( -9.680171189290716072, 199.9079932115567146, 98.19886208192144750 ) ) ;
#31564 = CARTESIAN_POINT ( 'NONE',  ( 68.22499999726881015, 149.9369285172503510, 15.58253174999999580 ) ) ;
#31565 = ORIENTED_EDGE ( 'NONE', *, *, #18337, .F. ) ;
#31566 = FACE_OUTER_BOUND ( 'NONE', #25513, .T. ) ;
#31567 = CARTESIAN_POINT ( 'NONE',  ( 42.19999999453762740, 163.5228861582408797, -11.73074641843674470 ) ) ;
#31568 = ADVANCED_BREP_SHAPE_REPRESENTATION ( '', ( #11883, #2404 ), #33408 ) ;
#31569 = PRODUCT_DEFINITION_SHAPE ( 'NONE', 'NONE',  #33694 ) ;
#31570 = DIRECTION ( 'NONE',  ( 0.000000000000000000, 0.000000000000000000, -1.000000000000000000 ) ) ;
#31571 = EDGE_CURVE ( 'NONE', #6338, #29398, #30838, .T. ) ;
#31572 = CARTESIAN_POINT ( 'NONE',  ( 2.499999999999999112, -7.216878364870334295, -7.063244554130005959 ) ) ;
#31573 = ORIENTED_EDGE ( 'NONE', *, *, #13514, .T. ) ;
#31574 = CARTESIAN_POINT ( 'NONE',  ( 8.118202686958138514, 201.1607312380088501, 97.29886208192144181 ) ) ;
#31575 = CARTESIAN_POINT ( 'NONE',  ( 12.01549611932659367, 203.1486557965466773, 34.14886208192143613 ) ) ;
#31576 = DIRECTION ( 'NONE',  ( 1.000000000000000000, 0.000000000000000000, 0.000000000000000000 ) ) ;
#31577 = EDGE_CURVE ( 'NONE', #28898, #28851, #29727, .T. ) ;
#31578 = CARTESIAN_POINT ( 'NONE',  ( -6.139770520408369237, 215.5359834540460042, 42.95113791807856529 ) ) ;
#31579 = ORIENTED_EDGE ( 'NONE', *, *, #27591, .F. ) ;
#31580 = CARTESIAN_POINT ( 'NONE',  ( -2.517493886309087880, 214.5937144450984135, 6.098862081921434530 ) ) ;
#31581 = EDGE_CURVE ( 'NONE', #14343, #10137, #16123, .T. ) ;
#31582 = CARTESIAN_POINT ( 'NONE',  ( 107.5000000000000000, 155.0000000000000000, -6.938893903907228378E-15 ) ) ;
#31583 = VERTEX_POINT ( 'NONE', #31474 ) ;
#31584 = CARTESIAN_POINT ( 'NONE',  ( -7.984503880673422316, 204.3529502787951628, 89.34886208192143897 ) ) ;
#31585 = CARTESIAN_POINT ( 'NONE',  ( 0.05014649552807626948, 215.4116977939061144, 31.25113791807856956 ) ) ;
#31586 = CARTESIAN_POINT ( 'NONE',  ( 56.21132485994281325, 170.7719333635740497, -7.904646289410545231E-15 ) ) ;
#31587 = EDGE_LOOP ( 'NONE', ( #16443, #10603, #28147, #23989, #5922, #12525 ) ) ;
#31588 = DIRECTION ( 'NONE',  ( 0.000000000000000000, 0.000000000000000000, 1.000000000000000000 ) ) ;
#31589 = CARTESIAN_POINT ( 'NONE',  ( 87.22499999726881015, 160.0630714827496206, -15.58253175000000823 ) ) ;
#31590 = DIRECTION ( 'NONE',  ( 0.7071067811865474617, 0.000000000000000000, -0.7071067811865474617 ) ) ;
#31591 = CARTESIAN_POINT ( 'NONE',  ( -8.015496119326531499, 204.4483345814780364, 84.35113791807857808 ) ) ;
#31592 = DIRECTION ( 'NONE',  ( 0.000000000000000000, 0.000000000000000000, 1.000000000000000000 ) ) ;
#31593 = CARTESIAN_POINT ( 'NONE',  ( 51.89999999999999858, 141.2096805137202580, 4.480746418436733158 ) ) ;
#31594 = CARTESIAN_POINT ( 'NONE',  ( -8.000000000000008882, 206.9523078486584780, 71.49886208192144466 ) ) ;
#31595 = CARTESIAN_POINT ( 'NONE',  ( -54.79999999999999716, -6.711064459327494323E-15, 20.00000000000001776 ) ) ;
#31596 = B_SPLINE_CURVE_WITH_KNOTS ( 'NONE', 3,
 ( #26691, #28920, #13742, #27028, #18703, #24139 ),
 .UNSPECIFIED., .F., .F.,
 ( 4, 2, 4 ),
 ( 0.000000000000000000, 0.002307655110370371299, 0.004615310220740742597 ),
 .UNSPECIFIED. ) ;
#31597 = EDGE_CURVE ( 'NONE', #16396, #20223, #11253, .T. ) ;
#31598 = CARTESIAN_POINT ( 'NONE',  ( 51.92499999726880588, 164.1591823560292198, 12.60653300113718167 ) ) ;
#31599 = CARTESIAN_POINT ( 'NONE',  ( 6.139770520408367460, 198.4640165459539389, 8.451137918078565292 ) ) ;
#31600 = CARTESIAN_POINT ( 'NONE',  ( 37.61132485994281183, 150.1262045565063374, -14.99999999999996803 ) ) ;
#31601 = CARTESIAN_POINT ( 'NONE',  ( 66.92499999726881299, 145.8408176439707802, -12.60653300113719588 ) ) ;
#31602 = CARTESIAN_POINT ( 'NONE',  ( 77.27499999726880731, 149.9369285172503510, -15.58253175000000823 ) ) ;
#31603 = CARTESIAN_POINT ( 'NONE',  ( -7.375838497908182134, 217.2372850707499765, 81.95113791807858661 ) ) ;
#31604 = CARTESIAN_POINT ( 'NONE',  ( 49.71132485994280614, 155.0000000000000000, -15.00000000000002487 ) ) ;
#31605 = CARTESIAN_POINT ( 'NONE',  ( -6.139770520408368348, 215.5359834540460042, 93.95113791807855819 ) ) ;
#31606 = EDGE_CURVE ( 'NONE', #9623, #15658, #16660, .T. ) ;
#31607 = DIRECTION ( 'NONE',  ( 1.000000000000000000, -0.000000000000000000, -0.000000000000000000 ) ) ;
#31608 = VERTEX_POINT ( 'NONE', #28415 ) ;
#31609 = CARTESIAN_POINT ( 'NONE',  ( 0.05014649552828288198, 194.3824533091408000, 55.74886208192143755 ) ) ;
#31610 = CARTESIAN_POINT ( 'NONE',  ( -10.01549611932659545, 210.2015048109875011, 68.64886208192143613 ) ) ;
#31611 = AXIS2_PLACEMENT_3D ( 'NONE', #8192, #18899, #21958 ) ;
#31612 = CARTESIAN_POINT ( 'NONE',  ( 0.05014649552828288198, 194.3824533091408000, 7.748862081921433109 ) ) ;
#31613 = CARTESIAN_POINT ( 'NONE',  ( 68.41132485994282320, 167.7597621252805880, 9.270509831248428867 ) ) ;
#31614 = CARTESIAN_POINT ( 'NONE',  ( -3.044812012440131443, 216.5253028482142952, 10.10113791807856565 ) ) ;
#31615 = CARTESIAN_POINT ( 'NONE',  ( 3.044812012439969795, 216.5253028482143520, 75.39886208192143613 ) ) ;
#31616 = APPLICATION_CONTEXT ( 'automotive_design' ) ;
#31617 = ORIENTED_EDGE ( 'NONE', *, *, #32432, .F. ) ;
#31618 = EDGE_CURVE ( 'NONE', #22909, #948, #16922, .T. ) ;
#31619 = VERTEX_POINT ( 'NONE', #5567 ) ;
#31620 = LINE ( 'NONE', #16105, #2599 ) ;
#31621 = CARTESIAN_POINT ( 'NONE',  ( 2.426778023690075337, 214.6231898156240447, 63.39886208192144323 ) ) ;
#31622 = ORIENTED_EDGE ( 'NONE', *, *, #13726, .T. ) ;
#31623 = CARTESIAN_POINT ( 'NONE',  ( 75.02499999726879309, 149.9369285172503510, -15.58253175000000823 ) ) ;
#31624 = FACE_OUTER_BOUND ( 'NONE', #25668, .T. ) ;
#31625 = DIRECTION ( 'NONE',  ( 0.000000000000000000, 1.000000000000000000, -9.682177540335733218E-15 ) ) ;
#31626 = AXIS2_PLACEMENT_3D ( 'NONE', #2186, #2357, #28253 ) ;
#31627 = CARTESIAN_POINT ( 'NONE',  ( 71.42499999726879878, 168.2552932293087906, -9.630534252274385310 ) ) ;
#31628 = EDGE_CURVE ( 'NONE', #6222, #21367, #31310, .T. ) ;
#31629 = CARTESIAN_POINT ( 'NONE',  ( 0.05014649552807626948, 215.4116977939061144, 61.25113791807857666 ) ) ;
#31630 = FACE_OUTER_BOUND ( 'NONE', #22900, .T. ) ;
#31631 = DIRECTION ( 'NONE',  ( 0.000000000000000000, 0.000000000000000000, -1.000000000000000000 ) ) ;
#31632 = CARTESIAN_POINT ( 'NONE',  ( 3.339999999999998970, 0.000000000000000000, -0.4621369752184044666 ) ) ;
#31633 = CARTESIAN_POINT ( 'NONE',  ( -7.984503880673422316, 204.3529502787951628, 35.34886208192144608 ) ) ;
#31634 = CARTESIAN_POINT ( 'NONE',  ( 0.05014649552810505201, 217.5146222423826714, 79.25113791807856956 ) ) ;
#31635 = CARTESIAN_POINT ( 'NONE',  ( 3.250000000000000444, 5.629165124598851655, -5.592027715088707218 ) ) ;
#31636 = CARTESIAN_POINT ( 'NONE',  ( -8.062137200540920645, 212.9164362838581894, 63.80113791807858092 ) ) ;
#31637 = DIRECTION ( 'NONE',  ( -1.000000000000000000, 0.000000000000000000, 0.000000000000000000 ) ) ;
#31638 = CARTESIAN_POINT ( 'NONE',  ( 8.015496119326531499, 209.5516654185219636, 10.85113791807856565 ) ) ;
#31639 = DIRECTION ( 'NONE',  ( 0.000000000000000000, 0.000000000000000000, -1.000000000000000000 ) ) ;
#31640 = CARTESIAN_POINT ( 'NONE',  ( -2.075968632161309557, 6.306992450857741517, -6.056431503346038525 ) ) ;
#31641 = CARTESIAN_POINT ( 'NONE',  ( 43.42499999726881299, 168.2552932293087906, -9.630534252274387086 ) ) ;
#31642 =( BOUNDED_CURVE ( )  B_SPLINE_CURVE ( 2, ( #22682, #12462, #31, #4792, #4966, #9739, #10427, #20125, #20799, #4630, #31201 ),
 .UNSPECIFIED., .F., .T. ) 
 B_SPLINE_CURVE_WITH_KNOTS ( ( 3, 2, 2, 2, 2, 3 ),
 ( 0.1428571428571428492, 0.1464285714285714357, 0.1499999999999999944, 0.1535714285714285532, 0.1571428571428571119, 0.1607142857142856984 ),
 .UNSPECIFIED. ) 
 CURVE ( )  GEOMETRIC_REPRESENTATION_ITEM ( )  RATIONAL_B_SPLINE_CURVE ( ( 1.000000000000000000, 0.9510565162951534202, 1.000000000000000000, 0.9510565162951534202, 1.000000000000000000, 0.9510565162951534202, 1.000000000000000000, 0.9510565162951534202, 1.000000000000000000, 0.9510565162951537532, 0.9999999999999996669 ) ) 
 REPRESENTATION_ITEM ( '' )  );
#31643 = CARTESIAN_POINT ( 'NONE',  ( 11.98450388067348271, 203.0532714938637753, 50.15113791807857524 ) ) ;
#31644 = DIRECTION ( 'NONE',  ( 0.000000000000000000, 0.9988620819214357738, 0.04769215134144196705 ) ) ;
#31645 = CARTESIAN_POINT ( 'NONE',  ( -3.135527875058821579, 197.5041725223112223, 98.90113791807857524 ) ) ;
#31646 = CARTESIAN_POINT ( 'NONE',  ( 6.220909254589536808, 215.4770327129947987, 55.55113791807856671 ) ) ;
#31647 = CARTESIAN_POINT ( 'NONE',  ( 9.680171189290716072, 214.0920067884432854, 24.69886208192143684 ) ) ;
#31648 = CARTESIAN_POINT ( 'NONE',  ( -0.05014649552828402690, 217.5146222423826714, 36.24886208192143755 ) ) ;
#31649 = AXIS2_PLACEMENT_3D ( 'NONE', #556, #29671, #5819 ) ;
#31650 = CARTESIAN_POINT ( 'NONE',  ( 78.09999999453762598, 159.7113355953771077, -14.50000000000000888 ) ) ;
#31651 = CARTESIAN_POINT ( 'NONE',  ( -3.753561863808691168, 195.6020594897209435, 68.90113791807856103 ) ) ;
#31652 = CARTESIAN_POINT ( 'NONE',  ( -6.500168698208129925, 202.3363017425936050, 87.20113791807858661 ) ) ;
#31653 = CARTESIAN_POINT ( 'NONE',  ( 9.984503880673420539, 210.2968891136705167, 51.84886208192143897 ) ) ;
#31654 = CARTESIAN_POINT ( 'NONE',  ( -67.50000000000000000, 155.0000000000000000, 6.938893903907228378E-15 ) ) ;
#31655 = VERTEX_POINT ( 'NONE', #10369 ) ;
#31656 = CARTESIAN_POINT ( 'NONE',  ( -7.375838497908014268, 196.7627149292498530, 53.04886208192142760 ) ) ;
#31657 = CIRCLE ( 'NONE', #23494, 12.10452846326765020 ) ;
#31658 = ORIENTED_EDGE ( 'NONE', *, *, #19742, .T. ) ;
#31659 = VERTEX_POINT ( 'NONE', #20742 ) ;
#31660 = EDGE_CURVE ( 'NONE', #24999, #19012, #31138, .T. ) ;
#31661 = EDGE_CURVE ( 'NONE', #20912, #14808, #21026, .T. ) ;
#31662 = CARTESIAN_POINT ( 'NONE',  ( 74.07499999726881867, 168.2552932293087906, 9.630534252274372875 ) ) ;
#31663 = DIRECTION ( 'NONE',  ( 0.000000000000000000, 0.000000000000000000, -1.000000000000000000 ) ) ;
#31664 = DIRECTION ( 'NONE',  ( 0.000000000000000000, 0.000000000000000000, 1.000000000000000000 ) ) ;
#31665 = CARTESIAN_POINT ( 'NONE',  ( -6.500168698208129925, 202.3363017425936050, 42.20113791807857240 ) ) ;
#31666 = EDGE_CURVE ( 'NONE', #31659, #19344, #5728, .T. ) ;
#31667 = EDGE_CURVE ( 'NONE', #27919, #22576, #27553, .T. ) ;
#31668 = CARTESIAN_POINT ( 'NONE',  ( 9.984503880673420539, 210.2968891136705167, 33.84886208192143187 ) ) ;
#31669 = CARTESIAN_POINT ( 'NONE',  ( 63.97499999726881725, 169.8198683612136222, 4.815267126137181997 ) ) ;
#31670 = ORIENTED_EDGE ( 'NONE', *, *, #8935, .T. ) ;
#31671 = CARTESIAN_POINT ( 'NONE',  ( 36.41132485994280898, 167.7597621252805880, 9.270509831248428867 ) ) ;
#31672 = CARTESIAN_POINT ( 'NONE',  ( -4.232971792145048787E-15, -9.016621985895911351, -7.999704684617487516 ) ) ;
#31673 = CARTESIAN_POINT ( 'NONE',  ( 6.500168698208244500, 202.3363017425938324, 7.298862081921435596 ) ) ;
#31674 = CARTESIAN_POINT ( 'NONE',  ( 8.062137200540920645, 201.0835637161417822, 47.30113791807857382 ) ) ;
#31675 = CARTESIAN_POINT ( 'NONE',  ( 4.000000000000000000, 0.000000000000000000, 0.000000000000000000 ) ) ;
#31676 = CARTESIAN_POINT ( 'NONE',  ( 3.135527875058820690, 216.4958274776887492, 37.40113791807857524 ) ) ;
#31677 = CARTESIAN_POINT ( 'NONE',  ( 87.37499999726880162, 155.0000000000000000, -15.58253175000000823 ) ) ;
#31678 = ITEM_DEFINED_TRANSFORMATION ( 'NONE', 'NONE', #9367,  #2404 ) ;
#31679 = CARTESIAN_POINT ( 'NONE',  ( 6.500168698208244500, 202.3363017425938324, 94.29886208192142760 ) ) ;
#31680 = CARTESIAN_POINT ( 'NONE',  ( 41.72499999726881015, 169.8198683612136222, 4.815267126137181997 ) ) ;
#31681 = DIRECTION ( 'NONE',  ( -1.000000000000000000, -0.000000000000000000, 0.000000000000000000 ) ) ;
#31682 = FACE_OUTER_BOUND ( 'NONE', #11881, .T. ) ;
#31683 = CARTESIAN_POINT ( 'NONE',  ( -3.753561863808691168, 195.6020594897209435, 11.90113791807856813 ) ) ;
#31684 = CARTESIAN_POINT ( 'NONE',  ( 58.27499999726880731, 160.0630714827496206, 15.58253174999999402 ) ) ;
#31685 = VECTOR ( 'NONE', #2801, 1000.000000000000227 ) ;
#31686 = CARTESIAN_POINT ( 'NONE',  ( -3.044812012440131443, 216.5253028482142952, 67.10113791807857808 ) ) ;
#31687 = CARTESIAN_POINT ( 'NONE',  ( -0.05014649552810635652, 196.4853777576173002, 29.75113791807856956 ) ) ;
#31688 = DIRECTION ( 'NONE',  ( 0.000000000000000000, -0.7071067811865506814, -0.7071067811865442421 ) ) ;
#31689 = CARTESIAN_POINT ( 'NONE',  ( -11.41286821541921448, 25.16504226903141017, -17.92845254598170257 ) ) ;
#31690 = CARTESIAN_POINT ( 'NONE',  ( 0.05014649552828275014, 196.4853777576173002, 13.74886208192143400 ) ) ;
#31691 = CARTESIAN_POINT ( 'NONE',  ( 60.99999999453763166, 155.0000000000000000, 14.49999999999999467 ) ) ;
#31692 = ORIENTED_EDGE ( 'NONE', *, *, #25545, .T. ) ;
#31693 = CARTESIAN_POINT ( 'NONE',  ( 3.753561863808689836, 218.3979405102790565, 37.40113791807856813 ) ) ;
#31694 = PLANE ( 'NONE',  #17072 ) ;
#31695 = CARTESIAN_POINT ( 'NONE',  ( -8.062137200540822946, 201.0835637161416400, 26.19886208192143684 ) ) ;
#31696 = CARTESIAN_POINT ( 'NONE',  ( 70.78867513459482552, 155.0000000000000000, -15.00000000000002487 ) ) ;
#31697 = ORIENTED_EDGE ( 'NONE', *, *, #13967, .F. ) ;
#31698 = AXIS2_PLACEMENT_3D ( 'NONE', #22844, #10415, #2748 ) ;
#31699 = CARTESIAN_POINT ( 'NONE',  ( 10.00000000000000711, 206.9523078486586201, 83.00113791807856956 ) ) ;
#31700 = EDGE_LOOP ( 'NONE', ( #9494, #8913, #28684, #32038 ) ) ;
#31701 = DIRECTION ( 'NONE',  ( 1.000000000000000000, 0.000000000000000000, 0.000000000000000000 ) ) ;
#31702 = CARTESIAN_POINT ( 'NONE',  ( 58.50000000000001421, -88.00000000000000000, -30.00000000000000000 ) ) ;
#31703 = ORIENTED_EDGE ( 'NONE', *, *, #8088, .T. ) ;
#31704 = CIRCLE ( 'NONE', #17007, 12.10452846326767684 ) ;
#31705 = CARTESIAN_POINT ( 'NONE',  ( -2.517493886308901807, 199.4062855549015012, 11.90113791807856813 ) ) ;
#31706 = AXIS2_PLACEMENT_3D ( 'NONE', #11297, #19294, #29686 ) ;
#31707 = DIRECTION ( 'NONE',  ( 0.000000000000000000, 0.000000000000000000, -1.000000000000000000 ) ) ;
#31708 = CARTESIAN_POINT ( 'NONE',  ( -3.753561863808878130, 218.3979405102790281, 102.0988620819214532 ) ) ;
#31709 = CARTESIAN_POINT ( 'NONE',  ( 42.57499999726881157, 145.8408176439707802, 12.60653300113718345 ) ) ;
#31710 = ORIENTED_EDGE ( 'NONE', *, *, #28045, .F. ) ;
#31711 = CARTESIAN_POINT ( 'NONE',  ( 47.62499999726880162, 171.3844434931184253, -7.942151717890132712E-15 ) ) ;
#31712 = CARTESIAN_POINT ( 'NONE',  ( 32.50000000000000000, 155.0000000000000000, -15.00000000000002487 ) ) ;
#31713 = DIRECTION ( 'NONE',  ( -0.000000000000000000, -0.000000000000000000, 1.000000000000000000 ) ) ;
#31714 = CARTESIAN_POINT ( 'NONE',  ( -6.139770520408224463, 198.4640165459539389, 80.04886208192139918 ) ) ;
#31715 = CARTESIAN_POINT ( 'NONE',  ( 56.67499999726881299, 141.7447067706911810, 9.630534252274376428 ) ) ;
#31716 = CARTESIAN_POINT ( 'NONE',  ( 0.05014649552810505201, 217.5146222423826714, 22.25113791807856956 ) ) ;
#31717 = CARTESIAN_POINT ( 'NONE',  ( 47.68867513459483831, 159.8737954434934920, 15.00000000000010836 ) ) ;
#31718 = CONICAL_SURFACE ( 'NONE', #17029, 15.79999999999999538, 0.9599310885968802554 ) ;
#31719 = CARTESIAN_POINT ( 'NONE',  ( 75.19999999999998863, 167.3344367211045096, 8.961492836873468093 ) ) ;
#31720 = DIRECTION ( 'NONE',  ( 0.9945218953682777308, 0.000000000000000000, -0.1045284632676113518 ) ) ;
#31721 = DIRECTION ( 'NONE',  ( 1.000000000000000000, -0.000000000000000000, -0.000000000000000000 ) ) ;
#31722 = CARTESIAN_POINT ( 'NONE',  ( 9.984503880673470277, 203.7031108863295401, 89.15113791807857524 ) ) ;
#31723 = LINE ( 'NONE', #11450, #24916 ) ;
#31724 = CARTESIAN_POINT ( 'NONE',  ( 39.97499999726881015, 169.8198683612136222, 4.815267126137181997 ) ) ;
#31725 = CARTESIAN_POINT ( 'NONE',  ( -0.05014649552828442242, 219.6175466908591716, 99.24886208192143044 ) ) ;
#31726 = CARTESIAN_POINT ( 'NONE',  ( 78.52499999726880731, 140.1801316387863778, 4.815267126137185549 ) ) ;
#31727 = VERTEX_POINT ( 'NONE', #2701 ) ;
#31728 = DIRECTION ( 'NONE',  ( -0.08583835255247916629, -0.09953364313786493278, -0.9913247858874408847 ) ) ;
#31729 = VECTOR ( 'NONE', #2615, 1000.000000000000000 ) ;
#31730 = CARTESIAN_POINT ( 'NONE',  ( 44.29999999453762882, 167.3344367211045096, -8.961492836873482304 ) ) ;
#31731 = CIRCLE ( 'NONE', #11068, 8.000000000000000000 ) ;
#31732 = CARTESIAN_POINT ( 'NONE',  ( -63.50000000000001421, 210.0000000000000000, 0.000000000000000000 ) ) ;
#31733 = CARTESIAN_POINT ( 'NONE',  ( -3.093533885184598375, -6.874201416485457017, -7.446478553994068328 ) ) ;
#31734 = EDGE_LOOP ( 'NONE', ( #28356, #9369, #3075, #18919 ) ) ;
#31735 = CARTESIAN_POINT ( 'NONE',  ( 8.118202686958138514, 201.1607312380088501, 94.29886208192144181 ) ) ;
#31736 = CARTESIAN_POINT ( 'NONE',  ( -0.05014649552828442242, 219.6175466908591716, 30.24886208192143755 ) ) ;
#31737 = CARTESIAN_POINT ( 'NONE',  ( 93.60208470531338776, 155.0000000000000000, 0.000000000000000000 ) ) ;
#31738 = CARTESIAN_POINT ( 'NONE',  ( -3.044812012440131443, 216.5253028482142952, 49.10113791807857808 ) ) ;
#31739 = VERTEX_POINT ( 'NONE', #21238 ) ;
#31740 = CARTESIAN_POINT ( 'NONE',  ( -8.015496119326597224, 209.5516654185217362, 5.648862081921434353 ) ) ;
#31741 = TOROIDAL_SURFACE ( 'NONE', #18138, 9.624472924841564136, 1.000000000000000444 ) ;
#31742 = DIRECTION ( 'NONE',  ( 0.8660254037844384856, 0.5000000000000003331, 0.000000000000000000 ) ) ;
#31743 = EDGE_LOOP ( 'NONE', ( #31770, #7199 ) ) ;
#31745 = CARTESIAN_POINT ( 'NONE',  ( -0.05014649552828365914, 215.4116977939061144, 87.24886208192144466 ) ) ;
#31744 = COLOUR_RGB ( '', 0.40784314, 0.44705882, 0.49803922) ;
#31746 = CARTESIAN_POINT ( 'NONE',  ( -2.517493886308901807, 199.4062855549015012, 26.90113791807856813 ) ) ;
#31747 = DIRECTION ( 'NONE',  ( 1.000000000000000000, 0.000000000000000000, 0.000000000000000000 ) ) ;
#31748 = VERTEX_POINT ( 'NONE', #23636 ) ;
#31749 = CARTESIAN_POINT ( 'NONE',  ( -0.04725809328185606034, 9.175759667312519241, -8.057670357645360326 ) ) ;
#31750 = VECTOR ( 'NONE', #27809, 1000.000000000000227 ) ;
#31751 = AXIS2_PLACEMENT_3D ( 'NONE', #904, #29524, #3799 ) ;
#31752 = CARTESIAN_POINT ( 'NONE',  ( 36.67499999726879878, 141.7447067706911810, 9.630534252274376428 ) ) ;
#31753 = CARTESIAN_POINT ( 'NONE',  ( -6.500168698208129925, 202.3363017425936050, 96.20113791807858661 ) ) ;
#31754 = ADVANCED_FACE ( 'NONE', ( #3015 ), #12881, .T. ) ;
#31755 = CIRCLE ( 'NONE', #15977, 1.649999999999999911 ) ;
#31756 = DIRECTION ( 'NONE',  ( 1.000000000000000000, 0.000000000000000000, 0.000000000000000000 ) ) ;
#31757 = CARTESIAN_POINT ( 'NONE',  ( 53.29999999999999716, 163.5228861582408797, 11.73074641843673049 ) ) ;
#31758 = CARTESIAN_POINT ( 'NONE',  ( -2.517493886309087880, 214.5937144450984135, 75.09886208192142476 ) ) ;
#31759 = CARTESIAN_POINT ( 'NONE',  ( 0.000000000000000000, 0.000000000000000000, -2.899999999999999911 ) ) ;
#31760 = CARTESIAN_POINT ( 'NONE',  ( 60.62499999726879452, 138.6155565068815463, -3.929120461958505118E-15 ) ) ;
#31761 = AXIS2_PLACEMENT_3D ( 'NONE', #18807, #19311, #32251 ) ;
#31763 = EDGE_LOOP ( 'NONE', ( #10355, #22098, #23069, #14435, #30231 ) ) ;
#31762 = CARTESIAN_POINT ( 'NONE',  ( 0.05014649552810506589, 217.5146222423826714, 7.251137918078566003 ) ) ;
#31764 = CARTESIAN_POINT ( 'NONE',  ( 36.81132485994281467, 150.1262045565063943, 14.99999999999997691 ) ) ;
#31765 = CARTESIAN_POINT ( 'NONE',  ( 64.92499999726881299, 145.8408176439707802, -12.60653300113719588 ) ) ;
#31766 = CARTESIAN_POINT ( 'NONE',  ( 74.47499999726881015, 149.9369285172503510, 15.58253174999999580 ) ) ;
#31767 = CARTESIAN_POINT ( 'NONE',  ( 7.456977232089302632, 217.1783343296989131, 79.55113791807858092 ) ) ;
#31768 = CARTESIAN_POINT ( 'NONE',  ( -10.01549611932653860, 203.7984951890123000, 99.35113791807857808 ) ) ;
#31769 = LINE ( 'NONE', #29216, #21063 ) ;
#31770 = ORIENTED_EDGE ( 'NONE', *, *, #7424, .F. ) ;
#31771 = CARTESIAN_POINT ( 'NONE',  ( 9.680171189290716072, 214.0920067884432854, 60.69886208192144039 ) ) ;
#31772 = CARTESIAN_POINT ( 'NONE',  ( 3.135527875058981895, 197.5041725223112792, 67.59886208192143897 ) ) ;
#31773 = VECTOR ( 'NONE', #6107, 1000.000000000000000 ) ;
#31774 = CARTESIAN_POINT ( 'NONE',  ( 12.00000000000000711, 207.0476921513415220, 3.998862081921433997 ) ) ;
#31775 = DIRECTION ( 'NONE',  ( -0.8660254037844382635, -0.5000000000000004441, 0.000000000000000000 ) ) ;
#31776 = CARTESIAN_POINT ( 'NONE',  ( 8.062137200540920645, 201.0835637161417822, 14.30113791807856671 ) ) ;
#31777 = AXIS2_PLACEMENT_3D ( 'NONE', #32875, #9368, #27428 ) ;
#31778 = CARTESIAN_POINT ( 'NONE',  ( -9.984503880673420539, 203.7031108863293980, 83.34886208192139634 ) ) ;
#31779 = VERTEX_POINT ( 'NONE', #13078 ) ;
#31780 = CARTESIAN_POINT ( 'NONE',  ( 10.00000000000000711, 206.9523078486586201, 101.0011379180785696 ) ) ;
#31781 = VERTEX_POINT ( 'NONE', #10863 ) ;
#31782 = CARTESIAN_POINT ( 'NONE',  ( 107.0104235265664556, 155.0000000000000000, 0.000000000000000000 ) ) ;
#31783 = CARTESIAN_POINT ( 'NONE',  ( 0.05014649552828262524, 198.5883022060938572, 64.74886208192143044 ) ) ;
#31784 = VERTEX_POINT ( 'NONE', #23135 ) ;
#31785 = CARTESIAN_POINT ( 'NONE',  ( 80.82499999726880446, 141.7447067706911810, -9.630534252274387086 ) ) ;
#31786 = VERTEX_POINT ( 'NONE', #18359 ) ;
#31787 = CARTESIAN_POINT ( 'NONE',  ( -2.690931834596280936, 5.951943280390038282, 1.006275141338108408E-15 ) ) ;
#31788 = CARTESIAN_POINT ( 'NONE',  ( 69.12499999726881583, 155.0000000000000000, -15.58253175000000823 ) ) ;
#31789 = CARTESIAN_POINT ( 'NONE',  ( 2.426778023690261410, 199.3768101843759837, 68.60113791807857808 ) ) ;
#31790 = EDGE_CURVE ( 'NONE', #18140, #895, #10536, .T. ) ;
#31791 = DIRECTION ( 'NONE',  ( 1.000000000000000000, 0.000000000000000000, -0.000000000000000000 ) ) ;
#31792 = AXIS2_PLACEMENT_3D ( 'NONE', #20242, #28595, #20421 ) ;
#31793 = CARTESIAN_POINT ( 'NONE',  ( 32.60000000000000853, 159.7113355953771077, -14.50000000000000888 ) ) ;
#31794 = CARTESIAN_POINT ( 'NONE',  ( 6.444103211790928043, 211.7408657792734061, 48.69886208192144750 ) ) ;
#31795 = CARTESIAN_POINT ( 'NONE',  ( 6.220909254589536808, 215.4770327129947702, 76.55113791807855250 ) ) ;
#31796 = CARTESIAN_POINT ( 'NONE',  ( -10.00000000000000711, 207.0476921513413515, 66.50113791807856956 ) ) ;
#31797 = EDGE_CURVE ( 'NONE', #19546, #16312, #21568, .T. ) ;
#31798 = PLANE ( 'NONE',  #15897 ) ;
#31799 = CARTESIAN_POINT ( 'NONE',  ( 8.000000000000008882, 206.9523078486586485, 20.00113791807856956 ) ) ;
#31800 = CARTESIAN_POINT ( 'NONE',  ( 7.500000000000000000, 4.330127018922190096, -7.422398894150032511 ) ) ;
#31801 = FACE_OUTER_BOUND ( 'NONE', #25627, .T. ) ;
#31802 = CARTESIAN_POINT ( 'NONE',  ( 46.12499999726880873, 155.0000000000000000, 15.58253174999999402 ) ) ;
#31803 = CARTESIAN_POINT ( 'NONE',  ( -9.680171189290831535, 214.0920067884431148, 45.80113791807856671 ) ) ;
#31804 = FACE_OUTER_BOUND ( 'NONE', #1913, .T. ) ;
#31805 = CARTESIAN_POINT ( 'NONE',  ( 6.139770520408368348, 198.4640165459539674, 98.45113791807854398 ) ) ;
#31806 = CARTESIAN_POINT ( 'NONE',  ( -0.05014649552810635652, 196.4853777576173002, 65.75113791807856956 ) ) ;
#31807 = CARTESIAN_POINT ( 'NONE',  ( -11.98450388067341876, 203.0532714938636047, 29.34886208192143897 ) ) ;
#31808 = CARTESIAN_POINT ( 'NONE',  ( -10.00000000000000711, 206.9523078486584495, 38.49886208192143755 ) ) ;
#31809 = CARTESIAN_POINT ( 'NONE',  ( 81.19999999453763451, 146.4771138417591203, 11.73074641843673227 ) ) ;
#31810 = CARTESIAN_POINT ( 'NONE',  ( -7.456977232089304408, 196.8216656703010301, 81.05113791807856671 ) ) ;
#31811 = CARTESIAN_POINT ( 'NONE',  ( -6.444103211791042618, 211.7408657792732356, 84.80113791807858092 ) ) ;
#31812 = EDGE_CURVE ( 'NONE', #28067, #26664, #715, .T. ) ;
#31813 = CARTESIAN_POINT ( 'NONE',  ( -8.118202686958138514, 212.8392687619910930, 47.79886208192143471 ) ) ;
#31814 = FACE_OUTER_BOUND ( 'NONE', #22783, .T. ) ;
#31815 = ORIENTED_EDGE ( 'NONE', *, *, #26437, .T. ) ;
#31816 = CARTESIAN_POINT ( 'NONE',  ( 0.05014649552828288198, 194.3824533091408000, 58.74886208192142334 ) ) ;
#31817 = ORIENTED_EDGE ( 'NONE', *, *, #22085, .F. ) ;
#31818 = CARTESIAN_POINT ( 'NONE',  ( 8.000000000000008882, 207.0476921513415220, 30.99886208192143400 ) ) ;
#31819 = EDGE_CURVE ( 'NONE', #22749, #15528, #20579, .T. ) ;
#31820 = ORIENTED_EDGE ( 'NONE', *, *, #29497, .F. ) ;
#31821 = CARTESIAN_POINT ( 'NONE',  ( 77.37499999726881583, 155.0000000000000000, -15.58253175000000823 ) ) ;
#31822 = CARTESIAN_POINT ( 'NONE',  ( 105.0134430565187387, 155.0000000000000000, 0.000000000000000000 ) ) ;
#31823 = FACE_OUTER_BOUND ( 'NONE', #26253, .T. ) ;
#31824 = CARTESIAN_POINT ( 'NONE',  ( 2.426778023690261410, 199.3768101843759837, 53.60113791807856387 ) ) ;
#31825 = FACE_OUTER_BOUND ( 'NONE', #8283, .T. ) ;
#31826 = CARTESIAN_POINT ( 'NONE',  ( 8.118202686958138514, 201.1607312380088501, 31.29886208192143826 ) ) ;
#31827 = CARTESIAN_POINT ( 'NONE',  ( 72.37499999726881583, 155.0000000000000000, 15.58253174999999402 ) ) ;
#31828 = EDGE_LOOP ( 'NONE', ( #9095, #7380, #11745, #3968 ) ) ;
#31829 = CARTESIAN_POINT ( 'NONE',  ( 41.18867513459483121, 169.2658477444273331, -4.635254915624224203 ) ) ;
#31830 =( BOUNDED_CURVE ( )  B_SPLINE_CURVE ( 3, ( #33489, #31110, #12874, #13046 ),
 .UNSPECIFIED., .F., .F. ) 
 B_SPLINE_CURVE_WITH_KNOTS ( ( 4, 4 ),
 ( 3.141592653589793116, 3.666471587091465700 ),
 .UNSPECIFIED. ) 
 CURVE ( )  GEOMETRIC_REPRESENTATION_ITEM ( )  RATIONAL_B_SPLINE_CURVE ( ( 1.000000000000000000, 0.9771733092046011038, 0.9771733092046011038, 1.000000000000000000 ) ) 
 REPRESENTATION_ITEM ( '' )  );
#31831 = DIRECTION ( 'NONE',  ( -0.000000000000000000, -0.000000000000000000, 1.000000000000000000 ) ) ;
#31832 = CARTESIAN_POINT ( 'NONE',  ( 2.426778023690075337, 214.6231898156240447, 18.39886208192143613 ) ) ;
#31833 = CARTESIAN_POINT ( 'NONE',  ( 6.220909254589536808, 215.4770327129947702, 49.55113791807855250 ) ) ;
#31834 = CARTESIAN_POINT ( 'NONE',  ( 7.264118654998712898, -4.945491722146229563, -7.907633014911220393 ) ) ;
#31835 = PRODUCT_DEFINITION_SHAPE ( 'NONE', 'NONE',  #33715 ) ;
#31836 = CARTESIAN_POINT ( 'NONE',  ( 3.044812012440130555, 197.4746971517856764, 32.60113791807857098 ) ) ;
#31837 = CARTESIAN_POINT ( 'NONE',  ( 84.57499999726880446, 145.8408176439707802, 12.60653300113718345 ) ) ;
#31838 = CARTESIAN_POINT ( 'NONE',  ( -8.015496119326597224, 209.5516654185217362, 89.64886208192142192 ) ) ;
#31839 = CARTESIAN_POINT ( 'NONE',  ( 36.32499999726881157, 145.8408176439707802, 12.60653300113718345 ) ) ;
#31840 =( NAMED_UNIT ( * ) SI_UNIT ( $, .STERADIAN. ) SOLID_ANGLE_UNIT ( ) );
#31841 = CARTESIAN_POINT ( 'NONE',  ( -3.500000000000001332, 2.020725942163676070, -2.899999999999999911 ) ) ;
#31842 = CARTESIAN_POINT ( 'NONE',  ( 7.456977232089302632, 217.1783343296989131, 19.55113791807856671 ) ) ;
#31843 = CARTESIAN_POINT ( 'NONE',  ( 7.848314987057850800, -4.129027267381569999, -7.493854785173811095 ) ) ;
#31844 = CARTESIAN_POINT ( 'NONE',  ( 59.47499999726879594, 160.0630714827496206, -15.58253175000000823 ) ) ;
#31845 = EDGE_CURVE ( 'NONE', #25373, #20010, #15933, .T. ) ;
#31846 = CARTESIAN_POINT ( 'NONE',  ( -6.220909254589537696, 198.5229672870051161, 66.05113791807858092 ) ) ;
#31847 = EDGE_CURVE ( 'NONE', #8400, #9623, #23302, .T. ) ;
#31848 = CARTESIAN_POINT ( 'NONE',  ( -3.044812012440131443, 216.5253028482142952, 37.10113791807857098 ) ) ;
#31849 = DIRECTION ( 'NONE',  ( -1.000000000000000000, 0.000000000000000000, 0.000000000000000000 ) ) ;
#31850 = CARTESIAN_POINT ( 'NONE',  ( 105.0134430565187387, 155.0000000000000000, 0.000000000000000000 ) ) ;
#31851 = CARTESIAN_POINT ( 'NONE',  ( -6.139770520408224463, 198.4640165459539105, 14.04886208192143471 ) ) ;
#31852 = CARTESIAN_POINT ( 'NONE',  ( 62.49999999453763166, 170.2462022514548323, -7.872454543227099337E-15 ) ) ;
#31853 = EDGE_LOOP ( 'NONE', ( #3499, #7718, #15195, #17798, #8947 ) ) ;
#31854 = CARTESIAN_POINT ( 'NONE',  ( -3.662846001190052991, 218.4274158808045740, 52.10113791807857808 ) ) ;
#31855 = EDGE_CURVE ( 'NONE', #5501, #29612, #5409, .T. ) ;
#31856 = DIRECTION ( 'NONE',  ( 0.000000000000000000, 0.000000000000000000, -1.000000000000000000 ) ) ;
#31857 = CARTESIAN_POINT ( 'NONE',  ( 6.220909254589681581, 198.5229672870052582, 19.44886208192142618 ) ) ;
#31858 = FACE_OUTER_BOUND ( 'NONE', #24023, .T. ) ;
#31859 = EDGE_LOOP ( 'NONE', ( #30708, #10608, #7080, #21146, #10447 ) ) ;
#31860 = CARTESIAN_POINT ( 'NONE',  ( -6.139770520408369237, 215.5359834540460042, 78.95113791807858661 ) ) ;
#31861 = ADVANCED_FACE ( 'NONE', ( #1127 ), #23279, .F. ) ;
#31862 = ORIENTED_EDGE ( 'NONE', *, *, #20533, .T. ) ;
#31863 = DIRECTION ( 'NONE',  ( 1.000000000000000000, 0.000000000000000000, 0.000000000000000000 ) ) ;
#31864 = DIRECTION ( 'NONE',  ( 0.3362851123284906207, 0.04491457122451913281, 0.9406885799869860731 ) ) ;
#31865 = ORIENTED_EDGE ( 'NONE', *, *, #31044, .F. ) ;
#31866 = CARTESIAN_POINT ( 'NONE',  ( 2.517493886308900919, 214.5937144450984420, 19.40113791807856813 ) ) ;
#31867 = DIRECTION ( 'NONE',  ( -0.000000000000000000, -0.000000000000000000, 1.000000000000000000 ) ) ;
#31868 = CARTESIAN_POINT ( 'NONE',  ( -12.00000000000000711, 206.9523078486584780, 104.4988620819214304 ) ) ;
#31869 = CARTESIAN_POINT ( 'NONE',  ( 49.17499999726881299, 145.8408176439707802, -12.60653300113719588 ) ) ;
#31870 = ORIENTED_EDGE ( 'NONE', *, *, #25823, .T. ) ;
#31871 = CARTESIAN_POINT ( 'NONE',  ( 58.02499999726880731, 160.0630714827496206, 15.58253174999999402 ) ) ;
#31872 = LINE ( 'NONE', #8709, #26231 ) ;
#31873 = DIRECTION ( 'NONE',  ( 1.000000000000000000, 0.000000000000000000, 0.000000000000000000 ) ) ;
#31874 = LINE ( 'NONE', #11112, #18448 ) ;
#31875 = CARTESIAN_POINT ( 'NONE',  ( -0.05014649552828403384, 217.5146222423826714, 84.24886208192143044 ) ) ;
#31876 = CARTESIAN_POINT ( 'NONE',  ( 52.87499999726880162, 138.6155565068815463, -3.929120461958505118E-15 ) ) ;
#31877 = CARTESIAN_POINT ( 'NONE',  ( 8.062137200540920645, 201.0835637161417822, 26.30113791807856671 ) ) ;
#31878 = CARTESIAN_POINT ( 'NONE',  ( 47.38867513459482694, 169.2658477444273331, 4.635254915624208216 ) ) ;
#31879 = CARTESIAN_POINT ( 'NONE',  ( 0.05014649552828288198, 194.3824533091408000, 79.74886208192143044 ) ) ;
#31880 = ADVANCED_FACE ( 'NONE', ( #20467 ), #20968, .F. ) ;
#31881 = AXIS2_PLACEMENT_3D ( 'NONE', #30266, #4372, #17483 ) ;
#31882 = CARTESIAN_POINT ( 'NONE',  ( 71.29999999999999716, 163.5228861582408797, 11.73074641843673049 ) ) ;
#31883 = CARTESIAN_POINT ( 'NONE',  ( 62.01132485994281751, 167.7597621252805880, -9.270509831248443078 ) ) ;
#31884 = DIRECTION ( 'NONE',  ( 0.000000000000000000, 0.000000000000000000, -1.000000000000000000 ) ) ;
#31885 = CARTESIAN_POINT ( 'NONE',  ( -9.984503880673473830, 210.2968891136704315, 96.65113791807857524 ) ) ;
#31886 = CARTESIAN_POINT ( 'NONE',  ( -67.50000000000000000, 155.0000000000000000, 37.00000000000001421 ) ) ;
#31887 = CARTESIAN_POINT ( 'NONE',  ( 35.27499999726881441, 149.9369285172503510, -15.58253175000000823 ) ) ;
#31888 = CARTESIAN_POINT ( 'NONE',  ( -3.044812012440131443, 216.5253028482142952, 40.10113791807857098 ) ) ;
#31889 = CARTESIAN_POINT ( 'NONE',  ( 74.72499999726881015, 140.1801316387863778, -4.815267126137194431 ) ) ;
#31890 = ORIENTED_EDGE ( 'NONE', *, *, #5218, .F. ) ;
#31891 = CARTESIAN_POINT ( 'NONE',  ( 0.000000000000000000, 0.000000000000000000, 0.000000000000000000 ) ) ;
#31892 = CARTESIAN_POINT ( 'NONE',  ( 38.89999999453763024, 159.7113355953771077, 14.49999999999999289 ) ) ;
#31893 = CARTESIAN_POINT ( 'NONE',  ( 3.753561863808689836, 218.3979405102790565, 10.40113791807856636 ) ) ;
#31894 = CARTESIAN_POINT ( 'NONE',  ( -60.00000000000000000, -7.347880794884118356E-15, 270.4495957273638282 ) ) ;
#31895 = DIRECTION ( 'NONE',  ( 0.000000000000000000, 0.000000000000000000, 1.000000000000000000 ) ) ;
#31896 = ORIENTED_EDGE ( 'NONE', *, *, #3252, .F. ) ;
#31897 = CARTESIAN_POINT ( 'NONE',  ( 9.984503880673420539, 210.2968891136705736, 96.84886208192142476 ) ) ;
#31898 = CARTESIAN_POINT ( 'NONE',  ( -11.98450388067341876, 203.0532714938636047, 29.34886208192143897 ) ) ;
#31899 = CARTESIAN_POINT ( 'NONE',  ( 3.399999999999999911, 0.000000000000000000, -0.4201245229258211977 ) ) ;
#31900 = CARTESIAN_POINT ( 'NONE',  ( -10.01549611932653860, 203.7984951890123284, 51.35113791807858519 ) ) ;
#31901 = ORIENTED_EDGE ( 'NONE', *, *, #26464, .F. ) ;
#31902 = CARTESIAN_POINT ( 'NONE',  ( -7.984503880673422316, 204.3529502787951628, 11.34886208192143542 ) ) ;
#31903 = AXIS2_PLACEMENT_3D ( 'NONE', #12297, #9239, #17073 ) ;
#31904 = CARTESIAN_POINT ( 'NONE',  ( 51.41132485994281609, 142.2402378747194405, -9.270509831248439525 ) ) ;
#31905 = ORIENTED_EDGE ( 'NONE', *, *, #7291, .T. ) ;
#31906 = CARTESIAN_POINT ( 'NONE',  ( -7.984503880673422316, 204.3529502787951628, 95.34886208192143897 ) ) ;
#31907 = CARTESIAN_POINT ( 'NONE',  ( -4.903702542908602524, 213.8346818373418898, 42.95113791807857240 ) ) ;
#31908 = DIRECTION ( 'NONE',  ( -0.000000000000000000, -0.000000000000000000, -1.000000000000000000 ) ) ;
#31910 = ORIENTED_EDGE ( 'NONE', *, *, #32890, .T. ) ;
#31909 = VECTOR ( 'NONE', #2854, 1000.000000000000000 ) ;
#31911 = CARTESIAN_POINT ( 'NONE',  ( 33.12499999726880873, 155.0000000000000000, -15.58253175000000823 ) ) ;
#31912 = CARTESIAN_POINT ( 'NONE',  ( 0.05014649552828275708, 196.4853777576173002, 55.74886208192143755 ) ) ;
#31913 = CARTESIAN_POINT ( 'NONE',  ( 36.47499999726881015, 149.9369285172503510, 15.58253174999999580 ) ) ;
#31914 = CARTESIAN_POINT ( 'NONE',  ( 77.30950000000004252, 0.000000000000000000, 4.000000000000000000 ) ) ;
#31915 = CARTESIAN_POINT ( 'NONE',  ( 6.500168698208129925, 211.6636982574063381, 100.7011379180785866 ) ) ;
#31916 = CARTESIAN_POINT ( 'NONE',  ( -58.50000000000001421, -88.00000000000000000, -38.00000000000000000 ) ) ;
#31917 = CARTESIAN_POINT ( 'NONE',  ( 54.30000000000000426, 146.4771138417591203, -11.73074641843674470 ) ) ;
#31918 = CARTESIAN_POINT ( 'NONE',  ( 8.000000000000008882, 207.0476921513415220, 69.99886208192144466 ) ) ;
#31919 = AXIS2_PLACEMENT_3D ( 'NONE', #13818, #874, #21652 ) ;
#31920 = LINE ( 'NONE', #21530, #955 ) ;
#31921 = AXIS2_PLACEMENT_3D ( 'NONE', #21428, #8479, #16311 ) ;
#31922 = CARTESIAN_POINT ( 'NONE',  ( 57.72499999726881015, 169.8198683612136222, 4.815267126137181997 ) ) ;
#31923 = CARTESIAN_POINT ( 'NONE',  ( -6.220909254589537696, 198.5229672870051445, 12.05113791807856671 ) ) ;
#31924 = DIRECTION ( 'NONE',  ( 1.000000000000000000, 0.000000000000000000, 0.000000000000000000 ) ) ;
#31925 = CARTESIAN_POINT ( 'NONE',  ( 63.12499999726880873, 155.0000000000000000, -15.58253175000000823 ) ) ;
#31926 = CARTESIAN_POINT ( 'NONE',  ( 77.97499999726881015, 169.8198683612136222, 4.815267126137181997 ) ) ;
#31927 = CARTESIAN_POINT ( 'NONE',  ( 12.00000000000000711, 206.9523078486586485, 74.00113791807856956 ) ) ;
#31928 = CARTESIAN_POINT ( 'NONE',  ( 8.062137200540920645, 201.0835637161417822, 101.3011379180785809 ) ) ;
#31929 = FACE_OUTER_BOUND ( 'NONE', #32196, .T. ) ;
#31930 = AXIS2_PLACEMENT_3D ( 'NONE', #4688, #28546, #10326 ) ;
#31931 = EDGE_LOOP ( 'NONE', ( #29231, #33437, #28179, #26654, #3662, #16201, #28822 ) ) ;
#31932 = CARTESIAN_POINT ( 'NONE',  ( 8.062137200540822946, 212.9164362838583315, 3.698862081921434619 ) ) ;
#31933 = CARTESIAN_POINT ( 'NONE',  ( -3.753561863808878130, 218.3979405102790281, 60.09886208192143897 ) ) ;
#31934 = CARTESIAN_POINT ( 'NONE',  ( -9.984503880673420539, 203.7031108863293980, 62.34886208192143897 ) ) ;
#31935 = CARTESIAN_POINT ( 'NONE',  ( -9.680171189290716072, 199.9079932115567146, 2.198862081921433731 ) ) ;
#31936 = LINE ( 'NONE', #3322, #26788 ) ;
#31937 = CARTESIAN_POINT ( 'NONE',  ( -3.135527875058821579, 197.5041725223112223, 20.90113791807856813 ) ) ;
#31938 = CARTESIAN_POINT ( 'NONE',  ( 6.139770520408223575, 215.5359834540460611, 90.54886208192144181 ) ) ;
#31939 = ADVANCED_FACE ( 'NONE', ( #33584 ), #7864, .T. ) ;
#31940 = VERTEX_POINT ( 'NONE', #31038 ) ;
#31941 = FACE_OUTER_BOUND ( 'NONE', #27330, .T. ) ;
#31942 = ORIENTED_EDGE ( 'NONE', *, *, #29511, .T. ) ;
#31943 = CARTESIAN_POINT ( 'NONE',  ( 2.343682934607771440, 2.688325911136448809, -0.02993401039713653594 ) ) ;
#31944 = CARTESIAN_POINT ( 'NONE',  ( 4.903702542908435547, 213.8346818373419751, 60.54886208192144181 ) ) ;
#31945 = CIRCLE ( 'NONE', #28680, 18.00000000000000355 ) ;
#31946 = ORIENTED_EDGE ( 'NONE', *, *, #25967, .T. ) ;
#31947 = AXIS2_PLACEMENT_3D ( 'NONE', #2838, #23622, #13225 ) ;
#31948 = CARTESIAN_POINT ( 'NONE',  ( 78.02499999726879309, 160.0630714827496206, 15.58253174999999224 ) ) ;
#31949 = VERTEX_POINT ( 'NONE', #8032 ) ;
#31950 = CARTESIAN_POINT ( 'NONE',  ( 103.4083388212532810, 155.0000000000000000, 0.000000000000000000 ) ) ;
#31951 = CIRCLE ( 'NONE', #25984, 1.000000000000000888 ) ;
#31952 = CARTESIAN_POINT ( 'NONE',  ( 71.12499999726881583, 155.0000000000000000, -15.58253175000000823 ) ) ;
#31953 = CARTESIAN_POINT ( 'NONE',  ( -0.05014649552807731031, 198.5883022060938572, 65.75113791807856956 ) ) ;
#31954 = SURFACE_STYLE_FILL_AREA ( #6057 ) ;
#31955 = AXIS2_PLACEMENT_3D ( 'NONE', #3781, #24561, #21499 ) ;
#31956 = CARTESIAN_POINT ( 'NONE',  ( 11.40740920524441293, 25.16819403002535083, 4.946672411965113980E-16 ) ) ;
#31957 = CARTESIAN_POINT ( 'NONE',  ( 34.70000000000000284, 163.5228861582408797, -11.73074641843674470 ) ) ;
#31958 = CARTESIAN_POINT ( 'NONE',  ( 2.426778023690075337, 214.6231898156240447, 42.39886208192144323 ) ) ;
#31959 = CARTESIAN_POINT ( 'NONE',  ( -8.118202686958039038, 201.1607312380087080, 78.20113791807857240 ) ) ;
#31960 = CARTESIAN_POINT ( 'NONE',  ( -3.135527875058821579, 197.5041725223112223, 62.90113791807858235 ) ) ;
#31961 = DIRECTION ( 'NONE',  ( 0.000000000000000000, 0.000000000000000000, -1.000000000000000000 ) ) ;
#31962 = CARTESIAN_POINT ( 'NONE',  ( 8.015496119326531499, 209.5516654185219636, 22.85113791807856742 ) ) ;
#31963 = CARTESIAN_POINT ( 'NONE',  ( -27.50000000000000000, 15.87713240271474824, -15.54379906938135214 ) ) ;
#31964 = CARTESIAN_POINT ( 'NONE',  ( 60.18867513459482410, 140.7341522555726669, 4.635254915624211769 ) ) ;
#31965 = CARTESIAN_POINT ( 'NONE',  ( 47.32499999726881867, 164.1591823560292198, -12.60653300113719766 ) ) ;
#31966 = CARTESIAN_POINT ( 'NONE',  ( -3.662846001190052991, 218.4274158808045740, 46.10113791807857098 ) ) ;
#31967 = CARTESIAN_POINT ( 'NONE',  ( 32.50000000000000000, 155.0000000000000000, 15.00000000000001243 ) ) ;
#31968 = AXIS2_PLACEMENT_3D ( 'NONE', #3881, #9502, #30287 ) ;
#31969 = CARTESIAN_POINT ( 'NONE',  ( 0.05014649552810505201, 217.5146222423826714, 91.25113791807858377 ) ) ;
#31970 = CARTESIAN_POINT ( 'NONE',  ( -3.135527875058821579, 197.5041725223112223, 71.90113791807857524 ) ) ;
#31971 = AXIS2_PLACEMENT_3D ( 'NONE', #22744, #5477, #23080 ) ;
#31972 = AXIS2_PLACEMENT_3D ( 'NONE', #8623, #19182, #27013 ) ;
#31973 = CARTESIAN_POINT ( 'NONE',  ( 9.680171189290716072, 214.0920067884432854, 33.69886208192142618 ) ) ;
#31974 = CARTESIAN_POINT ( 'NONE',  ( 6.139770520408223575, 215.5359834540460611, 33.54886208192143471 ) ) ;
#31975 = CARTESIAN_POINT ( 'NONE',  ( 88.19999999453763451, 163.5228861582408797, -11.73074641843674470 ) ) ;
#31976 = CARTESIAN_POINT ( 'NONE',  ( -7.456977232089304408, 196.8216656703010301, 75.05113791807858092 ) ) ;
#31977 = CARTESIAN_POINT ( 'NONE',  ( -2.426778023690262742, 214.6231898156240163, 94.10113791807857808 ) ) ;
#31978 =( BOUNDED_CURVE ( )  B_SPLINE_CURVE ( 2, ( #10065, #5601, #26216, #10400, #33557, #30840, #15825, #10233, #2557, #18556, #25716 ),
 .UNSPECIFIED., .F., .T. ) 
 B_SPLINE_CURVE_WITH_KNOTS ( ( 3, 2, 2, 2, 2, 3 ),
 ( 0.5535714285714284921, 0.5571428571428570509, 0.5607142857142856096, 0.5642857142857142794, 0.5678571428571428381, 0.5714285714285713969 ),
 .UNSPECIFIED. ) 
 CURVE ( )  GEOMETRIC_REPRESENTATION_ITEM ( )  RATIONAL_B_SPLINE_CURVE ( ( 1.000000000000001554, 0.9510565162951518658, 1.000000000000000000, 0.9510565162951534202, 1.000000000000000000, 0.9510565162951534202, 1.000000000000000000, 0.9510565162951534202, 1.000000000000000000, 0.9510565162951534202, 1.000000000000000000 ) ) 
 REPRESENTATION_ITEM ( '' )  );
#31979 = CARTESIAN_POINT ( 'NONE',  ( 6.220909254589681581, 198.5229672870052582, 49.44886208192144039 ) ) ;
#31980 = EDGE_CURVE ( 'NONE', #4155, #6185, #28475, .T. ) ;
#31981 = FACE_OUTER_BOUND ( 'NONE', #21432, .T. ) ;
#31982 = AXIS2_PLACEMENT_3D ( 'NONE', #1014, #32178, #8838 ) ;
#31983 = VERTEX_POINT ( 'NONE', #5131 ) ;
#31984 = CARTESIAN_POINT ( 'NONE',  ( 12.00000000000000711, 207.0476921513415220, 60.99886208192143044 ) ) ;
#31985 = ORIENTED_EDGE ( 'NONE', *, *, #17471, .T. ) ;
#31986 = CARTESIAN_POINT ( 'NONE',  ( -7.984503880673422316, 204.3529502787951628, 32.34886208192143897 ) ) ;
#31987 = VERTEX_POINT ( 'NONE', #5465 ) ;
#31988 = CARTESIAN_POINT ( 'NONE',  ( 75.47499999726881015, 160.0630714827496206, -15.58253175000000823 ) ) ;
#31989 = DIRECTION ( 'NONE',  ( -0.000000000000000000, -0.000000000000000000, 1.000000000000000000 ) ) ;
#31990 = EDGE_CURVE ( 'NONE', #3282, #12765, #14112, .T. ) ;
#31991 = CARTESIAN_POINT ( 'NONE',  ( 115.4999999999999858, 127.5651812191323557, -102.3881375866411645 ) ) ;
#31992 = CARTESIAN_POINT ( 'NONE',  ( -4.984841277089726574, 200.2242689037092305, 51.05113791807858092 ) ) ;
#31993 = VECTOR ( 'NONE', #20185, 1000.000000000000000 ) ;
#31994 = CARTESIAN_POINT ( 'NONE',  ( 1.750000000000016209, -3.031088913245524985, -2.899999999999999911 ) ) ;
#31995 = VECTOR ( 'NONE', #10892, 1000.000000000000000 ) ;
#31996 = CARTESIAN_POINT ( 'NONE',  ( -3.135527875058982783, 216.4958274776886924, 30.09886208192143897 ) ) ;
#31997 = CARTESIAN_POINT ( 'NONE',  ( 67.07499999726880446, 141.7447067706911810, -9.630534252274387086 ) ) ;
#31998 = ORIENTED_EDGE ( 'NONE', *, *, #25399, .F. ) ;
#31999 = CARTESIAN_POINT ( 'NONE',  ( 62.18867513459482410, 140.7341522555726669, 4.635254915624211769 ) ) ;
#32000 = SHAPE_REPRESENTATION_RELATIONSHIP ( 'NONE' , 'NONE' ,  #19592, #16530 ) ;
#32001 = CARTESIAN_POINT ( 'NONE',  ( 111.1125082318798007, 155.0000000000000000, 0.000000000000000000 ) ) ;
#32002 = CARTESIAN_POINT ( 'NONE',  ( -7.984503880673422316, 204.3529502787951628, 17.34886208192143187 ) ) ;
#32003 = CARTESIAN_POINT ( 'NONE',  ( -6.139770520408369237, 215.5359834540460042, 51.95113791807857950 ) ) ;
#32004 = CARTESIAN_POINT ( 'NONE',  ( 0.000000000000000000, 0.000000000000000000, 0.000000000000000000 ) ) ;
#32005 = EDGE_CURVE ( 'NONE', #2381, #30979, #9910, .T. ) ;
#32006 = CARTESIAN_POINT ( 'NONE',  ( -8.062137200540920645, 212.9164362838581894, 39.80113791807857382 ) ) ;
#32007 = CARTESIAN_POINT ( 'NONE',  ( 81.77499999726880731, 169.8198683612136222, -4.815267126137197984 ) ) ;
#32008 = CIRCLE ( 'NONE', #17870, 0.9999999999999941158 ) ;
#32009 = CONTEXT_DEPENDENT_SHAPE_REPRESENTATION ( #6130, #5103 ) ;
#32010 = CARTESIAN_POINT ( 'NONE',  ( -8.050845014156799095, 215.4811768934071665, 104.9910338291041114 ) ) ;
#32011 = CARTESIAN_POINT ( 'NONE',  ( 39.72499999726881015, 169.8198683612136222, 4.815267126137181997 ) ) ;
#32012 = DIRECTION ( 'NONE',  ( -1.000000000000000000, -0.000000000000000000, 0.000000000000000000 ) ) ;
#32013 = CARTESIAN_POINT ( 'NONE',  ( -12.01549611932652972, 203.1486557965464499, 21.35113791807856742 ) ) ;
#32014 = CARTESIAN_POINT ( 'NONE',  ( 7.112481253774308954, -4.553861071371678726, -7.781689322728511549 ) ) ;
#32015 = CARTESIAN_POINT ( 'NONE',  ( 64.07499999726881867, 168.2552932293087906, 9.630534252274372875 ) ) ;
#32016 = ADVANCED_FACE ( 'NONE', ( #28638 ), #21378, .F. ) ;
#32017 = CARTESIAN_POINT ( 'NONE',  ( 8.118202686958039038, 212.8392687619912635, 67.70113791807858661 ) ) ;
#32018 = CARTESIAN_POINT ( 'NONE',  ( 3.135527875058820690, 216.4958274776887492, 40.40113791807857524 ) ) ;
#32019 = LINE ( 'NONE', #32183, #165 ) ;
#32020 = CARTESIAN_POINT ( 'NONE',  ( -2.243702833038388356, 30.45886237079318093, -16.29170001372754939 ) ) ;
#32021 = CARTESIAN_POINT ( 'NONE',  ( -3.662846001189865142, 195.5725841191952838, 1.898862081921434131 ) ) ;
#32022 = CARTESIAN_POINT ( 'NONE',  ( -8.118202686958138514, 212.8392687619910930, 5.798862081921434708 ) ) ;
#32023 = CARTESIAN_POINT ( 'NONE',  ( 61.09999999453762598, 150.2886644046228639, 14.49999999999999645 ) ) ;
#32024 = ORIENTED_EDGE ( 'NONE', *, *, #33659, .T. ) ;
#32025 = CARTESIAN_POINT ( 'NONE',  ( 9.680171189290831535, 199.9079932115568852, 44.30113791807857382 ) ) ;
#32026 = VECTOR ( 'NONE', #32466, 1000.000000000000000 ) ;
#32027 = CARTESIAN_POINT ( 'NONE',  ( 37.38867513459481984, 169.2658477444273331, 4.635254915624208216 ) ) ;
#32028 = CARTESIAN_POINT ( 'NONE',  ( 3.135527875058981895, 197.5041725223112792, 22.59886208192143542 ) ) ;
#32029 = EDGE_CURVE ( 'NONE', #14565, #11491, #13765, .T. ) ;
#32030 = CARTESIAN_POINT ( 'NONE',  ( 59.01132485994281751, 142.2402378747194405, 9.270509831248432420 ) ) ;
#32031 = ORIENTED_EDGE ( 'NONE', *, *, #2528, .T. ) ;
#32032 = AXIS2_PLACEMENT_3D ( 'NONE', #709, #1048, #19270 ) ;
#32033 = CARTESIAN_POINT ( 'NONE',  ( -6.220909254589537696, 198.5229672870051161, 78.05113791807858092 ) ) ;
#32034 = ORIENTED_EDGE ( 'NONE', *, *, #12448, .T. ) ;
#32035 = AXIS2_PLACEMENT_3D ( 'NONE', #9058, #15765, #26160 ) ;
#32036 = DIRECTION ( 'NONE',  ( 0.000000000000000000, -0.000000000000000000, -1.000000000000000000 ) ) ;
#32037 = CARTESIAN_POINT ( 'NONE',  ( -2.241046694638765935, -6.576374040526340892, -6.171384342982618065 ) ) ;
#32038 = ORIENTED_EDGE ( 'NONE', *, *, #32224, .F. ) ;
#32039 = CARTESIAN_POINT ( 'NONE',  ( -2.426778023690262742, 214.6231898156240163, 19.10113791807856742 ) ) ;
#32040 = ADVANCED_FACE ( 'NONE', ( #7533 ), #17740, .T. ) ;
#32041 = CYLINDRICAL_SURFACE ( 'NONE', #10718, 15.00000000000001776 ) ;
#32042 = CARTESIAN_POINT ( 'NONE',  ( -8.062137200540822946, 201.0835637161416400, 5.198862081921435063 ) ) ;
#32043 = CARTESIAN_POINT ( 'NONE',  ( 52.17499999726880588, 164.1591823560292198, 12.60653300113718167 ) ) ;
#32044 = ORIENTED_EDGE ( 'NONE', *, *, #22865, .F. ) ;
#32045 = CARTESIAN_POINT ( 'NONE',  ( 57.52499999726881441, 169.8198683612136222, -4.815267126137197984 ) ) ;
#32046 = CARTESIAN_POINT ( 'NONE',  ( 89.50000000000002842, 155.0000000000000000, 0.000000000000000000 ) ) ;
#32047 = CARTESIAN_POINT ( 'NONE',  ( 7.500000000000000888, 4.330127018922190985, -7.564338275809340928 ) ) ;
#32048 = DIRECTION ( 'NONE',  ( 1.000000000000000000, -0.000000000000000000, -0.000000000000000000 ) ) ;
#32049 = VECTOR ( 'NONE', #5338, 1000.000000000000000 ) ;
#32050 = CARTESIAN_POINT ( 'NONE',  ( 3.135527875058981895, 197.5041725223112792, 88.59886208192143897 ) ) ;
#32051 = CARTESIAN_POINT ( 'NONE',  ( 60.77499999726881441, 140.1801316387863778, 4.815267126137185549 ) ) ;
#32052 = CARTESIAN_POINT ( 'NONE',  ( 6.139770520408368348, 198.4640165459539674, 23.45113791807856884 ) ) ;
#32053 = CARTESIAN_POINT ( 'NONE',  ( 72.88867513459481984, 159.8737954434938615, -14.99999999999984190 ) ) ;
#32054 = ADVANCED_FACE ( 'NONE', ( #12624 ), #9422, .T. ) ;
#32055 = CARTESIAN_POINT ( 'NONE',  ( 0.05014649552828288198, 194.3824533091408000, 76.74886208192144466 ) ) ;
#32056 = CARTESIAN_POINT ( 'NONE',  ( 72.59999999999996589, 159.7113355953771077, -14.50000000000000888 ) ) ;
#32057 = CARTESIAN_POINT ( 'NONE',  ( 125.5000000000000000, 157.1499999999996362, -106.0000000000000284 ) ) ;
#32058 = CARTESIAN_POINT ( 'NONE',  ( -1.083333333333333259, 6.880090707843040221, -5.848636054922037530 ) ) ;
#32059 = CARTESIAN_POINT ( 'NONE',  ( -8.062137200540920645, 212.9164362838581894, 93.80113791807858092 ) ) ;
#32060 = CARTESIAN_POINT ( 'NONE',  ( 33.48867513459482836, 167.7597621252805880, 9.270509831248428867 ) ) ;
#32061 = CARTESIAN_POINT ( 'NONE',  ( 43.97499999726881015, 169.8198683612136222, 4.815267126137181997 ) ) ;
#32062 = EDGE_CURVE ( 'NONE', #10890, #25762, #30083, .T. ) ;
#32063 = CARTESIAN_POINT ( 'NONE',  ( -6.220909254589537696, 198.5229672870051161, 36.05113791807857382 ) ) ;
#32064 =( REPRESENTATION_RELATIONSHIP ('NONE','NONE', #25663, #19592 ) REPRESENTATION_RELATIONSHIP_WITH_TRANSFORMATION ( #8672 )SHAPE_REPRESENTATION_RELATIONSHIP( ) );
#32065 = CARTESIAN_POINT ( 'NONE',  ( 74.82499999726881867, 141.7447067706911810, -9.630534252274385310 ) ) ;
#32066 = ORIENTED_EDGE ( 'NONE', *, *, #23461, .T. ) ;
#32067 = CARTESIAN_POINT ( 'NONE',  ( 4.102348501002488490, 207.3577873115561943, -8.835681806194324750 ) ) ;
#32068 = CARTESIAN_POINT ( 'NONE',  ( 44.19999999453762740, 163.5228861582408797, -11.73074641843674470 ) ) ;
#32069 = CARTESIAN_POINT ( 'NONE',  ( -12.00000000000000711, 207.0476921513413515, 24.50113791807856600 ) ) ;
#32070 = CARTESIAN_POINT ( 'NONE',  ( 115.4999999999999858, 248.9486928011511679, 52.99999999999880629 ) ) ;
#32071 = CARTESIAN_POINT ( 'NONE',  ( -5.147825380260782957, -5.688155668810408017, -7.450218641351304960 ) ) ;
#32072 = ORIENTED_EDGE ( 'NONE', *, *, #12430, .T. ) ;
#32073 = CARTESIAN_POINT ( 'NONE',  ( 12.00000000000000711, 207.0476921513415220, 30.99886208192143400 ) ) ;
#32074 = CARTESIAN_POINT ( 'NONE',  ( 52.78867513459482552, 155.0000000000000000, -15.00000000000002487 ) ) ;
#32075 = AXIS2_PLACEMENT_3D ( 'NONE', #19955, #14502, #32227 ) ;
#32076 = CARTESIAN_POINT ( 'NONE',  ( 6.220909254589536808, 215.4770327129947702, 52.55113791807858092 ) ) ;
#32077 = ORIENTED_EDGE ( 'NONE', *, *, #23883, .F. ) ;
#32078 = CARTESIAN_POINT ( 'NONE',  ( -0.05014649552828365914, 215.4116977939061144, 12.24886208192143577 ) ) ;
#32079 = CARTESIAN_POINT ( 'NONE',  ( 51.71132485994281325, 155.0000000000000000, -15.00000000000002487 ) ) ;
#32080 = ORIENTED_EDGE ( 'NONE', *, *, #19116, .F. ) ;
#32081 = CARTESIAN_POINT ( 'NONE',  ( -8.000000000000008882, 206.9523078486584780, 95.49886208192144466 ) ) ;
#32082 = EDGE_CURVE ( 'NONE', #10180, #25466, #28968, .T. ) ;
#32083 = CARTESIAN_POINT ( 'NONE',  ( 6.444103211791042618, 202.2591342207267644, 41.30113791807857382 ) ) ;
#32084 = CARTESIAN_POINT ( 'NONE',  ( 0.000000000000000000, 0.000000000000000000, 0.000000000000000000 ) ) ;
#32085 = ORIENTED_EDGE ( 'NONE', *, *, #32471, .F. ) ;
#32086 = CARTESIAN_POINT ( 'NONE',  ( 39.62499999726880162, 171.3844434931184253, -7.942151717890132712E-15 ) ) ;
#32087 = CARTESIAN_POINT ( 'NONE',  ( 0.05014649552828275708, 196.4853777576173002, 61.74886208192143755 ) ) ;
#32088 = CARTESIAN_POINT ( 'NONE',  ( 37.67499999726881299, 168.2552932293087906, -9.630534252274385310 ) ) ;
#32089 = CARTESIAN_POINT ( 'NONE',  ( -6.500000000000000000, 2.501851166488374911, -5.848636054922034866 ) ) ;
#32090 = CARTESIAN_POINT ( 'NONE',  ( 0.05014649552807626948, 215.4116977939061144, 97.25113791807856956 ) ) ;
#32091 = EDGE_CURVE ( 'NONE', #10396, #30404, #24187, .T. ) ;
#32092 = CARTESIAN_POINT ( 'NONE',  ( 51.50000000000000711, 155.0000000000000000, 14.49999999999999467 ) ) ;
#32093 = CARTESIAN_POINT ( 'NONE',  ( 4.903702542908435547, 213.8346818373419751, 72.54886208192141339 ) ) ;
#32094 = CARTESIAN_POINT ( 'NONE',  ( 75.71132485994280614, 155.0000000000000000, -15.00000000000002487 ) ) ;
#32095 = CARTESIAN_POINT ( 'NONE',  ( 56.72499999726881015, 140.1801316387863778, -4.815267126137194431 ) ) ;
#32097 = ORIENTED_EDGE ( 'NONE', *, *, #24751, .T. ) ;
#32096 = CARTESIAN_POINT ( 'NONE',  ( 10.01549611932653860, 210.2015048109876716, 13.85113791807856742 ) ) ;
#32098 = CARTESIAN_POINT ( 'NONE',  ( -6.826580258811596025, 2.695816818222440681, -6.331007506863580048 ) ) ;
#32099 = CARTESIAN_POINT ( 'NONE',  ( 66.02499999726879309, 160.0630714827496206, 15.58253174999999224 ) ) ;
#32100 = CARTESIAN_POINT ( 'NONE',  ( 79.17499999726881299, 145.8408176439707802, -12.60653300113719588 ) ) ;
#32101 = CARTESIAN_POINT ( 'NONE',  ( 3.662846001190051659, 195.5725841191953691, 77.60113791807854966 ) ) ;
#32102 = CARTESIAN_POINT ( 'NONE',  ( -6.220909254589537696, 198.5229672870051445, 99.05113791807858092 ) ) ;
#32103 = CARTESIAN_POINT ( 'NONE',  ( 83.98867513459481415, 146.1832212156128890, 12.13525491562421976 ) ) ;
#32104 = VERTEX_POINT ( 'NONE', #31529 ) ;
#32105 = CARTESIAN_POINT ( 'NONE',  ( 6.220909254589681581, 198.5229672870052582, 1.448862081921434397 ) ) ;
#32106 = CARTESIAN_POINT ( 'NONE',  ( -12.00000000000000711, 206.9523078486584780, 65.49886208192144466 ) ) ;
#32107 = CARTESIAN_POINT ( 'NONE',  ( 3.044812012439969795, 216.5253028482143520, 63.39886208192144323 ) ) ;
#32108 = CARTESIAN_POINT ( 'NONE',  ( 3.662846001190051659, 195.5725841191953691, 101.6011379180785781 ) ) ;
#32109 = CARTESIAN_POINT ( 'NONE',  ( -67.50001199999999812, 162.5335705082559059, -15.28016032735712493 ) ) ;
#32110 = CARTESIAN_POINT ( 'NONE',  ( -10.01549611932653860, 203.7984951890123284, 27.35113791807856742 ) ) ;
#32111 = CARTESIAN_POINT ( 'NONE',  ( 8.118202686958138514, 201.1607312380088501, 91.29886208192144181 ) ) ;
#32112 = VERTEX_POINT ( 'NONE', #13621 ) ;
#32113 = CARTESIAN_POINT ( 'NONE',  ( 10.20891672561132424, 208.8253170565643302, -1.573594014082846382 ) ) ;
#32114 = ORIENTED_EDGE ( 'NONE', *, *, #20169, .F. ) ;
#32115 = DIRECTION ( 'NONE',  ( -1.000000000000000000, 0.000000000000000000, 0.000000000000000000 ) ) ;
#32116 = CARTESIAN_POINT ( 'NONE',  ( 8.015496119326595448, 204.4483345814782638, 73.14886208192142192 ) ) ;
#32117 = ORIENTED_EDGE ( 'NONE', *, *, #15204, .F. ) ;
#32118 = CARTESIAN_POINT ( 'NONE',  ( 84.62499999726880162, 138.6155565068815747, -3.929120461958505118E-15 ) ) ;
#32119 = ORIENTED_EDGE ( 'NONE', *, *, #16647, .T. ) ;
#32120 = DIRECTION ( 'NONE',  ( -0.000000000000000000, -0.000000000000000000, -1.000000000000000000 ) ) ;
#32121 = CARTESIAN_POINT ( 'NONE',  ( 68.62499999726880162, 138.6155565068815463, -3.929120461958505118E-15 ) ) ;
#32122 = CARTESIAN_POINT ( 'NONE',  ( 8.000000000000008882, 206.9523078486586485, 65.00113791807856956 ) ) ;
#32123 = DIRECTION ( 'NONE',  ( -0.000000000000000000, -0.000000000000000000, 1.000000000000000000 ) ) ;
#32124 = CARTESIAN_POINT ( 'NONE',  ( 58.50000000000001421, -88.00000000000000000, 20.00000000000000000 ) ) ;
#32125 = AXIS2_PLACEMENT_3D ( 'NONE', #5934, #24001, #24331 ) ;
#32126 = SURFACE_SIDE_STYLE ('',( #16957 ) ) ;
#32127 = CARTESIAN_POINT ( 'NONE',  ( 37.80000000000000426, 142.6655632788954620, 8.961492836873471646 ) ) ;
#32128 = CARTESIAN_POINT ( 'NONE',  ( -4.903702542908436435, 200.1653181626580249, 44.04886208192144181 ) ) ;
#32129 = CARTESIAN_POINT ( 'NONE',  ( 6.139770520408368348, 198.4640165459539674, 86.45113791807854398 ) ) ;
#32130 = CARTESIAN_POINT ( 'NONE',  ( 0.05014649552810505201, 217.5146222423826714, 67.25113791807856956 ) ) ;
#32131 = PLANE ( 'NONE',  #17531 ) ;
#32132 = CARTESIAN_POINT ( 'NONE',  ( 4.984841277089725686, 213.7757310962907411, 25.55113791807857027 ) ) ;
#32133 = CARTESIAN_POINT ( 'NONE',  ( 1.206569728928466700, 7.963640680051486953, -0.4524126574264497602 ) ) ;
#32134 = CARTESIAN_POINT ( 'NONE',  ( 6.500000000000000000, -2.501851166488383349, -5.848636054922036642 ) ) ;
#32135 = CARTESIAN_POINT ( 'NONE',  ( 45.62499999726880162, 171.3844434931184253, -7.942151717890134290E-15 ) ) ;
#32136 = CARTESIAN_POINT ( 'NONE',  ( -3.662846001190052991, 218.4274158808045740, 52.10113791807857808 ) ) ;
#32137 = DIRECTION ( 'NONE',  ( -0.9891821073486148919, -0.1466927349985451545, 0.000000000000000000 ) ) ;
#32138 = CARTESIAN_POINT ( 'NONE',  ( 10.01549611932653860, 210.2015048109876716, 97.85113791807857808 ) ) ;
#32139 = CARTESIAN_POINT ( 'NONE',  ( 3.135527875058820690, 216.4958274776887492, 70.40113791807857524 ) ) ;
#32140 = CARTESIAN_POINT ( 'NONE',  ( -0.05014649552828442242, 219.6175466908591716, 30.24886208192143755 ) ) ;
#32141 = CARTESIAN_POINT ( 'NONE',  ( -10.00000000000000711, 206.9523078486584495, 35.49886208192143044 ) ) ;
#32142 = CARTESIAN_POINT ( 'NONE',  ( 87.89999999453760893, 150.2886644046228639, -14.50000000000000888 ) ) ;
#32143 = CARTESIAN_POINT ( 'NONE',  ( 3.753561863808689836, 218.3979405102790565, 76.40113791807856103 ) ) ;
#32144 = CARTESIAN_POINT ( 'NONE',  ( 7.984503880673485376, 204.3529502787953902, 95.15113791807856103 ) ) ;
#32145 = CARTESIAN_POINT ( 'NONE',  ( -6.139770520408224463, 198.4640165459539389, 62.04886208192142050 ) ) ;
#32146 = CARTESIAN_POINT ( 'NONE',  ( 7.922281120364393914, 4.573931137438269623, -8.047472243342930653 ) ) ;
#32147 = ORIENTED_EDGE ( 'NONE', *, *, #29739, .T. ) ;
#32148 = CARTESIAN_POINT ( 'NONE',  ( -3.753561863808878130, 218.3979405102790281, 57.09886208192143897 ) ) ;
#32149 = AXIS2_PLACEMENT_3D ( 'NONE', #17683, #25014, #9674 ) ;
#32150 = ORIENTED_EDGE ( 'NONE', *, *, #17637, .T. ) ;
#32151 = CARTESIAN_POINT ( 'NONE',  ( 71.17499999726881299, 145.8408176439707802, -12.60653300113719588 ) ) ;
#32152 = CARTESIAN_POINT ( 'NONE',  ( 6.500168698208244500, 202.3363017425938324, 43.29886208192144181 ) ) ;
#32153 = VERTEX_POINT ( 'NONE', #24019 ) ;
#32154 = CARTESIAN_POINT ( 'NONE',  ( 76.87499999726881583, 138.6155565068815747, -3.929120461958505118E-15 ) ) ;
#32155 = FACE_OUTER_BOUND ( 'NONE', #15023, .T. ) ;
#32156 = DIRECTION ( 'NONE',  ( 0.000000000000000000, 0.000000000000000000, -1.000000000000000000 ) ) ;
#32157 = CARTESIAN_POINT ( 'NONE',  ( 2.517493886308900919, 214.5937144450984420, 52.40113791807858235 ) ) ;
#32158 = LINE ( 'NONE', #32329, #31388 ) ;
#32159 = CARTESIAN_POINT ( 'NONE',  ( 3.135527875058981895, 197.5041725223112792, 37.59886208192143187 ) ) ;
#32160 = CARTESIAN_POINT ( 'NONE',  ( 66.27499999726880731, 160.0630714827496206, 15.58253174999999224 ) ) ;
#32161 = EDGE_LOOP ( 'NONE', ( #7846, #1868 ) ) ;
#32162 = CARTESIAN_POINT ( 'NONE',  ( 35.81132485994280756, 159.8737954434936626, -15.00000000000000178 ) ) ;
#32163 = SURFACE_SIDE_STYLE ('',( #17168 ) ) ;
#32164 = DIRECTION ( 'NONE',  ( 0.000000000000000000, 0.000000000000000000, -1.000000000000000000 ) ) ;
#32165 = CARTESIAN_POINT ( 'NONE',  ( -7.297096662748653293E-16, -8.716842316802402735, -7.700127545397317697 ) ) ;
#32166 = CARTESIAN_POINT ( 'NONE',  ( 0.05014649552828262524, 198.5883022060938572, 19.74886208192143400 ) ) ;
#32167 = CARTESIAN_POINT ( 'NONE',  ( 3.135527875058820690, 216.4958274776887492, 55.40113791807857524 ) ) ;
#32168 = ADVANCED_FACE ( 'NONE', ( #1019 ), #29133, .F. ) ;
#32169 = CARTESIAN_POINT ( 'NONE',  ( -3.135527875058821579, 197.5041725223112223, 41.90113791807856813 ) ) ;
#32170 = CARTESIAN_POINT ( 'NONE',  ( 85.97499999726882436, 169.8198683612136222, 4.815267126137181997 ) ) ;
#32171 = PRODUCT_CONTEXT ( 'NONE', #16582, 'mechanical' ) ;
#32172 = AXIS2_PLACEMENT_3D ( 'NONE', #25944, #2950, #30902 ) ;
#32173 = CARTESIAN_POINT ( 'NONE',  ( -6.444103211790928043, 202.2591342207265939, 101.1988620819214475 ) ) ;
#32174 = CARTESIAN_POINT ( 'NONE',  ( 44.32499999726881157, 145.8408176439707802, 12.60653300113718345 ) ) ;
#32175 = FILL_AREA_STYLE_COLOUR ( '', #1869 ) ;
#32176 = PLANE ( 'NONE',  #18531 ) ;
#32177 = CARTESIAN_POINT ( 'NONE',  ( 3.662846001190051659, 195.5725841191953691, 17.60113791807856742 ) ) ;
#32178 = DIRECTION ( 'NONE',  ( -1.000000000000000000, -0.000000000000000000, -0.000000000000000000 ) ) ;
#32179 = B_SPLINE_CURVE_WITH_KNOTS ( 'NONE', 3,
 ( #16289, #26678, #3340, #13727, #31956, #19019 ),
 .UNSPECIFIED., .F., .F.,
 ( 4, 2, 4 ),
 ( 2.380727408881369683E-07, 0.008032766472079767850, 0.01606529487141864984 ),
 .UNSPECIFIED. ) ;
#32180 =( BOUNDED_CURVE ( )  B_SPLINE_CURVE ( 2, ( #5987, #29670, #24559, #16375, #3104, #32385, #13492, #6322, #1215, #9049, #19441 ),
 .UNSPECIFIED., .F., .T. ) 
 B_SPLINE_CURVE_WITH_KNOTS ( ( 3, 2, 2, 2, 2, 3 ),
 ( 0.8392857142857141906, 0.8428571428571427493, 0.8464285714285714191, 0.8499999999999999778, 0.8535714285714285365, 0.8571428571428570953 ),
 .UNSPECIFIED. ) 
 CURVE ( )  GEOMETRIC_REPRESENTATION_ITEM ( )  RATIONAL_B_SPLINE_CURVE ( ( 1.000000000000000000, 0.9510565162951534202, 1.000000000000000000, 0.9510565162951534202, 1.000000000000000000, 0.9510565162951534202, 1.000000000000000000, 0.9510565162951534202, 1.000000000000000000, 0.9510565162951534202, 1.000000000000000000 ) ) 
 REPRESENTATION_ITEM ( '' )  );
#32181 = CARTESIAN_POINT ( 'NONE',  ( 3.044812012440130555, 197.4746971517856764, 68.60113791807857808 ) ) ;
#32182 = CARTESIAN_POINT ( 'NONE',  ( -3.135527875058821579, 197.5041725223112223, 41.90113791807856813 ) ) ;
#32183 = CARTESIAN_POINT ( 'NONE',  ( 60.63708498984762940, 155.0000000000000000, -40.00000000000000000 ) ) ;
#32184 = CARTESIAN_POINT ( 'NONE',  ( 13.75000000000002487, 23.81569860407205397, -18.00000000000000000 ) ) ;
#32185 = CARTESIAN_POINT ( 'NONE',  ( -0.05014649552807705357, 194.3824533091408000, 101.7511379180785696 ) ) ;
#32186 = CARTESIAN_POINT ( 'NONE',  ( 0.05014649552828275014, 196.4853777576173002, 4.748862081921433997 ) ) ;
#32187 = CARTESIAN_POINT ( 'NONE',  ( 63.69999999453762740, 142.6655632788954620, -8.961492836873480528 ) ) ;
#32188 = CIRCLE ( 'NONE', #7175, 98.00000000000000000 ) ;
#32189 = EDGE_LOOP ( 'NONE', ( #25590, #15416 ) ) ;
#32190 = CARTESIAN_POINT ( 'NONE',  ( -3.662846001190052991, 218.4274158808045740, 49.10113791807857808 ) ) ;
#32191 = CARTESIAN_POINT ( 'NONE',  ( 2.517493886308900919, 214.5937144450984420, 70.40113791807856103 ) ) ;
#32192 = CARTESIAN_POINT ( 'NONE',  ( -0.05014649552828403384, 217.5146222423826714, 33.24886208192142334 ) ) ;
#32193 = CARTESIAN_POINT ( 'NONE',  ( 45.71132485994280614, 155.0000000000000000, -15.00000000000002487 ) ) ;
#32194 = ORIENTED_EDGE ( 'NONE', *, *, #9929, .T. ) ;
#32195 = CARTESIAN_POINT ( 'NONE',  ( 8.118202686958039038, 212.8392687619912635, 79.70113791807857240 ) ) ;
#32196 = EDGE_LOOP ( 'NONE', ( #25581, #2472, #15821, #27259 ) ) ;
#32197 = DIRECTION ( 'NONE',  ( -0.000000000000000000, -0.000000000000000000, 1.000000000000000000 ) ) ;
#32198 = LINE ( 'NONE', #21980, #22522 ) ;
#32199 = ORIENTED_EDGE ( 'NONE', *, *, #3127, .T. ) ;
#32200 = CARTESIAN_POINT ( 'NONE',  ( 2.426778023690261410, 199.3768101843759837, 23.60113791807857098 ) ) ;
#32201 = EDGE_CURVE ( 'NONE', #17836, #30489, #28477, .T. ) ;
#32202 = CARTESIAN_POINT ( 'NONE',  ( 3.499999999999999556, 0.000000000000000000, 0.000000000000000000 ) ) ;
#32203 = CARTESIAN_POINT ( 'NONE',  ( 0.05014649552828275708, 196.4853777576173002, 4.748862081921434886 ) ) ;
#32204 = CARTESIAN_POINT ( 'NONE',  ( 50.67499999726880588, 141.7447067706911810, 9.630534252274376428 ) ) ;
#32205 = ORIENTED_EDGE ( 'NONE', *, *, #17026, .T. ) ;
#32206 = CARTESIAN_POINT ( 'NONE',  ( 58.52499999726881441, 140.1801316387863778, 4.815267126137185549 ) ) ;
#32207 = DIRECTION ( 'NONE',  ( 0.000000000000000000, 1.000000000000000000, -0.000000000000000000 ) ) ;
#32208 = DIRECTION ( 'NONE',  ( -1.000000000000000000, -0.000000000000000000, -0.000000000000000000 ) ) ;
#32209 = CARTESIAN_POINT ( 'NONE',  ( -27.50000000000000000, 15.87713240271469672, -2.456200930618631428 ) ) ;
#32210 = CARTESIAN_POINT ( 'NONE',  ( 8.062137200540822946, 212.9164362838583315, 93.69886208192143329 ) ) ;
#32211 = CARTESIAN_POINT ( 'NONE',  ( 60.37499999726880873, 155.0000000000000000, 15.58253174999999402 ) ) ;
#32212 = CARTESIAN_POINT ( 'NONE',  ( 6.220909254589536808, 215.4770327129947702, 25.55113791807856671 ) ) ;
#32213 = CARTESIAN_POINT ( 'NONE',  ( 72.98867513459481415, 163.8167787843871110, -12.13525491562423397 ) ) ;
#32214 = EDGE_CURVE ( 'NONE', #30105, #17836, #32781, .T. ) ;
#32215 = CARTESIAN_POINT ( 'NONE',  ( 11.98450388067341876, 210.9467285061363953, 78.84886208192143897 ) ) ;
#32216 = CARTESIAN_POINT ( 'NONE',  ( 74.50000000000001421, 155.0000000000000000, -14.50000000000000711 ) ) ;
#32217 = DIRECTION ( 'NONE',  ( 0.000000000000000000, 0.000000000000000000, -1.000000000000000000 ) ) ;
#32218 = LINE ( 'NONE', #16376, #9892 ) ;
#32219 = CARTESIAN_POINT ( 'NONE',  ( -6.220909254589537696, 198.5229672870051161, 93.05113791807853829 ) ) ;
#32220 = CARTESIAN_POINT ( 'NONE',  ( 125.5000000000000000, 80.04668119422662187, 74.95331880577468553 ) ) ;
#32221 = CARTESIAN_POINT ( 'NONE',  ( 43.27499999726880020, 149.9369285172503510, -15.58253175000000823 ) ) ;
#32222 = CARTESIAN_POINT ( 'NONE',  ( 6.139770520408368348, 198.4640165459539674, 41.45113791807857240 ) ) ;
#32223 = CARTESIAN_POINT ( 'NONE',  ( 75.42499999726879878, 168.2552932293087906, -9.630534252274385310 ) ) ;
#32224 = EDGE_CURVE ( 'NONE', #9110, #10473, #849, .T. ) ;
#32225 = ORIENTED_EDGE ( 'NONE', *, *, #16433, .T. ) ;
#32226 = AXIS2_PLACEMENT_3D ( 'NONE', #32549, #30176, #6833 ) ;
#32227 = DIRECTION ( 'NONE',  ( 0.000000000000000000, 0.000000000000000000, 1.000000000000000000 ) ) ;
#32228 = CARTESIAN_POINT ( 'NONE',  ( 45.29999999453762172, 142.6655632788954620, 8.961492836873471646 ) ) ;
#32229 = CARTESIAN_POINT ( 'NONE',  ( -7.375838497908182134, 217.2372850707499765, 21.95113791807856884 ) ) ;
#32230 = PLANE ( 'NONE',  #21036 ) ;
#32231 = ORIENTED_EDGE ( 'NONE', *, *, #15768, .T. ) ;
#32232 = CARTESIAN_POINT ( 'NONE',  ( 9.680171189290716072, 214.0920067884432854, 30.69886208192143684 ) ) ;
#32233 = CARTESIAN_POINT ( 'NONE',  ( 6.500000000000000888, 0.000000000000000000, 0.000000000000000000 ) ) ;
#32234 = CARTESIAN_POINT ( 'NONE',  ( 6.139770520408368348, 198.4640165459539674, 47.45113791807857950 ) ) ;
#32235 = ORIENTED_EDGE ( 'NONE', *, *, #23741, .T. ) ;
#32236 = AXIS2_PLACEMENT_3D ( 'NONE', #12002, #14396, #19839 ) ;
#32237 = EDGE_CURVE ( 'NONE', #14046, #20137, #26276, .T. ) ;
#32238 = CARTESIAN_POINT ( 'NONE',  ( -4.903702542908436435, 200.1653181626580249, 17.04886208192143471 ) ) ;
#32239 = PRODUCT_DEFINITION_CONTEXT ( 'detailed design', #20725, 'design' ) ;
#32240 = DIRECTION ( 'NONE',  ( -1.000000000000000000, 0.000000000000000000, 0.000000000000000000 ) ) ;
#32241 = ORIENTED_EDGE ( 'NONE', *, *, #32838, .F. ) ;
#32242 = CARTESIAN_POINT ( 'NONE',  ( 4.903702542908435547, 213.8346818373419751, 96.54886208192142760 ) ) ;
#32243 = CARTESIAN_POINT ( 'NONE',  ( 0.000000000000000000, 0.000000000000000000, -18.00000000000000000 ) ) ;
#32244 = CARTESIAN_POINT ( 'NONE',  ( 4.984841277089725686, 213.7757310962907411, 43.55113791807857382 ) ) ;
#32245 = DIRECTION ( 'NONE',  ( 1.000000000000000000, 0.000000000000000000, 0.000000000000000000 ) ) ;
#32246 = ORIENTED_EDGE ( 'NONE', *, *, #10771, .T. ) ;
#32247 = CARTESIAN_POINT ( 'NONE',  ( 36.92499999726880588, 145.8408176439707802, -12.60653300113719588 ) ) ;
#32248 = AXIS2_PLACEMENT_3D ( 'NONE', #11574, #30306, #9520 ) ;
#32249 = CARTESIAN_POINT ( 'NONE',  ( -3.135527875058982783, 216.4958274776886924, 60.09886208192143897 ) ) ;
#32250 = CARTESIAN_POINT ( 'NONE',  ( 41.17499999726881299, 145.8408176439707802, -12.60653300113719588 ) ) ;
#32251 = DIRECTION ( 'NONE',  ( 0.000000000000000000, 0.000000000000000000, 1.000000000000000000 ) ) ;
#32252 = CARTESIAN_POINT ( 'NONE',  ( -8.015496119326531499, 204.4483345814780364, 93.35113791807857808 ) ) ;
#32253 = PRODUCT ( 'air chamber shell front', 'air chamber shell front', '', ( #32171 ) ) ;
#32254 = VECTOR ( 'NONE', #10622, 1000.000000000000000 ) ;
#32255 = CARTESIAN_POINT ( 'NONE',  ( 51.70000000000000284, 146.4771138417591203, 11.73074641843673227 ) ) ;
#32256 = FACE_BOUND ( 'NONE', #21515, .T. ) ;
#32257 = CARTESIAN_POINT ( 'NONE',  ( 0.05014649552828262524, 198.5883022060938572, 73.74886208192144466 ) ) ;
#32258 = CARTESIAN_POINT ( 'NONE',  ( 77.78867513459483973, 155.0000000000000000, 15.00000000000001243 ) ) ;
#32259 = CARTESIAN_POINT ( 'NONE',  ( 97.30927364589244632, 155.0000000000000000, 0.000000000000000000 ) ) ;
#32260 = AXIS2_PLACEMENT_3D ( 'NONE', #28062, #20404, #4724 ) ;
#32261 = CARTESIAN_POINT ( 'NONE',  ( 58.42499999726879878, 141.7447067706911810, 9.630534252274376428 ) ) ;
#32263 = VERTEX_POINT ( 'NONE', #21626 ) ;
#32262 = CARTESIAN_POINT ( 'NONE',  ( 6.139770520408367460, 198.4640165459539389, 11.45113791807856707 ) ) ;
#32264 = DIRECTION ( 'NONE',  ( -1.000000000000000000, 0.000000000000000000, 0.000000000000000000 ) ) ;
#32265 = CARTESIAN_POINT ( 'NONE',  ( 74.97499999726881015, 140.1801316387863778, -4.815267126137194431 ) ) ;
#32266 = CARTESIAN_POINT ( 'NONE',  ( -7.456977232089304408, 196.8216656703010301, 81.05113791807856671 ) ) ;
#32267 = EDGE_CURVE ( 'NONE', #33308, #25011, #8513, .T. ) ;
#32268 = EDGE_CURVE ( 'NONE', #27806, #21434, #15333, .T. ) ;
#32269 = CARTESIAN_POINT ( 'NONE',  ( -6.220909254589537696, 198.5229672870051445, 96.05113791807858092 ) ) ;
#32270 = PLANE ( 'NONE',  #27035 ) ;
#32271 = ORIENTED_EDGE ( 'NONE', *, *, #14533, .F. ) ;
#32272 = CARTESIAN_POINT ( 'NONE',  ( -10.01549611932659722, 210.2015048109875011, 5.648862081921435241 ) ) ;
#32273 = CARTESIAN_POINT ( 'NONE',  ( 7.375838497908012492, 217.2372850707501186, 57.54886208192142760 ) ) ;
#32274 = VECTOR ( 'NONE', #25980, 1000.000000000000000 ) ;
#32275 = CARTESIAN_POINT ( 'NONE',  ( 8.062137200540822946, 212.9164362838583315, 75.69886208192143329 ) ) ;
#32276 = CARTESIAN_POINT ( 'NONE',  ( 9.736236675708031640, 199.9851607334238963, 7.298862081921434708 ) ) ;
#32277 = DIRECTION ( 'NONE',  ( -0.000000000000000000, -0.000000000000000000, -1.000000000000000000 ) ) ;
#32278 = CARTESIAN_POINT ( 'NONE',  ( 10.00000000000000711, 206.9523078486586201, 26.00113791807856956 ) ) ;
#32279 = PRODUCT_DEFINITION ( 'UNKNOWN', '', #19725, #16570 ) ;
#32280 = EDGE_CURVE ( 'NONE', #28851, #250, #32019, .T. ) ;
#32281 = CARTESIAN_POINT ( 'NONE',  ( -9.984503880673420539, 203.7031108863293980, 92.34886208192141055 ) ) ;
#32282 = VERTEX_POINT ( 'NONE', #5781 ) ;
#32283 = FACE_OUTER_BOUND ( 'NONE', #19548, .T. ) ;
#32284 = CIRCLE ( 'NONE', #5639, 13.50000000000001066 ) ;
#32285 = ORIENTED_EDGE ( 'NONE', *, *, #17294, .F. ) ;
#32286 = CARTESIAN_POINT ( 'NONE',  ( -5.416666666666667851, -4.378239541354669306, -5.848636054922036642 ) ) ;
#32287 = CARTESIAN_POINT ( 'NONE',  ( 6.500168698208244500, 202.3363017425938324, 73.29886208192142760 ) ) ;
#32288 = CIRCLE ( 'NONE', #32818, 4.057500000000000107 ) ;
#32289 = ADVANCED_FACE ( 'NONE', ( #19243 ), #8198, .F. ) ;
#32290 = ORIENTED_EDGE ( 'NONE', *, *, #24751, .F. ) ;
#32291 = CIRCLE ( 'NONE', #2394, 112.0000000000000711 ) ;
#32292 = CARTESIAN_POINT ( 'NONE',  ( 81.82499999726879025, 168.2552932293087906, 9.630534252274372875 ) ) ;
#32293 = EDGE_LOOP ( 'NONE', ( #3496, #24168, #13837 ) ) ;
#32294 = DIRECTION ( 'NONE',  ( -0.8289387912553660698, 0.000000000000000000, 0.5593393248754217062 ) ) ;
#32295 = CARTESIAN_POINT ( 'NONE',  ( 74.82499999726881867, 141.7447067706911810, -9.630534252274385310 ) ) ;
#32296 = CARTESIAN_POINT ( 'NONE',  ( -0.05014649552807731031, 198.5883022060938572, 71.75113791807856956 ) ) ;
#32297 = CARTESIAN_POINT ( 'NONE',  ( 87.50000000000001421, 167.6893833810455305, 8.204385406124638180 ) ) ;
#32298 =( GEOMETRIC_REPRESENTATION_CONTEXT ( 3 ) GLOBAL_UNCERTAINTY_ASSIGNED_CONTEXT ( ( #13391 ) ) GLOBAL_UNIT_ASSIGNED_CONTEXT ( ( #17898, #30682, #7848 ) ) REPRESENTATION_CONTEXT ( 'NONE', 'WORKASPACE' ) );
#32299 = CARTESIAN_POINT ( 'NONE',  ( 36.79999999999999716, 167.3344367211045096, -8.961492836873482304 ) ) ;
#32300 = CARTESIAN_POINT ( 'NONE',  ( 2.517493886309087436, 199.4062855549015865, 43.59886208192144608 ) ) ;
#32301 = CARTESIAN_POINT ( 'NONE',  ( 3.135527875058820690, 216.4958274776887492, 88.40113791807857524 ) ) ;
#32302 = CARTESIAN_POINT ( 'NONE',  ( 8.062137200540920645, 201.0835637161417822, 62.30113791807858092 ) ) ;
#32303 = DIRECTION ( 'NONE',  ( 0.000000000000000000, 0.000000000000000000, -1.000000000000000000 ) ) ;
#32304 = CARTESIAN_POINT ( 'NONE',  ( 5.000000000000000000, 0.000000000000000000, 4.057500000000000107 ) ) ;
#32305 = AXIS2_PLACEMENT_3D ( 'NONE', #143, #15131, #33369 ) ;
#32306 = CARTESIAN_POINT ( 'NONE',  ( 108.0049454219347354, 155.0000000000000000, 0.000000000000000000 ) ) ;
#32307 = CARTESIAN_POINT ( 'NONE',  ( 48.22499999726881015, 149.9369285172503510, 15.58253174999999580 ) ) ;
#32308 = CARTESIAN_POINT ( 'NONE',  ( 7.375838497908181246, 196.7627149292499666, 50.45113791807855819 ) ) ;
#32309 = CARTESIAN_POINT ( 'NONE',  ( 41.01132485994281041, 142.2402378747194405, 9.270509831248432420 ) ) ;
#32310 = CARTESIAN_POINT ( 'NONE',  ( -10.00000000000000711, 207.0476921513413515, 90.50113791807858377 ) ) ;
#32311 = CARTESIAN_POINT ( 'NONE',  ( -9.984503880673475606, 210.2968891136704315, 69.65113791807856103 ) ) ;
#32312 = CARTESIAN_POINT ( 'NONE',  ( -12.00000000000000711, 206.9523078486584780, 35.49886208192143044 ) ) ;
#32313 = CARTESIAN_POINT ( 'NONE',  ( -3.135527875058982783, 216.4958274776886924, 42.09886208192143897 ) ) ;
#32314 = CARTESIAN_POINT ( 'NONE',  ( 83.09999999453761177, 150.2886644046228639, 14.49999999999999645 ) ) ;
#32315 = CARTESIAN_POINT ( 'NONE',  ( 9.680171189290831535, 199.9079932115568852, 77.30113791807858092 ) ) ;
#32316 = CARTESIAN_POINT ( 'NONE',  ( -4.984841277089726574, 200.2242689037092305, 96.05113791807858092 ) ) ;
#32317 = CARTESIAN_POINT ( 'NONE',  ( -3.044812012439970683, 197.4746971517856196, 58.89886208192143613 ) ) ;
#32318 = ORIENTED_EDGE ( 'NONE', *, *, #20154, .F. ) ;
#32319 = CARTESIAN_POINT ( 'NONE',  ( -12.00000000000000711, 206.9523078486584780, 65.49886208192144466 ) ) ;
#32320 = STYLED_ITEM ( 'NONE', ( #26392 ), #9595 ) ;
#32321 = ORIENTED_EDGE ( 'NONE', *, *, #19350, .T. ) ;
#32322 = CARTESIAN_POINT ( 'NONE',  ( 73.97499999726881015, 169.8198683612136222, 4.815267126137181997 ) ) ;
#32323 = CARTESIAN_POINT ( 'NONE',  ( -4.903702542908436435, 200.1653181626580249, 44.04886208192144181 ) ) ;
#32324 = EDGE_LOOP ( 'NONE', ( #21102, #29353, #10109, #26496 ) ) ;
#32325 = CARTESIAN_POINT ( 'NONE',  ( 83.97499999726882436, 169.8198683612136222, 4.815267126137181997 ) ) ;
#32326 = CARTESIAN_POINT ( 'NONE',  ( -3.500000000000001332, 2.020725942163708488, -2.587392608830344720 ) ) ;
#32327 = PRESENTATION_LAYER_ASSIGNMENT (  '', '', ( #22542 ) ) ;
#32328 = CARTESIAN_POINT ( 'NONE',  ( -7.984503880673488041, 209.6470497212046098, 48.65113791807857524 ) ) ;
#32329 = CARTESIAN_POINT ( 'NONE',  ( 125.5000000000000000, 157.1499999999996362, -106.0000000000000284 ) ) ;
#32330 = CARTESIAN_POINT ( 'NONE',  ( 6.220909254589681581, 198.5229672870052582, 34.44886208192143329 ) ) ;
#32331 = CARTESIAN_POINT ( 'NONE',  ( 71.17499999726881299, 145.8408176439707802, -12.60653300113719588 ) ) ;
#32332 = ORIENTED_EDGE ( 'NONE', *, *, #1238, .T. ) ;
#32333 = DIRECTION ( 'NONE',  ( 1.000000000000000000, 0.000000000000000000, -0.000000000000000000 ) ) ;
#32334 =( LENGTH_UNIT ( ) NAMED_UNIT ( * ) SI_UNIT ( .MILLI., .METRE. ) );
#32335 = CARTESIAN_POINT ( 'NONE',  ( 51.78867513459482552, 155.0000000000000000, 15.00000000000001243 ) ) ;
#32336 = ADVANCED_BREP_SHAPE_REPRESENTATION ( '', ( #789, #2404 ), #8406 ) ;
#32337 = CYLINDRICAL_SURFACE ( 'NONE', #32125, 4.199999999999988631 ) ;
#32338 = CARTESIAN_POINT ( 'NONE',  ( 4.903702542908435547, 213.8346818373419751, 15.54886208192143826 ) ) ;
#32339 = CARTESIAN_POINT ( 'NONE',  ( 3.135527875058820690, 216.4958274776887492, 58.40113791807857524 ) ) ;
#32340 = CARTESIAN_POINT ( 'NONE',  ( -10.00000000000000711, 207.0476921513413515, 36.50113791807857666 ) ) ;
#32341 = CARTESIAN_POINT ( 'NONE',  ( 37.81132485994280756, 159.8737954434935489, -15.00000000000008527 ) ) ;
#32342 = ITEM_DEFINED_TRANSFORMATION ( 'NONE', 'NONE', #14275,  #2404 ) ;
#32343 = MECHANICAL_DESIGN_GEOMETRIC_PRESENTATION_REPRESENTATION (  '', ( #17666 ), #4614 ) ;
#32344 = CARTESIAN_POINT ( 'NONE',  ( 6.500168698208244500, 202.3363017425938324, 100.2988620819214276 ) ) ;
#32345 = CARTESIAN_POINT ( 'NONE',  ( 45.72499999726881015, 169.8198683612136222, 4.815267126137181997 ) ) ;
#32346 = DIRECTION ( 'NONE',  ( 1.000000000000000000, 0.000000000000000000, -0.000000000000000000 ) ) ;
#32347 = CARTESIAN_POINT ( 'NONE',  ( 33.12499999726880873, 155.0000000000000000, -15.58253175000000823 ) ) ;
#32348 = CARTESIAN_POINT ( 'NONE',  ( 9.736236675707914401, 214.0148392665762458, 16.70113791807856529 ) ) ;
#32349 = CARTESIAN_POINT ( 'NONE',  ( -63.49999999999884892, 215.0000000000003979, 0.000000000000000000 ) ) ;
#32350 = CARTESIAN_POINT ( 'NONE',  ( -0.05014649552810635652, 196.4853777576173002, 65.75113791807856956 ) ) ;
#32351 = CARTESIAN_POINT ( 'NONE',  ( 3.135527875058820690, 216.4958274776887492, 37.40113791807857524 ) ) ;
#32352 = CARTESIAN_POINT ( 'NONE',  ( -65.20000000000000284, 0.9203920079924583497, -19.30000000000004690 ) ) ;
#32353 = DIRECTION ( 'NONE',  ( 1.000000000000000000, -0.000000000000000000, -0.000000000000000000 ) ) ;
#32354 = CARTESIAN_POINT ( 'NONE',  ( -7.375838497908014268, 196.7627149292498530, 8.048862081921434708 ) ) ;
#32355 = CARTESIAN_POINT ( 'NONE',  ( 10.00000000000000711, 207.0476921513415220, 6.998862081921434886 ) ) ;
#32356 = CARTESIAN_POINT ( 'NONE',  ( 67.99999999453761745, 155.0000000000000000, -14.50000000000000711 ) ) ;
#32357 = ORIENTED_EDGE ( 'NONE', *, *, #31581, .T. ) ;
#32358 = CARTESIAN_POINT ( 'NONE',  ( 12.01549611932652972, 210.8513442034534933, 52.85113791807857098 ) ) ;
#32359 = CARTESIAN_POINT ( 'NONE',  ( 2.426778023690261410, 199.3768101843759837, 71.60113791807857808 ) ) ;
#32360 = CARTESIAN_POINT ( 'NONE',  ( 74.38867513459481984, 140.7341522555726669, -4.635254915624220651 ) ) ;
#32361 = CARTESIAN_POINT ( 'NONE',  ( -3.044812012439970683, 197.4746971517856196, 31.89886208192143613 ) ) ;
#32362 = ORIENTED_EDGE ( 'NONE', *, *, #29596, .F. ) ;
#32363 = CARTESIAN_POINT ( 'NONE',  ( -6.139770520408369237, 215.5359834540460042, 75.95113791807857240 ) ) ;
#32364 = ORIENTED_EDGE ( 'NONE', *, *, #3864, .T. ) ;
#32365 = EDGE_CURVE ( 'NONE', #30922, #615, #3070, .T. ) ;
#32366 = CARTESIAN_POINT ( 'NONE',  ( 58.48867513459484258, 142.2402378747194405, -9.270509831248439525 ) ) ;
#32367 = CARTESIAN_POINT ( 'NONE',  ( -4.424031367838992423, -4.951337798339370266, -6.056431503346042078 ) ) ;
#32368 = VERTEX_POINT ( 'NONE', #8683 ) ;
#32369 = CARTESIAN_POINT ( 'NONE',  ( -6.500168698208129925, 202.3363017425936050, 18.20113791807856529 ) ) ;
#32370 = CARTESIAN_POINT ( 'NONE',  ( -60.66914996032592455, 194.9805833264304908, -1.253524243223063994 ) ) ;
#32371 = CARTESIAN_POINT ( 'NONE',  ( -9.984503880673420539, 203.7031108863293980, 8.348862081921435419 ) ) ;
#32372 = CARTESIAN_POINT ( 'NONE',  ( 52.37499999726881583, 155.0000000000000000, 15.58253174999999402 ) ) ;
#32373 = ORIENTED_EDGE ( 'NONE', *, *, #13038, .F. ) ;
#32374 = CARTESIAN_POINT ( 'NONE',  ( 55.72499999726881015, 169.8198683612136222, 4.815267126137181997 ) ) ;
#32375 = CARTESIAN_POINT ( 'NONE',  ( 4.984841277089725686, 213.7757310962907411, 49.55113791807858092 ) ) ;
#32376 = FACE_OUTER_BOUND ( 'NONE', #10487, .T. ) ;
#32377 = SURFACE_STYLE_FILL_AREA ( #3769 ) ;
#32378 = DIRECTION ( 'NONE',  ( 0.000000000000000000, 0.000000000000000000, -1.000000000000000000 ) ) ;
#32379 = CARTESIAN_POINT ( 'NONE',  ( 10.01549611932659545, 203.7984951890123853, 94.14886208192143613 ) ) ;
#32380 = CARTESIAN_POINT ( 'NONE',  ( 60.47499999726881725, 149.9369285172503510, 15.58253174999999580 ) ) ;
#32381 = CARTESIAN_POINT ( 'NONE',  ( 8.118202686958039038, 212.8392687619912635, 28.70113791807856884 ) ) ;
#32382 = CARTESIAN_POINT ( 'NONE',  ( -64.50000000000000000, 0.000000000000000000, 20.00000000000000000 ) ) ;
#32383 = CARTESIAN_POINT ( 'NONE',  ( -12.00000000000000711, 206.9523078486584780, 83.49886208192144466 ) ) ;
#32384 = CARTESIAN_POINT ( 'NONE',  ( 79.69999999999998863, 146.4771138417591203, 11.73074641843673227 ) ) ;
#32385 = CARTESIAN_POINT ( 'NONE',  ( 40.28867513459482552, 139.2280666364260071, -4.041636747397287284E-15 ) ) ;
#32386 = CARTESIAN_POINT ( 'NONE',  ( 77.50000000000000000, 155.0000000000000000, -15.50000000000001776 ) ) ;
#32387 = CARTESIAN_POINT ( 'NONE',  ( 10.01549611932653860, 210.2015048109876716, 97.85113791807857808 ) ) ;
#32388 = CYLINDRICAL_SURFACE ( 'NONE', #17278, 15.00000000000001776 ) ;
#32389 = CARTESIAN_POINT ( 'NONE',  ( 43.47499999726881015, 160.0630714827496206, -15.58253175000000823 ) ) ;
#32390 = CARTESIAN_POINT ( 'NONE',  ( -0.05014649552810635652, 196.4853777576173002, 32.75113791807856956 ) ) ;
#32391 = CARTESIAN_POINT ( 'NONE',  ( 76.72499999726881015, 140.1801316387863778, -4.815267126137194431 ) ) ;
#32392 = ORIENTED_EDGE ( 'NONE', *, *, #32214, .T. ) ;
#32393 = FACE_OUTER_BOUND ( 'NONE', #1650, .T. ) ;
#32394 = DIRECTION ( 'NONE',  ( -1.000000000000000000, 0.000000000000000000, 0.000000000000000000 ) ) ;
#32395 = CARTESIAN_POINT ( 'NONE',  ( 45.99999999453763166, 155.0000000000000000, -14.50000000000000711 ) ) ;
#32396 = CARTESIAN_POINT ( 'NONE',  ( -7.456977232089304408, 196.8216656703010301, 18.05113791807856316 ) ) ;
#32397 = CARTESIAN_POINT ( 'NONE',  ( -10.79277039317867271, 207.6632728202857550, 102.8962892815882668 ) ) ;
#32398 = DIRECTION ( 'NONE',  ( -0.9945218953682687379, 0.000000000000000000, 0.1045284632676965614 ) ) ;
#32399 = ORIENTED_EDGE ( 'NONE', *, *, #28744, .F. ) ;
#32400 = CARTESIAN_POINT ( 'NONE',  ( 12.01549611932659367, 203.1486557965466773, 43.14886208192143613 ) ) ;
#32401 = CARTESIAN_POINT ( 'NONE',  ( 8.062137200540920645, 201.0835637161417822, 5.301137918078566713 ) ) ;
#32402 = CARTESIAN_POINT ( 'NONE',  ( 10.00000000000000711, 206.9523078486586201, 56.00113791807856956 ) ) ;
#32403 = CARTESIAN_POINT ( 'NONE',  ( -8.015496119326597224, 209.5516654185217362, 11.64886208192143613 ) ) ;
#32404 = EDGE_CURVE ( 'NONE', #1044, #3872, #26910, .T. ) ;
#32405 = CARTESIAN_POINT ( 'NONE',  ( 99.30625411593993590, 155.0000000000000000, 12.00000000000001066 ) ) ;
#32406 = EDGE_LOOP ( 'NONE', ( #4294, #20939, #31942, #19639 ) ) ;
#32407 = CARTESIAN_POINT ( 'NONE',  ( -8.015496119326597224, 209.5516654185217362, 95.64886208192143613 ) ) ;
#32408 = DIRECTION ( 'NONE',  ( 1.000000000000000000, 0.000000000000000000, 0.000000000000000000 ) ) ;
#32409 = CARTESIAN_POINT ( 'NONE',  ( -4.903702542908602524, 213.8346818373418898, 36.95113791807857950 ) ) ;
#32410 = DIRECTION ( 'NONE',  ( 0.000000000000000000, 0.7071067811865434649, -0.7071067811865515695 ) ) ;
#32411 = ORIENTED_EDGE ( 'NONE', *, *, #15353, .T. ) ;
#32412 = CARTESIAN_POINT ( 'NONE',  ( 38.42499999726879878, 141.7447067706911810, 9.630534252274376428 ) ) ;
#32413 = CARTESIAN_POINT ( 'NONE',  ( -0.3755270751584372513, 206.7692714347155629, 108.3323677711371573 ) ) ;
#32414 = EDGE_CURVE ( 'NONE', #24055, #27878, #18583, .T. ) ;
#32415 = SHAPE_REPRESENTATION ( 'air chamber shell front', ( #2404 ), #8406 ) ;
#32416 = CARTESIAN_POINT ( 'NONE',  ( 3.135527875058981895, 197.5041725223112792, 64.59886208192143897 ) ) ;
#32417 = CARTESIAN_POINT ( 'NONE',  ( 38.97499999726881015, 140.1801316387863778, -4.815267126137194431 ) ) ;
#32418 = DIRECTION ( 'NONE',  ( 5.170793409489829447E-18, -0.9988620819214357738, 0.04769215134144141888 ) ) ;
#32419 = CARTESIAN_POINT ( 'NONE',  ( 6.500168698208129925, 211.6636982574063381, 94.70113791807858661 ) ) ;
#32420 = CARTESIAN_POINT ( 'NONE',  ( 60.10000000000000142, 141.2096805137202580, -4.480746418436742040 ) ) ;
#32421 = DIRECTION ( 'NONE',  ( -1.000000000000000000, 0.000000000000000000, -0.000000000000000000 ) ) ;
#32422 = CARTESIAN_POINT ( 'NONE',  ( -0.05014649552828365914, 215.4116977939061144, 78.24886208192144466 ) ) ;
#32423 = CARTESIAN_POINT ( 'NONE',  ( 95.70416941062676131, 155.0000000000000000, 0.000000000000000000 ) ) ;
#32424 = DIRECTION ( 'NONE',  ( -1.000000000000000000, -0.000000000000000000, -0.000000000000000000 ) ) ;
#32425 = EDGE_CURVE ( 'NONE', #4684, #18787, #11586, .T. ) ;
#32426 = CARTESIAN_POINT ( 'NONE',  ( 59.82499999726879736, 168.2552932293087906, 9.630534252274372875 ) ) ;
#32428 = EDGE_LOOP ( 'NONE', ( #22615, #26421, #12337, #15016 ) ) ;
#32427 = CARTESIAN_POINT ( 'NONE',  ( -9.984503880673475606, 210.2968891136704315, 21.65113791807856103 ) ) ;
#32429 = CYLINDRICAL_SURFACE ( 'NONE', #16264, 7.500000000000015099 ) ;
#32430 = CARTESIAN_POINT ( 'NONE',  ( 83.17499999726882720, 145.8408176439707802, -12.60653300113719588 ) ) ;
#32431 = CARTESIAN_POINT ( 'NONE',  ( 7.375838497908181246, 196.7627149292499666, 86.45113791807858661 ) ) ;
#32432 = EDGE_CURVE ( 'NONE', #32263, #19301, #18601, .T. ) ;
#32433 = DIRECTION ( 'NONE',  ( -1.000000000000000000, -0.000000000000000000, -0.000000000000000000 ) ) ;
#32434 = CYLINDRICAL_SURFACE ( 'NONE', #31408, 40.00000000000000711 ) ;
#32435 = CIRCLE ( 'NONE', #6886, 3.500000000000000444 ) ;
#32436 = ORIENTED_EDGE ( 'NONE', *, *, #30545, .T. ) ;
#32437 = CARTESIAN_POINT ( 'NONE',  ( -11.98450388067341876, 203.0532714938636047, 71.34886208192142476 ) ) ;
#32438 = CARTESIAN_POINT ( 'NONE',  ( -8.062137200540822946, 201.0835637161416400, 77.19886208192143329 ) ) ;
#32439 = CARTESIAN_POINT ( 'NONE',  ( 12.00000000000000711, 207.0476921513415220, 9.998862081921435774 ) ) ;
#32440 = CARTESIAN_POINT ( 'NONE',  ( 0.000000000000000000, 0.000000000000000000, -18.00000000000000000 ) ) ;
#32441 = CARTESIAN_POINT ( 'NONE',  ( 9.984503880673470277, 203.7031108863295401, 23.15113791807856813 ) ) ;
#32442 = CARTESIAN_POINT ( 'NONE',  ( -3.044812012439970683, 197.4746971517856196, 91.89886208192143613 ) ) ;
#32444 = ORIENTED_EDGE ( 'NONE', *, *, #10368, .T. ) ;
#32443 = AXIS2_PLACEMENT_3D ( 'NONE', #11726, #5490, #6613 ) ;
#32445 = CARTESIAN_POINT ( 'NONE',  ( 63.01132485994281751, 142.2402378747194405, 9.270509831248432420 ) ) ;
#32446 = ORIENTED_EDGE ( 'NONE', *, *, #15827, .T. ) ;
#32447 = LINE ( 'NONE', #32620, #22147 ) ;
#32448 = CARTESIAN_POINT ( 'NONE',  ( 4.903702542908435547, 213.8346818373419751, 75.54886208192142760 ) ) ;
#32449 = ORIENTED_EDGE ( 'NONE', *, *, #367, .T. ) ;
#32450 = CARTESIAN_POINT ( 'NONE',  ( 82.62499999726881583, 138.6155565068815747, -3.929120461958505118E-15 ) ) ;
#32451 = EDGE_LOOP ( 'NONE', ( #6217, #21387, #24665, #4930 ) ) ;
#32452 = DIRECTION ( 'NONE',  ( 0.000000000000000000, 0.000000000000000000, 1.000000000000000000 ) ) ;
#32453 = CARTESIAN_POINT ( 'NONE',  ( 78.12499999726883004, 155.0000000000000000, 15.58253174999999402 ) ) ;
#32454 = CARTESIAN_POINT ( 'NONE',  ( -63.50000000000001421, 210.0000000000000000, 0.000000000000000000 ) ) ;
#32455 = CARTESIAN_POINT ( 'NONE',  ( 8.015496119326531499, 209.5516654185219636, 67.85113791807857808 ) ) ;
#32456 = EDGE_CURVE ( 'NONE', #23779, #82, #1778, .T. ) ;
#32457 = LINE ( 'NONE', #6911, #15669 ) ;
#32458 = AXIS2_PLACEMENT_3D ( 'NONE', #26886, #29277, #3715 ) ;
#32459 = SHAPE_REPRESENTATION_RELATIONSHIP ( 'NONE' , 'NONE' ,  #30243, #20158 ) ;
#32460 = CARTESIAN_POINT ( 'NONE',  ( 33.70000000000000284, 146.4771138417591203, 11.73074641843673227 ) ) ;
#32461 = CARTESIAN_POINT ( 'NONE',  ( -0.05014649552828365914, 215.4116977939061144, 48.24886208192144466 ) ) ;
#32462 = ADVANCED_FACE ( 'NONE', ( #14634 ), #9692, .T. ) ;
#32463 = CARTESIAN_POINT ( 'NONE',  ( 10.00000000000000711, 206.9523078486586201, 77.00113791807858377 ) ) ;
#32464 = AXIS2_PLACEMENT_3D ( 'NONE', #27233, #9179, #19569 ) ;
#32465 = DIRECTION ( 'NONE',  ( 1.000000000000000000, 0.000000000000000000, 0.000000000000000000 ) ) ;
#32466 = DIRECTION ( 'NONE',  ( 0.000000000000000000, 0.000000000000000000, 1.000000000000000000 ) ) ;
#32467 = DIRECTION ( 'NONE',  ( 0.000000000000000000, 0.000000000000000000, -1.000000000000000000 ) ) ;
#32468 = CARTESIAN_POINT ( 'NONE',  ( 53.02499999726881441, 149.9369285172503510, -15.58253175000000823 ) ) ;
#32469 = CARTESIAN_POINT ( 'NONE',  ( 9.736236675707914401, 214.0148392665762458, 55.70113791807856529 ) ) ;
#32470 = CARTESIAN_POINT ( 'NONE',  ( -120.8017490774095535, -3.226370279868306046, 35.00001200000000523 ) ) ;
#32471 = EDGE_CURVE ( 'NONE', #11308, #26980, #24522, .T. ) ;
#32472 = CARTESIAN_POINT ( 'NONE',  ( 0.05014649552810505201, 217.5146222423826714, 100.2511379180785838 ) ) ;
#32473 = CARTESIAN_POINT ( 'NONE',  ( -6.139770520408368348, 215.5359834540460042, 63.95113791807857950 ) ) ;
#32474 = CARTESIAN_POINT ( 'NONE',  ( 3.753561863808876797, 195.6020594897209719, 31.59886208192143187 ) ) ;
#32475 = CARTESIAN_POINT ( 'NONE',  ( -10.01549611932659545, 210.2015048109875011, 50.64886208192143613 ) ) ;
#32476 = CARTESIAN_POINT ( 'NONE',  ( 86.49999999453761745, 170.2462022514548323, -7.872454543227099337E-15 ) ) ;
#32477 = CARTESIAN_POINT ( 'NONE',  ( -7.375838497908182134, 217.2372850707499765, 72.95113791807857240 ) ) ;
#32478 = AXIS2_PLACEMENT_3D ( 'NONE', #14996, #19606, #33227 ) ;
#32479 = CARTESIAN_POINT ( 'NONE',  ( -7.984503880673488041, 209.6470497212046098, 99.65113791807858945 ) ) ;
#32480 = CARTESIAN_POINT ( 'NONE',  ( -8.118202686958138514, 212.8392687619910930, 56.79886208192143471 ) ) ;
#32481 = AXIS2_PLACEMENT_3D ( 'NONE', #15945, #2686, #31298 ) ;
#32482 = FACE_OUTER_BOUND ( 'NONE', #19321, .T. ) ;
#32483 = ORIENTED_EDGE ( 'NONE', *, *, #29099, .F. ) ;
#32484 = CARTESIAN_POINT ( 'NONE',  ( -9.680171189290716072, 199.9079932115567146, 65.19886208192143329 ) ) ;
#32485 = ORIENTED_EDGE ( 'NONE', *, *, #31448, .F. ) ;
#32486 = CARTESIAN_POINT ( 'NONE',  ( 68.67499999726879878, 141.7447067706911810, 9.630534252274376428 ) ) ;
#32487 = CARTESIAN_POINT ( 'NONE',  ( 6.444103211790928043, 211.7408657792734061, 39.69886208192144750 ) ) ;
#32488 = ORIENTED_EDGE ( 'NONE', *, *, #6858, .T. ) ;
#32489 = AXIS2_PLACEMENT_3D ( 'NONE', #6876, #33280, #19991 ) ;
#32490 = CARTESIAN_POINT ( 'NONE',  ( 82.77499999726880731, 140.1801316387863778, 4.815267126137185549 ) ) ;
#32491 = CARTESIAN_POINT ( 'NONE',  ( -67.50000000000000000, 0.000000000000000000, 17.00000000000001421 ) ) ;
#32492 = FACE_OUTER_BOUND ( 'NONE', #23063, .T. ) ;
#32493 = CARTESIAN_POINT ( 'NONE',  ( -2.426778023690262742, 214.6231898156240163, 58.10113791807857808 ) ) ;
#32494 = ADVANCED_FACE ( 'NONE', ( #20084 ), #31718, .F. ) ;
#32495 = CARTESIAN_POINT ( 'NONE',  ( 6.220909254589681581, 198.5229672870052582, 46.44886208192141908 ) ) ;
#32496 = CARTESIAN_POINT ( 'NONE',  ( 71.97499999726881015, 169.8198683612136222, 4.815267126137181997 ) ) ;
#32497 = ORIENTED_EDGE ( 'NONE', *, *, #12482, .T. ) ;
#32498 = DIRECTION ( 'NONE',  ( 0.000000000000000000, 0.000000000000000000, -1.000000000000000000 ) ) ;
#32499 =( LENGTH_UNIT ( ) NAMED_UNIT ( * ) SI_UNIT ( .MILLI., .METRE. ) );
#32500 = DIRECTION ( 'NONE',  ( -0.000000000000000000, -0.000000000000000000, 1.000000000000000000 ) ) ;
#32501 = FACE_OUTER_BOUND ( 'NONE', #2958, .T. ) ;
#32502 = CARTESIAN_POINT ( 'NONE',  ( 0.05014649552828262524, 198.5883022060938572, 16.74886208192143755 ) ) ;
#32503 = CARTESIAN_POINT ( 'NONE',  ( 3.135527875058820690, 216.4958274776887492, 61.40113791807857524 ) ) ;
#32504 = EDGE_CURVE ( 'NONE', #8132, #3157, #7141, .T. ) ;
#32505 = CARTESIAN_POINT ( 'NONE',  ( 3.135527875058820690, 216.4958274776887492, 46.40113791807857524 ) ) ;
#32506 = CARTESIAN_POINT ( 'NONE',  ( 88.37499999726880162, 155.0000000000000000, 15.58253174999999402 ) ) ;
#32507 = VECTOR ( 'NONE', #17796, 1000.000000000000000 ) ;
#32508 =( GEOMETRIC_REPRESENTATION_CONTEXT ( 3 ) GLOBAL_UNCERTAINTY_ASSIGNED_CONTEXT ( ( #18520 ) ) GLOBAL_UNIT_ASSIGNED_CONTEXT ( ( #23960, #16449, #31472 ) ) REPRESENTATION_CONTEXT ( 'NONE', 'WORKASPACE' ) );
#32509 = CARTESIAN_POINT ( 'NONE',  ( -0.05014649552810635652, 196.4853777576173002, 14.75113791807856245 ) ) ;
#32510 = CARTESIAN_POINT ( 'NONE',  ( 8.000000000000008882, 206.9523078486586485, -0.9988620819214343305 ) ) ;
#32511 = CARTESIAN_POINT ( 'NONE',  ( 45.62499999726880162, 171.3844434931184253, -7.942151717890132712E-15 ) ) ;
#32512 = DIRECTION ( 'NONE',  ( 0.000000000000000000, 0.000000000000000000, 1.000000000000000000 ) ) ;
#32513 = CARTESIAN_POINT ( 'NONE',  ( 0.05014649552807549926, 219.6175466908591716, 22.25113791807856956 ) ) ;
#32514 = DIRECTION ( 'NONE',  ( 1.000000000000000000, 0.000000000000000000, 0.000000000000000000 ) ) ;
#32515 = CARTESIAN_POINT ( 'NONE',  ( 8.062137200540920645, 201.0835637161417822, 77.30113791807858092 ) ) ;
#32516 = CARTESIAN_POINT ( 'NONE',  ( 6.139770520408367460, 198.4640165459539389, 38.45113791807856529 ) ) ;
#32517 = CARTESIAN_POINT ( 'NONE',  ( 76.68867513459481700, 150.1262045565067922, -15.00000000000028599 ) ) ;
#32518 = DIRECTION ( 'NONE',  ( 1.000000000000000000, 0.000000000000000000, 0.000000000000000000 ) ) ;
#32519 = CARTESIAN_POINT ( 'NONE',  ( -7.375838497908014268, 196.7627149292498530, 5.048862081921433820 ) ) ;
#32520 = CARTESIAN_POINT ( 'NONE',  ( 10.00000000000000711, 207.0476921513415220, 21.99886208192143755 ) ) ;
#32521 = CARTESIAN_POINT ( 'NONE',  ( 68.89999999453763735, 159.7113355953771077, 14.49999999999999289 ) ) ;
#32522 = ORIENTED_EDGE ( 'NONE', *, *, #20142, .F. ) ;
#32523 = CARTESIAN_POINT ( 'NONE',  ( -3.753561863808691168, 195.6020594897209435, 47.90113791807857524 ) ) ;
#32524 = CARTESIAN_POINT ( 'NONE',  ( 2.517493886308900919, 214.5937144450984420, 73.40113791807856103 ) ) ;
#32525 = CARTESIAN_POINT ( 'NONE',  ( 9.984503880673420539, 210.2968891136705167, 30.84886208192142831 ) ) ;
#32526 = ORIENTED_EDGE ( 'NONE', *, *, #25637, .T. ) ;
#32527 = CARTESIAN_POINT ( 'NONE',  ( 10.01549611932653860, 210.2015048109876716, 91.85113791807853545 ) ) ;
#32528 = AXIS2_PLACEMENT_3D ( 'NONE', #1850, #32512, #6968 ) ;
#32529 = ORIENTED_EDGE ( 'NONE', *, *, #4354, .T. ) ;
#32530 = AXIS2_PLACEMENT_3D ( 'NONE', #9160, #6604, #16987 ) ;
#32531 = CARTESIAN_POINT ( 'NONE',  ( 87.49999999999995737, 162.7917165882215329, -13.53300274343441956 ) ) ;
#32532 = LINE ( 'NONE', #29990, #17632 ) ;
#32533 = ORIENTED_EDGE ( 'NONE', *, *, #32432, .T. ) ;
#32534 = CARTESIAN_POINT ( 'NONE',  ( -6.500168698208129925, 202.3363017425936050, 24.20113791807856529 ) ) ;
#32535 = DIRECTION ( 'NONE',  ( 0.8660254037844382635, 0.5000000000000004441, 0.000000000000000000 ) ) ;
#32536 = CARTESIAN_POINT ( 'NONE',  ( 10.01549611932659545, 203.7984951890123853, 7.148862081921433465 ) ) ;
#32537 = CARTESIAN_POINT ( 'NONE',  ( 47.37499999726880873, 155.0000000000000000, -15.58253175000000823 ) ) ;
#32539 = ORIENTED_EDGE ( 'NONE', *, *, #395, .T. ) ;
#32538 = AXIS2_PLACEMENT_3D ( 'NONE', #4190, #30090, #19863 ) ;
#32540 = CARTESIAN_POINT ( 'NONE',  ( 6.500168698208129925, 211.6636982574063381, 52.70113791807857240 ) ) ;
#32541 = CARTESIAN_POINT ( 'NONE',  ( 32.50000000000000000, 155.0000000000000000, -15.00000000000002487 ) ) ;
#32542 =( NAMED_UNIT ( * ) PLANE_ANGLE_UNIT ( ) SI_UNIT ( $, .RADIAN. ) );
#32543 = DIRECTION ( 'NONE',  ( 1.000000000000000000, -0.000000000000000000, -0.000000000000000000 ) ) ;
#32544 = CARTESIAN_POINT ( 'NONE',  ( -6.220909254589682469, 215.4770327129946850, 86.94886208192141908 ) ) ;
#32545 = CARTESIAN_POINT ( 'NONE',  ( 62.37499999726880873, 155.0000000000000000, 15.58253174999999402 ) ) ;
#32546 = CARTESIAN_POINT ( 'NONE',  ( 0.05014649552810505201, 217.5146222423826714, 28.25113791807855890 ) ) ;
#32547 = CARTESIAN_POINT ( 'NONE',  ( 70.08867513459482268, 142.2402378747194405, 9.270509831248432420 ) ) ;
#32548 = CARTESIAN_POINT ( 'NONE',  ( -0.05014649552828442242, 219.6175466908591716, 78.24886208192144466 ) ) ;
#32549 = CARTESIAN_POINT ( 'NONE',  ( -60.00000000000000000, -7.347880794884118356E-15, 45.00000000000000711 ) ) ;
#32550 = CARTESIAN_POINT ( 'NONE',  ( 81.79999999999999716, 142.6655632788954620, 8.961492836873471646 ) ) ;
#32551 =( LENGTH_UNIT ( ) NAMED_UNIT ( * ) SI_UNIT ( .MILLI., .METRE. ) );
#32552 = CARTESIAN_POINT ( 'NONE',  ( -3.499999999999996891, 4.286263797015732651E-16, 2.066666666666666430 ) ) ;
#32553 = CARTESIAN_POINT ( 'NONE',  ( -10.00000000000000711, 207.0476921513413515, 90.50113791807858377 ) ) ;
#32554 = CIRCLE ( 'NONE', #26056, 11.99999999999998224 ) ;
#32555 = DIRECTION ( 'NONE',  ( 0.1045284632676479336, 0.000000000000000000, -0.9945218953682739560 ) ) ;
#32556 = CARTESIAN_POINT ( 'NONE',  ( 42.87499999726881583, 138.6155565068815463, -3.929120461958505118E-15 ) ) ;
#32557 = CARTESIAN_POINT ( 'NONE',  ( -6.220909254589537696, 198.5229672870051161, 39.05113791807856671 ) ) ;
#32558 = ADVANCED_FACE ( 'NONE', ( #17526 ), #20293, .T. ) ;
#32559 = VECTOR ( 'NONE', #10232, 1000.000000000000000 ) ;
#32560 = CARTESIAN_POINT ( 'NONE',  ( 85.52499999726880731, 169.8198683612136222, -4.815267126137197984 ) ) ;
#32561 = VECTOR ( 'NONE', #20110, 1000.000000000000000 ) ;
#32562 = CARTESIAN_POINT ( 'NONE',  ( -125.0000000000000000, 0.000000000000000000, -35.00000000000000000 ) ) ;
#32563 = DIRECTION ( 'NONE',  ( -1.000000000000000000, -0.000000000000000000, -0.000000000000000000 ) ) ;
#32564 = CARTESIAN_POINT ( 'NONE',  ( 46.79999999453762882, 163.5228861582408797, 11.73074641843673049 ) ) ;
#32565 = ORIENTED_EDGE ( 'NONE', *, *, #25125, .F. ) ;
#32566 = CARTESIAN_POINT ( 'NONE',  ( -9.736236675707914401, 199.9851607334237542, 15.20113791807857062 ) ) ;
#32567 = CARTESIAN_POINT ( 'NONE',  ( 60.81132485994280756, 150.1262045565063659, 14.99999999999997158 ) ) ;
#32568 = VECTOR ( 'NONE', #30353, 1000.000000000000000 ) ;
#32569 = CARTESIAN_POINT ( 'NONE',  ( 66.01132485994280330, 167.7597621252805880, -9.270509831248443078 ) ) ;
#32570 = EDGE_LOOP ( 'NONE', ( #25194, #16481 ) ) ;
#32571 = CARTESIAN_POINT ( 'NONE',  ( -3.753561863808878130, 218.3979405102790281, 39.09886208192143187 ) ) ;
#32572 = CARTESIAN_POINT ( 'NONE',  ( 3.044812012440130555, 197.4746971517856764, -0.3988620819214342972 ) ) ;
#32573 = CARTESIAN_POINT ( 'NONE',  ( 3.044812012440130555, 197.4746971517856764, 59.60113791807857808 ) ) ;
#32574 = CARTESIAN_POINT ( 'NONE',  ( 2.517493886309087436, 199.4062855549015865, 10.59886208192143542 ) ) ;
#32575 = UNCERTAINTY_MEASURE_WITH_UNIT (LENGTH_MEASURE( 1.000000000000000082E-05 ), #1970, 'distance_accuracy_value', 'NONE');
#32576 = CARTESIAN_POINT ( 'NONE',  ( 51.21132485994281325, 139.2280666364260071, -4.041636747397287284E-15 ) ) ;
#32577 = ORIENTED_EDGE ( 'NONE', *, *, #26948, .T. ) ;
#32578 = CARTESIAN_POINT ( 'NONE',  ( 8.000000000000008882, 207.0476921513415220, 96.99886208192143044 ) ) ;
#32579 = AXIS2_PLACEMENT_3D ( 'NONE', #9953, #25617, #2283 ) ;
#32580 = CARTESIAN_POINT ( 'NONE',  ( 32.50000000000000000, 155.0000000000000000, -13.00000000000002487 ) ) ;
#32581 = CARTESIAN_POINT ( 'NONE',  ( 8.000000000000008882, 206.9523078486586485, 38.00113791807857666 ) ) ;
#32582 = CYLINDRICAL_SURFACE ( 'NONE', #3182, 2.149999999999996803 ) ;
#32583 = ORIENTED_EDGE ( 'NONE', *, *, #4354, .F. ) ;
#32584 = CARTESIAN_POINT ( 'NONE',  ( 36.82499999726881157, 141.7447067706911810, -9.630534252274385310 ) ) ;
#32585 = CARTESIAN_POINT ( 'NONE',  ( 8.000000000000000000, 0.000000000000000000, 0.000000000000000000 ) ) ;
#32586 = CARTESIAN_POINT ( 'NONE',  ( -2.654873707089192509E-16, -7.693917458112650820, -6.460793508093416904 ) ) ;
#32587 = AXIS2_PLACEMENT_3D ( 'NONE', #4267, #22663, #30503 ) ;
#32588 = CARTESIAN_POINT ( 'NONE',  ( 61.72499999726881015, 169.8198683612136222, 4.815267126137181997 ) ) ;
#32589 = CARTESIAN_POINT ( 'NONE',  ( 10.00000000000000711, 207.0476921513415220, 63.99886208192143044 ) ) ;
#32590 = CARTESIAN_POINT ( 'NONE',  ( 39.87499999726880162, 171.3844434931184253, -7.942151717890132712E-15 ) ) ;
#32591 = CYLINDRICAL_SURFACE ( 'NONE', #9206, 17.00000000000000355 ) ;
#32592 = CARTESIAN_POINT ( 'NONE',  ( -0.05014649552810635652, 196.4853777576173002, 5.751137918078563338 ) ) ;
#32593 = VECTOR ( 'NONE', #17258, 999.9999999999998863 ) ;
#32594 = CARTESIAN_POINT ( 'NONE',  ( 63.00000000000000000, 170.2462022514548323, -7.872454543227099337E-15 ) ) ;
#32595 = DIRECTION ( 'NONE',  ( -0.000000000000000000, -0.000000000000000000, 1.000000000000000000 ) ) ;
#32596 = CARTESIAN_POINT ( 'NONE',  ( -6.444103211790928043, 202.2591342207265939, 83.19886208192144750 ) ) ;
#32597 = DIRECTION ( 'NONE',  ( 0.000000000000000000, 0.000000000000000000, -1.000000000000000000 ) ) ;
#32598 = LINE ( 'NONE', #30047, #24339 ) ;
#32599 = EDGE_CURVE ( 'NONE', #25683, #20297, #8331, .T. ) ;
#32600 = CARTESIAN_POINT ( 'NONE',  ( 66.52499999726880731, 140.1801316387863778, 4.815267126137185549 ) ) ;
#32602 = ORIENTED_EDGE ( 'NONE', *, *, #33299, .F. ) ;
#32601 = CARTESIAN_POINT ( 'NONE',  ( 8.118202686958039038, 212.8392687619912635, 16.70113791807856529 ) ) ;
#32603 = DIRECTION ( 'NONE',  ( 0.000000000000000000, 0.000000000000000000, 1.000000000000000000 ) ) ;
#32604 = CARTESIAN_POINT ( 'NONE',  ( 85.77499999726880731, 169.8198683612136222, -4.815267126137197984 ) ) ;
#32605 = CARTESIAN_POINT ( 'NONE',  ( -7.375838497908182134, 217.2372850707499765, 87.95113791807857240 ) ) ;
#32606 = AXIS2_PLACEMENT_3D ( 'NONE', #7866, #22854, #28639 ) ;
#32607 = CARTESIAN_POINT ( 'NONE',  ( 6.815830331203685866, 1.228021141713631082E-13, -6.171384342982610960 ) ) ;
#32608 = EDGE_CURVE ( 'NONE', #33593, #4673, #27243, .T. ) ;
#32609 = ORIENTED_EDGE ( 'NONE', *, *, #25434, .F. ) ;
#32610 = CARTESIAN_POINT ( 'NONE',  ( -12.00000000000000711, 206.9523078486584780, 71.49886208192144466 ) ) ;
#32611 = CARTESIAN_POINT ( 'NONE',  ( 0.05014649552828275014, 196.4853777576173002, 76.74886208192143044 ) ) ;
#32612 = CARTESIAN_POINT ( 'NONE',  ( -7.456977232089471386, 217.1783343296987709, 11.94886208192143506 ) ) ;
#32613 = CARTESIAN_POINT ( 'NONE',  ( 0.000000000000000000, -4.685197434473814759, 3.903127820947815962E-15 ) ) ;
#32614 = CARTESIAN_POINT ( 'NONE',  ( -6.139770520408369237, 215.5359834540460042, 24.95113791807855819 ) ) ;
#32615 = CARTESIAN_POINT ( 'NONE',  ( 101.3062541159399075, 155.0000000000000000, -12.00000000000001066 ) ) ;
#32616 = CARTESIAN_POINT ( 'NONE',  ( -0.05014649552828403384, 217.5146222423826714, 84.24886208192143044 ) ) ;
#32617 = EDGE_CURVE ( 'NONE', #10137, #14343, #13214, .T. ) ;
#32618 = CARTESIAN_POINT ( 'NONE',  ( 79.50000000000000000, 155.0000000000000000, -6.938893903907228378E-15 ) ) ;
#32619 = ORIENTED_EDGE ( 'NONE', *, *, #13553, .T. ) ;
#32620 = CARTESIAN_POINT ( 'NONE',  ( 94.70964751525852421, 155.0000000000000000, -32.10452846326766974 ) ) ;
#32621 = CARTESIAN_POINT ( 'NONE',  ( 8.000000000000008882, 207.0476921513415220, 69.99886208192144466 ) ) ;
#32622 = SHAPE_REPRESENTATION ( 'socket head cap screw_iso_ISO 4762 M8 x 70 - 28N', ( #2404 ), #20321 ) ;
#32623 = ORIENTED_EDGE ( 'NONE', *, *, #21584, .T. ) ;
#32624 = CARTESIAN_POINT ( 'NONE',  ( 83.62499999726881583, 171.3844434931184253, -7.942151717890134290E-15 ) ) ;
#32625 = ORIENTED_EDGE ( 'NONE', *, *, #20539, .F. ) ;
#32626 = CARTESIAN_POINT ( 'NONE',  ( 69.58867513459482268, 163.8167787843871110, 12.13525491562421621 ) ) ;
#32627 = EDGE_CURVE ( 'NONE', #20140, #11974, #1856, .T. ) ;
#32628 = CARTESIAN_POINT ( 'NONE',  ( 78.52499999726880731, 140.1801316387863778, 4.815267126137185549 ) ) ;
#32629 = CARTESIAN_POINT ( 'NONE',  ( -7.500000000000001776, 2.932633423934442263, -0.4709827563909292358 ) ) ;
#32630 = CARTESIAN_POINT ( 'NONE',  ( -4.903702542908602524, 213.8346818373418898, 75.95113791807857240 ) ) ;
#32631 = DIRECTION ( 'NONE',  ( -1.000000000000000000, -0.000000000000000000, -0.000000000000000000 ) ) ;
#32632 = FILL_AREA_STYLE_COLOUR ( '', #9995 ) ;
#32633 = CARTESIAN_POINT ( 'NONE',  ( 43.99999999999999289, 139.7537977485451393, -4.138211985947621020E-15 ) ) ;
#32634 = CARTESIAN_POINT ( 'NONE',  ( -4.903702542908436435, 200.1653181626580249, 53.04886208192144181 ) ) ;
#32635 = EDGE_CURVE ( 'NONE', #27924, #25081, #9136, .T. ) ;
#32636 = DIRECTION ( 'NONE',  ( 0.000000000000000000, 0.000000000000000000, 1.000000000000000000 ) ) ;
#32637 = CARTESIAN_POINT ( 'NONE',  ( 73.51132485994280330, 146.1832212156128890, -12.13525491562423042 ) ) ;
#32638 = LINE ( 'NONE', #9301, #18608 ) ;
#32639 = CARTESIAN_POINT ( 'NONE',  ( 48.32499999726881157, 145.8408176439707802, 12.60653300113718345 ) ) ;
#32640 = CARTESIAN_POINT ( 'NONE',  ( 60.87499999726879452, 138.6155565068815463, -3.929120461958505118E-15 ) ) ;
#32641 = CARTESIAN_POINT ( 'NONE',  ( -9.736236675707914401, 199.9851607334237542, 57.20113791807856529 ) ) ;
#32642 = CARTESIAN_POINT ( 'NONE',  ( -121.7736297201316660, -4.198250922590450074, 35.00001199999999102 ) ) ;
#32643 = CARTESIAN_POINT ( 'NONE',  ( -12.00000000000000711, 207.0476921513413515, 3.501137918078566003 ) ) ;
#32644 = CARTESIAN_POINT ( 'NONE',  ( -8.118202686958039038, 201.1607312380087080, 75.20113791807857240 ) ) ;
#32645 = EDGE_CURVE ( 'NONE', #27342, #31940, #11740, .T. ) ;
#32646 = CARTESIAN_POINT ( 'NONE',  ( -12.00000000000000711, 206.9523078486584780, 41.49886208192143044 ) ) ;
#32647 = CARTESIAN_POINT ( 'NONE',  ( -10.01549611932659545, 210.2015048109875011, 47.64886208192142902 ) ) ;
#32648 = CARTESIAN_POINT ( 'NONE',  ( 86.99999999453764588, 155.0000000000000000, 14.49999999999999467 ) ) ;
#32649 = CARTESIAN_POINT ( 'NONE',  ( -7.375838497908182134, 217.2372850707499765, 90.95113791807855819 ) ) ;
#32650 = CARTESIAN_POINT ( 'NONE',  ( -8.000000000000008882, 207.0476921513413515, 99.50113791807856956 ) ) ;
#32651 = CARTESIAN_POINT ( 'NONE',  ( 0.05014649552828275708, 196.4853777576173002, 61.74886208192143755 ) ) ;
#32652 = ORIENTED_EDGE ( 'NONE', *, *, #5768, .F. ) ;
#32653 = CARTESIAN_POINT ( 'NONE',  ( -11.98450388067341876, 203.0532714938636047, 68.34886208192142476 ) ) ;
#32654 = EDGE_LOOP ( 'NONE', ( #10525, #414, #15695, #28494 ) ) ;
#32655 = CARTESIAN_POINT ( 'NONE',  ( 71.47499999726879594, 160.0630714827496206, -15.58253175000000823 ) ) ;
#32656 = CARTESIAN_POINT ( 'NONE',  ( -4.984841277089891776, 213.7757310962905990, 38.94886208192144039 ) ) ;
#32657 = ORIENTED_EDGE ( 'NONE', *, *, #26000, .F. ) ;
#32658 = EDGE_CURVE ( 'NONE', #2927, #12471, #19406, .T. ) ;
#32659 = CARTESIAN_POINT ( 'NONE',  ( 85.17499999726882720, 145.8408176439707802, -12.60653300113719588 ) ) ;
#32660 = CARTESIAN_POINT ( 'NONE',  ( 2.000000000000000000, 1.773042676681340968, -2.276824562219559311E-15 ) ) ;
#32661 = CARTESIAN_POINT ( 'NONE',  ( -6.269955739554009533, -4.268932597852945321, -6.443844059477445541 ) ) ;
#32662 = CARTESIAN_POINT ( 'NONE',  ( -6.500168698208129925, 202.3363017425936050, 60.20113791807857240 ) ) ;
#32663 = CARTESIAN_POINT ( 'NONE',  ( 99.99999999999998579, 0.000000000000000000, 0.000000000000000000 ) ) ;
#32664 = CARTESIAN_POINT ( 'NONE',  ( -8.062137200540822946, 201.0835637161416400, 41.19886208192144039 ) ) ;
#32665 = ORIENTED_EDGE ( 'NONE', *, *, #6177, .F. ) ;
#32666 = CARTESIAN_POINT ( 'NONE',  ( 115.4999999999999858, 155.0000000000000000, 112.0000000000000426 ) ) ;
#32667 = AXIS2_PLACEMENT_3D ( 'NONE', #16336, #26730, #6108 ) ;
#32668 = DIRECTION ( 'NONE',  ( 1.000000000000000000, 0.000000000000000000, 0.000000000000000000 ) ) ;
#32669 = DIRECTION ( 'NONE',  ( 0.000000000000000000, 0.000000000000000000, 1.000000000000000000 ) ) ;
#32670 = CARTESIAN_POINT ( 'NONE',  ( -8.000000000000008882, 206.9523078486584780, 23.49886208192144110 ) ) ;
#32671 = CARTESIAN_POINT ( 'NONE',  ( 3.135527875058820690, 216.4958274776887492, 64.40113791807857524 ) ) ;
#32672 = CARTESIAN_POINT ( 'NONE',  ( -0.05014649552810635652, 196.4853777576173002, 47.75113791807855534 ) ) ;
#32673 = FACE_OUTER_BOUND ( 'NONE', #20364, .T. ) ;
#32674 = CARTESIAN_POINT ( 'NONE',  ( 8.118202686958039038, 212.8392687619912635, 13.70113791807856707 ) ) ;
#32675 = CARTESIAN_POINT ( 'NONE',  ( -6.444103211790928043, 202.2591342207265939, 98.19886208192144750 ) ) ;
#32676 = CARTESIAN_POINT ( 'NONE',  ( 42.52499999726880731, 140.1801316387863778, 4.815267126137185549 ) ) ;
#32677 = CARTESIAN_POINT ( 'NONE',  ( 87.49999999999998579, 151.6435044740348417, -14.93273091701168909 ) ) ;
#32678 = CARTESIAN_POINT ( 'NONE',  ( -3.753561863808691168, 195.6020594897209435, 29.90113791807857169 ) ) ;
#32679 = DIRECTION ( 'NONE',  ( 0.000000000000000000, 0.000000000000000000, -1.000000000000000000 ) ) ;
#32680 = CARTESIAN_POINT ( 'NONE',  ( -0.05014649552810635652, 196.4853777576173002, 71.75113791807858377 ) ) ;
#32681 = CARTESIAN_POINT ( 'NONE',  ( 6.139770520408367460, 198.4640165459539389, 47.45113791807856529 ) ) ;
#32682 = CARTESIAN_POINT ( 'NONE',  ( 32.50000000000000000, 155.0000000000000000, -6.938893903907228378E-15 ) ) ;
#32683 = CARTESIAN_POINT ( 'NONE',  ( -9.736236675708031640, 214.0148392665760753, 17.79886208192143471 ) ) ;
#32684 = CARTESIAN_POINT ( 'NONE',  ( -10.01549611932659545, 210.2015048109875011, 14.64886208192143435 ) ) ;
#32685 = AXIS2_PLACEMENT_3D ( 'NONE', #25521, #7643, #28073 ) ;
#32686 = CARTESIAN_POINT ( 'NONE',  ( 63.89999999453763024, 150.2886644046228639, -14.50000000000000888 ) ) ;
#32687 = ORIENTED_EDGE ( 'NONE', *, *, #13334, .T. ) ;
#32688 = CARTESIAN_POINT ( 'NONE',  ( 3.662846001190051659, 195.5725841191953691, 59.60113791807857808 ) ) ;
#32689 = CARTESIAN_POINT ( 'NONE',  ( -8.015496119326531499, 204.4483345814780364, 69.35113791807857808 ) ) ;
#32690 = EDGE_CURVE ( 'NONE', #12765, #22989, #11915, .T. ) ;
#32691 = CARTESIAN_POINT ( 'NONE',  ( -3.044812012439970683, 197.4746971517856196, 28.89886208192143613 ) ) ;
#32692 = EDGE_CURVE ( 'NONE', #3666, #1492, #18701, .T. ) ;
#32693 = CARTESIAN_POINT ( 'NONE',  ( 76.11132485994281183, 169.2658477444273331, -4.635254915624224203 ) ) ;
#32694 = ORIENTED_EDGE ( 'NONE', *, *, #7292, .T. ) ;
#32695 = CARTESIAN_POINT ( 'NONE',  ( 8.062137200540920645, 201.0835637161417822, 86.30113791807856671 ) ) ;
#32696 = EDGE_CURVE ( 'NONE', #14731, #16034, #13793, .T. ) ;
#32697 = ORIENTED_EDGE ( 'NONE', *, *, #26515, .T. ) ;
#32698 = ADVANCED_FACE ( 'NONE', ( #10050 ), #24126, .T. ) ;
#32699 =( REPRESENTATION_RELATIONSHIP ('NONE','NONE', #25663, #16098 ) REPRESENTATION_RELATIONSHIP_WITH_TRANSFORMATION ( #7645 )SHAPE_REPRESENTATION_RELATIONSHIP( ) );
#32700 = CARTESIAN_POINT ( 'NONE',  ( 42.18867513459481700, 140.7341522555726669, 4.635254915624211769 ) ) ;
#32701 = CARTESIAN_POINT ( 'NONE',  ( -130.2500000000000000, 6.429395695523608097E-16, -35.00000000000000000 ) ) ;
#32702 = EDGE_LOOP ( 'NONE', ( #16691, #28533, #10887, #3765, #23861 ) ) ;
#32703 = CARTESIAN_POINT ( 'NONE',  ( 2.426778023690261410, 199.3768101843759837, 29.60113791807856742 ) ) ;
#32704 = FACE_OUTER_BOUND ( 'NONE', #4209, .T. ) ;
#32705 = CARTESIAN_POINT ( 'NONE',  ( -10.00000000000000711, 206.9523078486584495, 11.49886208192143577 ) ) ;
#32706 = CARTESIAN_POINT ( 'NONE',  ( 56.37499999726880873, 155.0000000000000000, 15.58253174999999402 ) ) ;
#32707 = ORIENTED_EDGE ( 'NONE', *, *, #28929, .F. ) ;
#32708 = CARTESIAN_POINT ( 'NONE',  ( 8.000000000000008882, 206.9523078486586485, 53.00113791807857666 ) ) ;
#32709 = DIRECTION ( 'NONE',  ( 1.000000000000000000, 0.000000000000000000, 0.000000000000000000 ) ) ;
#32710 = AXIS2_PLACEMENT_3D ( 'NONE', #5988, #3268, #19442 ) ;
#32711 =( LENGTH_UNIT ( ) NAMED_UNIT ( * ) SI_UNIT ( .MILLI., .METRE. ) );
#32712 = FACE_OUTER_BOUND ( 'NONE', #14994, .T. ) ;
#32713 = CARTESIAN_POINT ( 'NONE',  ( -8.062137200540822946, 201.0835637161416400, 98.19886208192143329 ) ) ;
#32714 = CARTESIAN_POINT ( 'NONE',  ( 59.97499999726881015, 169.8198683612136222, 4.815267126137181997 ) ) ;
#32715 = CARTESIAN_POINT ( 'NONE',  ( 9.984503880673470277, 203.7031108863295401, 35.15113791807856813 ) ) ;
#32716 = CYLINDRICAL_SURFACE ( 'NONE', #8860, 15.00000000000001776 ) ;
#32717 = CARTESIAN_POINT ( 'NONE',  ( -8.118202686958039038, 201.1607312380087080, 18.20113791807856884 ) ) ;
#32718 = DIRECTION ( 'NONE',  ( 0.000000000000000000, 0.000000000000000000, 1.000000000000000000 ) ) ;
#32719 = CARTESIAN_POINT ( 'NONE',  ( 77.79999999999999716, 142.6655632788954620, 8.961492836873471646 ) ) ;
#32720 = SURFACE_STYLE_FILL_AREA ( #19783 ) ;
#32721 = CYLINDRICAL_SURFACE ( 'NONE', #618, 4.200000000000001954 ) ;
#32722 = CARTESIAN_POINT ( 'NONE',  ( -3.135527875058821579, 197.5041725223112223, 101.9011379180785752 ) ) ;
#32723 = DIRECTION ( 'NONE',  ( -0.000000000000000000, -0.000000000000000000, 1.000000000000000000 ) ) ;
#32724 = CARTESIAN_POINT ( 'NONE',  ( 43.77499999726881441, 169.8198683612136222, -4.815267126137197984 ) ) ;
#32725 = CARTESIAN_POINT ( 'NONE',  ( -8.118202686958039038, 201.1607312380087080, 42.20113791807857240 ) ) ;
#32726 = CARTESIAN_POINT ( 'NONE',  ( 86.32499999726880446, 145.8408176439707802, 12.60653300113718345 ) ) ;
#32727 = CARTESIAN_POINT ( 'NONE',  ( -10.39117206796836257, 1.272551561242683764E-15, -8.499999999999998224 ) ) ;
#32728 = FACE_OUTER_BOUND ( 'NONE', #14022, .T. ) ;
#32729 = CARTESIAN_POINT ( 'NONE',  ( 48.29999999453762882, 167.3344367211045096, -8.961492836873482304 ) ) ;
#32730 =( BOUNDED_CURVE ( )  B_SPLINE_CURVE ( 2, ( #9891, #9719, #22323, #27267, #17043, #7165, #3924, #30332, #30167, #24720, #27437 ),
 .UNSPECIFIED., .F., .F. ) 
 B_SPLINE_CURVE_WITH_KNOTS ( ( 3, 2, 2, 2, 2, 3 ),
 ( 0.5892857142857140795, 0.5928571428571426383, 0.5964285714285711970, 0.5999999999999998668, 0.6035714285714284255, 0.6071428571428569843 ),
 .UNSPECIFIED. ) 
 CURVE ( )  GEOMETRIC_REPRESENTATION_ITEM ( )  RATIONAL_B_SPLINE_CURVE ( ( 1.000000000000003109, 0.9510565162951504226, 1.000000000000000000, 0.9510565162951534202, 1.000000000000000000, 0.9510565162951534202, 1.000000000000000000, 0.9510565162951534202, 1.000000000000000000, 0.9510565162951549745, 0.9999999999999984457 ) ) 
 REPRESENTATION_ITEM ( '' )  );
#32731 = ORIENTED_EDGE ( 'NONE', *, *, #22897, .F. ) ;
#32732 = CARTESIAN_POINT ( 'NONE',  ( 12.00000000000000711, 206.9523078486586485, 29.00113791807856956 ) ) ;
#32733 = DIRECTION ( 'NONE',  ( 0.000000000000000000, 0.000000000000000000, 1.000000000000000000 ) ) ;
#32734 = CARTESIAN_POINT ( 'NONE',  ( 32.50000000000000000, 155.0000000000000000, -6.938893903907228378E-15 ) ) ;
#32735 = VERTEX_POINT ( 'NONE', #18210 ) ;
#32736 = AXIS2_PLACEMENT_3D ( 'NONE', #3937, #30179, #12454 ) ;
#32737 = CARTESIAN_POINT ( 'NONE',  ( 3.753561863808876797, 195.6020594897209719, 40.59886208192143187 ) ) ;
#32738 = CARTESIAN_POINT ( 'NONE',  ( -8.062137200540920645, 212.9164362838581894, 3.801137918078565825 ) ) ;
#32739 = CARTESIAN_POINT ( 'NONE',  ( 6.220909254589536808, 215.4770327129947702, 61.55113791807858092 ) ) ;
#32740 = CARTESIAN_POINT ( 'NONE',  ( -7.984503880673422316, 204.3529502787951628, 26.34886208192143897 ) ) ;
#32741 = DIRECTION ( 'NONE',  ( -1.000000000000000000, -0.000000000000000000, -0.000000000000000000 ) ) ;
#32742 = ORIENTED_EDGE ( 'NONE', *, *, #27884, .F. ) ;
#32743 = CONICAL_SURFACE ( 'NONE', #2291, 27.50000000000000355, 1.047197551196595411 ) ;
#32744 = CARTESIAN_POINT ( 'NONE',  ( 4.903702542908601636, 200.1653181626581102, 8.451137918078563516 ) ) ;
#32745 = CYLINDRICAL_SURFACE ( 'NONE', #31362, 5.200000000000009948 ) ;
#32746 = CARTESIAN_POINT ( 'NONE',  ( 3.753561863808876797, 195.6020594897209719, 85.59886208192143897 ) ) ;
#32747 = DIRECTION ( 'NONE',  ( 0.000000000000000000, 0.000000000000000000, -1.000000000000000000 ) ) ;
#32748 = VERTEX_POINT ( 'NONE', #10214 ) ;
#32749 = CARTESIAN_POINT ( 'NONE',  ( 38.22499999726881015, 149.9369285172503510, 15.58253174999999580 ) ) ;
#32750 = CARTESIAN_POINT ( 'NONE',  ( 5.000000000000000000, -2.342598717236903383, 4.057500000000001883 ) ) ;
#32751 = CARTESIAN_POINT ( 'NONE',  ( -31.74999999999995737, 0.000000000000000000, 0.000000000000000000 ) ) ;
#32752 = CARTESIAN_POINT ( 'NONE',  ( -3.044812012439970683, 197.4746971517856196, 61.89886208192143613 ) ) ;
#32753 = CARTESIAN_POINT ( 'NONE',  ( 40.47499999726881725, 149.9369285172503510, 15.58253174999999580 ) ) ;
#32754 = CARTESIAN_POINT ( 'NONE',  ( 0.5725525826504701543, 3.710888496608923059, -0.1217565302851157799 ) ) ;
#32755 = CARTESIAN_POINT ( 'NONE',  ( -10.01549611932653860, 203.7984951890123284, 0.3511379180785655363 ) ) ;
#32756 = DIRECTION ( 'NONE',  ( 1.000000000000000000, -0.000000000000000000, -0.000000000000000000 ) ) ;
#32757 = FACE_OUTER_BOUND ( 'NONE', #1106, .T. ) ;
#32758 = CARTESIAN_POINT ( 'NONE',  ( 62.00000000000000000, 139.7537977485451393, -4.138211985947621020E-15 ) ) ;
#32759 = DIRECTION ( 'NONE',  ( -1.000000000000000000, -0.000000000000000000, -0.000000000000000000 ) ) ;
#32760 = CARTESIAN_POINT ( 'NONE',  ( -4.903702542908436435, 200.1653181626580249, 86.04886208192145602 ) ) ;
#32761 = CARTESIAN_POINT ( 'NONE',  ( 0.04606493828584144051, 9.175055303659556571, -8.057411785091790790 ) ) ;
#32762 = CARTESIAN_POINT ( 'NONE',  ( 3.500000000000004885, 1.693985822988437917, -2.681714356710791058 ) ) ;
#32763 = CARTESIAN_POINT ( 'NONE',  ( 9.680171189290716072, 214.0920067884432854, 84.69886208192144750 ) ) ;
#32764 = CARTESIAN_POINT ( 'NONE',  ( 62.92499999726880588, 145.8408176439707802, -12.60653300113719588 ) ) ;
#32766 = ORIENTED_EDGE ( 'NONE', *, *, #23140, .F. ) ;
#32765 = CARTESIAN_POINT ( 'NONE',  ( 0.05014649552810506589, 217.5146222423826714, 25.25113791807856600 ) ) ;
#32767 = LINE ( 'NONE', #17110, #2131 ) ;
#32768 = VECTOR ( 'NONE', #29328, 1000.000000000000000 ) ;
#32769 = CARTESIAN_POINT ( 'NONE',  ( 83.57499999726880446, 164.1591823560292198, -12.60653300113719766 ) ) ;
#32770 = CARTESIAN_POINT ( 'NONE',  ( 12.01549611932652972, 210.8513442034534933, 82.85113791807857808 ) ) ;
#32771 = AXIS2_PLACEMENT_3D ( 'NONE', #23615, #10845, #7783 ) ;
#32772 = DIRECTION ( 'NONE',  ( -1.000000000000000000, 0.000000000000000000, 0.000000000000000000 ) ) ;
#32773 = VERTEX_POINT ( 'NONE', #25874 ) ;
#32774 = CARTESIAN_POINT ( 'NONE',  ( 3.753561863808876797, 195.6020594897209719, 67.59886208192143897 ) ) ;
#32775 = CARTESIAN_POINT ( 'NONE',  ( 8.062137200540822946, 212.9164362838583315, 72.69886208192143329 ) ) ;
#32776 = CARTESIAN_POINT ( 'NONE',  ( -3.753561863808878130, 218.3979405102790281, 18.09886208192143187 ) ) ;
#32777 = FACE_BOUND ( 'NONE', #2628, .T. ) ;
#32778 = CARTESIAN_POINT ( 'NONE',  ( 9.984503880673470277, 203.7031108863295401, 29.15113791807856103 ) ) ;
#32779 = CARTESIAN_POINT ( 'NONE',  ( 4.000000000000000000, 0.000000000000000000, 0.000000000000000000 ) ) ;
#32780 = CARTESIAN_POINT ( 'NONE',  ( 9.984503880673420539, 210.2968891136705167, 102.8488620819214390 ) ) ;
#32781 = CIRCLE ( 'NONE', #28447, 6.500000000000000000 ) ;
#32782 = CYLINDRICAL_SURFACE ( 'NONE', #18127, 15.00000000000001776 ) ;
#32783 = VERTEX_POINT ( 'NONE', #25533 ) ;
#32784 = CARTESIAN_POINT ( 'NONE',  ( 92.60208470531341618, 155.0000000000000000, 0.000000000000000000 ) ) ;
#32785 = CARTESIAN_POINT ( 'NONE',  ( -0.05014649552828365914, 215.4116977939061144, 72.24886208192143044 ) ) ;
#32786 = ORIENTED_EDGE ( 'NONE', *, *, #17216, .F. ) ;
#32787 = EDGE_CURVE ( 'NONE', #3834, #31333, #9866, .T. ) ;
#32788 = CARTESIAN_POINT ( 'NONE',  ( 81.02499999726880731, 149.9369285172503510, -15.58253175000000823 ) ) ;
#32789 = EDGE_LOOP ( 'NONE', ( #3880, #18837, #15151, #23939 ) ) ;
#32790 = CARTESIAN_POINT ( 'NONE',  ( 0.000000000000000000, 0.000000000000000000, -8.000000000000000000 ) ) ;
#32791 = AXIS2_PLACEMENT_3D ( 'NONE', #31732, #21508, #23732 ) ;
#32792 = VECTOR ( 'NONE', #9797, 999.9999999999998863 ) ;
#32793 = CARTESIAN_POINT ( 'NONE',  ( 75.42499999726879878, 168.2552932293087906, -9.630534252274385310 ) ) ;
#32794 = CARTESIAN_POINT ( 'NONE',  ( -7.500000000000000888, 3.988838049906426875, -0.8529248949437632232 ) ) ;
#32795 = CARTESIAN_POINT ( 'NONE',  ( -2.517493886308901807, 199.4062855549015012, 74.90113791807856103 ) ) ;
#32796 = CARTESIAN_POINT ( 'NONE',  ( 107.0104235265664556, 155.0000000000000000, -11.99999999999998224 ) ) ;
#32797 = AXIS2_PLACEMENT_3D ( 'NONE', #13566, #3175, #16110 ) ;
#32798 =( LENGTH_UNIT ( ) NAMED_UNIT ( * ) SI_UNIT ( .MILLI., .METRE. ) );
#32799 = CARTESIAN_POINT ( 'NONE',  ( 42.30000000000000426, 146.4771138417591203, -11.73074641843674470 ) ) ;
#32800 = CARTESIAN_POINT ( 'NONE',  ( -6.500168698208244500, 211.6636982574061676, 56.79886208192143471 ) ) ;
#32801 = CIRCLE ( 'NONE', #21403, 7.499999999999992895 ) ;
#32802 = DIRECTION ( 'NONE',  ( -0.9396926207859143121, 0.000000000000000000, -0.3420201433256525592 ) ) ;
#32803 = CARTESIAN_POINT ( 'NONE',  ( 77.78867513459483973, 155.0000000000000000, 15.00000000000001243 ) ) ;
#32804 = FACE_OUTER_BOUND ( 'NONE', #3817, .T. ) ;
#32805 = CARTESIAN_POINT ( 'NONE',  ( 47.82499999726881867, 168.2552932293087906, 9.630534252274372875 ) ) ;
#32806 = CARTESIAN_POINT ( 'NONE',  ( 66.67499999726881299, 141.7447067706911810, 9.630534252274376428 ) ) ;
#32807 = CARTESIAN_POINT ( 'NONE',  ( -9.736236675707914401, 199.9851607334237542, 60.20113791807857240 ) ) ;
#32808 = CARTESIAN_POINT ( 'NONE',  ( -120.4126214611401480, -2.643999646947226889, 35.00001199999999812 ) ) ;
#32809 = PRODUCT_DEFINITION_SHAPE ( 'NONE', 'NONE',  #31263 ) ;
#32810 = CARTESIAN_POINT ( 'NONE',  ( 7.375838497908181246, 196.7627149292499666, -0.5488620819214343749 ) ) ;
#32811 = CARTESIAN_POINT ( 'NONE',  ( -10.01549611932653860, 203.7984951890123000, 81.35113791807857808 ) ) ;
#32812 = CARTESIAN_POINT ( 'NONE',  ( 7.375838497908012492, 217.2372850707501186, 42.54886208192143471 ) ) ;
#32813 = CARTESIAN_POINT ( 'NONE',  ( -10.00000000000000711, 206.9523078486584495, 44.49886208192143755 ) ) ;
#32814 = FACE_OUTER_BOUND ( 'NONE', #15864, .T. ) ;
#32815 = CIRCLE ( 'NONE', #23029, 2.500000000000000000 ) ;
#32816 = CARTESIAN_POINT ( 'NONE',  ( 0.05014649552807549926, 219.6175466908591716, 82.25113791807856956 ) ) ;
#32817 = CARTESIAN_POINT ( 'NONE',  ( -3.044812012440131443, 216.5253028482142952, 1.101137918078565869 ) ) ;
#32818 = AXIS2_PLACEMENT_3D ( 'NONE', #8089, #18799, #408 ) ;
#32819 = CARTESIAN_POINT ( 'NONE',  ( 3.044812012439969795, 216.5253028482143520, 60.39886208192143613 ) ) ;
#32820 = CIRCLE ( 'NONE', #2900, 5.249999999999991118 ) ;
#32821 =( LENGTH_UNIT ( ) NAMED_UNIT ( * ) SI_UNIT ( .MILLI., .METRE. ) );
#32822 = ORIENTED_EDGE ( 'NONE', *, *, #28130, .F. ) ;
#32823 = CARTESIAN_POINT ( 'NONE',  ( 9.736236675708031640, 199.9851607334238963, 73.29886208192142760 ) ) ;
#32824 = ORIENTED_EDGE ( 'NONE', *, *, #381, .F. ) ;
#32825 = CARTESIAN_POINT ( 'NONE',  ( 72.17499999726881299, 164.1591823560292198, 12.60653300113718167 ) ) ;
#32826 = CARTESIAN_POINT ( 'NONE',  ( 2.426778023690075337, 214.6231898156240447, 39.39886208192144323 ) ) ;
#32827 = EDGE_LOOP ( 'NONE', ( #6531, #27666, #13757, #4802 ) ) ;
#32828 = ADVANCED_FACE ( 'NONE', ( #33376 ), #27382, .F. ) ;
#32829 = CARTESIAN_POINT ( 'NONE',  ( 80.57499999726880446, 145.8408176439707802, 12.60653300113718345 ) ) ;
#32830 = FACE_BOUND ( 'NONE', #26258, .T. ) ;
#32831 = VECTOR ( 'NONE', #29808, 1000.000000000000000 ) ;
#32832 = CARTESIAN_POINT ( 'NONE',  ( -9.040084412992170471, 207.3449885071057395, 103.1858979897393738 ) ) ;
#32833 = CARTESIAN_POINT ( 'NONE',  ( 2.517493886308900919, 214.5937144450984420, 61.40113791807856813 ) ) ;
#32834 = MECHANICAL_DESIGN_GEOMETRIC_PRESENTATION_REPRESENTATION (  '', ( #7268 ), #6181 ) ;
#32835 = CARTESIAN_POINT ( 'NONE',  ( 3.044812012439969795, 216.5253028482143520, 39.39886208192143613 ) ) ;
#32836 = ORIENTED_EDGE ( 'NONE', *, *, #1631, .F. ) ;
#32837 = FACE_OUTER_BOUND ( 'NONE', #9399, .T. ) ;
#32838 = EDGE_CURVE ( 'NONE', #1694, #889, #195, .T. ) ;
#32839 = COLOUR_RGB ( '', 0.31764706, 0.68627451, 0.89019608) ;
#32840 = DIRECTION ( 'NONE',  ( -1.000000000000000000, -0.000000000000000000, 0.000000000000000000 ) ) ;
#32841 = CARTESIAN_POINT ( 'NONE',  ( 10.39117206796836079, 1.272551561242683567E-15, -8.499999999999998224 ) ) ;
#32842 = CARTESIAN_POINT ( 'NONE',  ( 7.984503880673422316, 209.6470497212048372, 21.84886208192143542 ) ) ;
#32843 = CARTESIAN_POINT ( 'NONE',  ( 10.01549611932653860, 210.2015048109876716, 64.85113791807857808 ) ) ;
#32844 = CARTESIAN_POINT ( 'NONE',  ( -3.044812012440131443, 216.5253028482142952, 43.10113791807857808 ) ) ;
#32845 = CARTESIAN_POINT ( 'NONE',  ( 67.08867513459482268, 167.7597621252805880, -9.270509831248443078 ) ) ;
#32846 = CONTEXT_DEPENDENT_SHAPE_REPRESENTATION ( #18591, #6274 ) ;
#32847 = CARTESIAN_POINT ( 'NONE',  ( 10.00000000000000711, 206.9523078486586201, 14.00113791807856600 ) ) ;
#32848 = CARTESIAN_POINT ( 'NONE',  ( -2.517493886308901807, 199.4062855549015012, 8.901137918078566358 ) ) ;
#32849 = CARTESIAN_POINT ( 'NONE',  ( 44.12499999726881583, 155.0000000000000000, 15.58253174999999402 ) ) ;
#32850 = CARTESIAN_POINT ( 'NONE',  ( -3.811597179862308060, 5.304926841629211687, -0.01956314070068241109 ) ) ;
#32851 = CARTESIAN_POINT ( 'NONE',  ( 34.72499999726881015, 140.1801316387863778, -4.815267126137194431 ) ) ;
#32852 = CARTESIAN_POINT ( 'NONE',  ( 12.01549611932652972, 210.8513442034534933, 25.85113791807856742 ) ) ;
#32853 = CARTESIAN_POINT ( 'NONE',  ( 6.539198257601831266, -3.775407874310755307, -6.286450516130489774 ) ) ;
#32854 = EDGE_CURVE ( 'NONE', #9113, #8437, #17871, .T. ) ;
#32855 = CARTESIAN_POINT ( 'NONE',  ( -8.118202686958039038, 201.1607312380087080, 78.20113791807857240 ) ) ;
#32856 = CARTESIAN_POINT ( 'NONE',  ( -6.220909254589537696, 198.5229672870051445, 45.05113791807856671 ) ) ;
#32857 = CARTESIAN_POINT ( 'NONE',  ( 76.08867513459483689, 142.2402378747194405, 9.270509831248432420 ) ) ;
#32858 = AXIS2_PLACEMENT_3D ( 'NONE', #8255, #18644, #5852 ) ;
#32859 = PLANE ( 'NONE',  #542 ) ;
#32860 = CARTESIAN_POINT ( 'NONE',  ( -9.736236675708031640, 214.0148392665760753, 11.79886208192143648 ) ) ;
#32861 = CARTESIAN_POINT ( 'NONE',  ( 10.01549611932659367, 203.7984951890124421, 16.14886208192143613 ) ) ;
#32862 = CARTESIAN_POINT ( 'NONE',  ( 66.59999999453764019, 168.7903194862797420, 4.480746418436729606 ) ) ;
#32863 = VERTEX_POINT ( 'NONE', #28601 ) ;
#32864 = CARTESIAN_POINT ( 'NONE',  ( -11.98450388067348804, 210.9467285061362247, 54.65113791807857524 ) ) ;
#32865 = CARTESIAN_POINT ( 'NONE',  ( 2.426778023690261410, 199.3768101843759837, 80.60113791807857808 ) ) ;
#32866 = ADVANCED_FACE ( 'NONE', ( #33203 ), #28085, .T. ) ;
#32867 = CARTESIAN_POINT ( 'NONE',  ( 8.062137200540822946, 212.9164362838583315, 30.69886208192144039 ) ) ;
#32868 = DIRECTION ( 'NONE',  ( 0.000000000000000000, 0.000000000000000000, -1.000000000000000000 ) ) ;
#32869 = VERTEX_POINT ( 'NONE', #5089 ) ;
#32870 = AXIS2_PLACEMENT_3D ( 'NONE', #25181, #29966, #32346 ) ;
#32871 = EDGE_LOOP ( 'NONE', ( #1827, #32097, #24950, #9711 ) ) ;
#32872 = VECTOR ( 'NONE', #4048, 1000.000000000000000 ) ;
#32873 = VERTEX_POINT ( 'NONE', #25359 ) ;
#32874 = CARTESIAN_POINT ( 'NONE',  ( 107.5000000000000000, 155.0000000000000000, 69.99999999999998579 ) ) ;
#32875 = CARTESIAN_POINT ( 'NONE',  ( 0.000000000000000000, 0.000000000000000000, 0.000000000000000000 ) ) ;
#32876 = VERTEX_POINT ( 'NONE', #22976 ) ;
#32877 = CARTESIAN_POINT ( 'NONE',  ( 8.015496119326531499, 209.5516654185219636, 28.85113791807856032 ) ) ;
#32878 = CARTESIAN_POINT ( 'NONE',  ( 84.71132485994282035, 155.0000000000000000, 15.00000000000001243 ) ) ;
#32879 = CARTESIAN_POINT ( 'NONE',  ( -8.062137200540822946, 201.0835637161416400, 17.19886208192143684 ) ) ;
#32880 = CARTESIAN_POINT ( 'NONE',  ( 53.87499999726881583, 171.3844434931184253, -7.942151717890134290E-15 ) ) ;
#32881 = ORIENTED_EDGE ( 'NONE', *, *, #32201, .F. ) ;
#32882 = CARTESIAN_POINT ( 'NONE',  ( -7.984503880673488041, 209.6470497212046098, 54.65113791807857524 ) ) ;
#32883 = CARTESIAN_POINT ( 'NONE',  ( 5.416666666666667851, -4.378239541354669306, -5.848636054922037530 ) ) ;
#32884 = STYLED_ITEM ( 'NONE', ( #9851 ), #2741 ) ;
#32885 = FACE_OUTER_BOUND ( 'NONE', #9205, .T. ) ;
#32886 = CARTESIAN_POINT ( 'NONE',  ( 10.00000000000000711, 207.0476921513415220, 102.9988620819214447 ) ) ;
#32887 = CARTESIAN_POINT ( 'NONE',  ( 64.37499999726881583, 155.0000000000000000, 15.58253174999999402 ) ) ;
#32888 = CARTESIAN_POINT ( 'NONE',  ( -10.00000000000000711, 207.0476921513413515, 36.50113791807857666 ) ) ;
#32889 = ADVANCED_FACE ( 'NONE', ( #15483 ), #28266, .F. ) ;
#32890 = EDGE_CURVE ( 'NONE', #24566, #21928, #28503, .T. ) ;
#32891 = CARTESIAN_POINT ( 'NONE',  ( -8.118202686958039038, 201.1607312380087080, 21.20113791807856529 ) ) ;
#32892 = DIRECTION ( 'NONE',  ( 0.000000000000000000, -1.000000000000000000, 1.047444401652940007E-14 ) ) ;
#32893 = CARTESIAN_POINT ( 'NONE',  ( 79.19999999999998863, 167.3344367211045096, 8.961492836873468093 ) ) ;
#32894 = CARTESIAN_POINT ( 'NONE',  ( 0.000000000000000000, 0.000000000000000000, -6.800000000000000711 ) ) ;
#32895 = DIRECTION ( 'NONE',  ( -0.000000000000000000, 0.000000000000000000, -1.000000000000000000 ) ) ;
#32896 = CARTESIAN_POINT ( 'NONE',  ( 3.044812012440130555, 197.4746971517856764, 101.6011379180785781 ) ) ;
#32897 = CYLINDRICAL_SURFACE ( 'NONE', #16200, 15.00000000000001776 ) ;
#32898 = CARTESIAN_POINT ( 'NONE',  ( 50.17499999726881299, 164.1591823560292198, 12.60653300113718167 ) ) ;
#32899 = PRODUCT_RELATED_PRODUCT_CATEGORY ( 'part', '', ( #17886 ) ) ;
#32900 = EDGE_CURVE ( 'NONE', #8405, #29827, #3430, .T. ) ;
#32901 = CARTESIAN_POINT ( 'NONE',  ( -10.01549611932653860, 203.7984951890123284, 48.35113791807855677 ) ) ;
#32902 = CARTESIAN_POINT ( 'NONE',  ( 84.42499999726881299, 141.7447067706911810, 9.630534252274376428 ) ) ;
#32903 = LINE ( 'NONE', #6842, #31005 ) ;
#32904 = CARTESIAN_POINT ( 'NONE',  ( -31.74999999999995737, 0.000000000000000000, 0.000000000000000000 ) ) ;
#32905 = CARTESIAN_POINT ( 'NONE',  ( 48.89999999453763735, 159.7113355953771077, 14.49999999999999289 ) ) ;
#32906 = ORIENTED_EDGE ( 'NONE', *, *, #23457, .F. ) ;
#32907 = CARTESIAN_POINT ( 'NONE',  ( -7.375838497908182134, 217.2372850707499765, 27.95113791807857240 ) ) ;
#32908 = ADVANCED_FACE ( 'NONE', ( #15644 ), #20320, .T. ) ;
#32909 = CARTESIAN_POINT ( 'NONE',  ( 42.49999999999999289, -72.99999999999998579, -51.04834939252008041 ) ) ;
#32910 = CARTESIAN_POINT ( 'NONE',  ( 0.05014649552828275708, 196.4853777576173002, 1.748862081921434219 ) ) ;
#32911 =( REPRESENTATION_RELATIONSHIP ('NONE','NONE', #25663, #30038 ) REPRESENTATION_RELATIONSHIP_WITH_TRANSFORMATION ( #21121 )SHAPE_REPRESENTATION_RELATIONSHIP( ) );
#32912 = DIRECTION ( 'NONE',  ( 0.000000000000000000, 0.000000000000000000, -1.000000000000000000 ) ) ;
#32913 = VERTEX_POINT ( 'NONE', #4585 ) ;
#32914 = CARTESIAN_POINT ( 'NONE',  ( 10.01549611932653860, 210.2015048109876716, 1.851137918078565203 ) ) ;
#32915 = CARTESIAN_POINT ( 'NONE',  ( 3.135527875058820690, 216.4958274776887492, 64.40113791807857524 ) ) ;
#32916 = CARTESIAN_POINT ( 'NONE',  ( 6.444103211790928043, 211.7408657792734061, 18.69886208192143684 ) ) ;
#32917 = DIRECTION ( 'NONE',  ( 1.000000000000000000, 0.000000000000000000, 0.000000000000000000 ) ) ;
#32918 = ORIENTED_EDGE ( 'NONE', *, *, #11152, .T. ) ;
#32919 = CARTESIAN_POINT ( 'NONE',  ( 4.984841277089725686, 213.7757310962907411, 7.551137918078564049 ) ) ;
#32920 = DIRECTION ( 'NONE',  ( -1.000000000000000000, 0.000000000000000000, -0.000000000000000000 ) ) ;
#32921 = CARTESIAN_POINT ( 'NONE',  ( -9.680171189290716072, 199.9079932115567146, 89.19886208192144750 ) ) ;
#32922 = CARTESIAN_POINT ( 'NONE',  ( 40.37499999726880873, 155.0000000000000000, 15.58253174999999402 ) ) ;
#32923 = ORIENTED_EDGE ( 'NONE', *, *, #13269, .T. ) ;
#32924 = CARTESIAN_POINT ( 'NONE',  ( 45.92499999726881299, 164.1591823560292198, 12.60653300113718167 ) ) ;
#32925 = DIRECTION ( 'NONE',  ( 0.000000000000000000, 0.5000000000000008882, 0.8660254037844381525 ) ) ;
#32926 = CARTESIAN_POINT ( 'NONE',  ( 53.81132485994281467, 159.8737954434934920, -15.00000000000012434 ) ) ;
#32927 = CARTESIAN_POINT ( 'NONE',  ( -9.984503880673420539, 203.7031108863293980, 71.34886208192142476 ) ) ;
#32928 = CARTESIAN_POINT ( 'NONE',  ( 49.17499999726881299, 145.8408176439707802, -12.60653300113719588 ) ) ;
#32929 = CARTESIAN_POINT ( 'NONE',  ( 32.50000000000000000, 155.0000000000000000, -6.938893903907228378E-15 ) ) ;
#32930 = CARTESIAN_POINT ( 'NONE',  ( 6.220909254589536808, 215.4770327129947702, 1.551137918078565825 ) ) ;
#32931 = CARTESIAN_POINT ( 'NONE',  ( -3.500000000000000888, 1.362959798491803154, -0.1397344949837840966 ) ) ;
#32932 = CARTESIAN_POINT ( 'NONE',  ( 58.20000000000000284, 142.6655632788954620, -8.961492836873480528 ) ) ;
#32933 =( BOUNDED_CURVE ( )  B_SPLINE_CURVE ( 2, ( #7730, #13006, #18452, #10459, #28839, #10299, #10787, #28670, #18615, #23561, #2618 ),
 .UNSPECIFIED., .F., .F. ) 
 B_SPLINE_CURVE_WITH_KNOTS ( ( 3, 2, 2, 2, 2, 3 ),
 ( 0.8750000000000000000, 0.8785714285714285587, 0.8821428571428571175, 0.8857142857142856762, 0.8892857142857142350, 0.8928571428571427937 ),
 .UNSPECIFIED. ) 
 CURVE ( )  GEOMETRIC_REPRESENTATION_ITEM ( )  RATIONAL_B_SPLINE_CURVE ( ( 1.000000000000000000, 0.9510565162951534202, 1.000000000000000000, 0.9510565162951534202, 1.000000000000000000, 0.9510565162951534202, 1.000000000000000000, 0.9510565162951534202, 1.000000000000000000, 0.9510565162951534202, 1.000000000000000000 ) ) 
 REPRESENTATION_ITEM ( '' )  );
#32934 = CARTESIAN_POINT ( 'NONE',  ( 10.00000000000000711, 206.9523078486586201, 89.00113791807858377 ) ) ;
#32935 = CARTESIAN_POINT ( 'NONE',  ( -3.499999999999997780, -2.020725942163714262, -0.3126073911696551910 ) ) ;
#32936 = CARTESIAN_POINT ( 'NONE',  ( 0.05014649552828262524, 198.5883022060938572, 82.74886208192144466 ) ) ;
#32937 = DIRECTION ( 'NONE',  ( 0.000000000000000000, 1.000000000000000000, 0.000000000000000000 ) ) ;
#32938 = CARTESIAN_POINT ( 'NONE',  ( 127.5000000000000000, 48.99999999999998579, -2.149999999999999023 ) ) ;
#32939 = CARTESIAN_POINT ( 'NONE',  ( -3.662846001189865142, 195.5725841191952838, 85.89886208192143613 ) ) ;
#32940 = CARTESIAN_POINT ( 'NONE',  ( 64.82499999726881867, 141.7447067706911810, -9.630534252274385310 ) ) ;
#32942 = ORIENTED_EDGE ( 'NONE', *, *, #16858, .T. ) ;
#32941 = CARTESIAN_POINT ( 'NONE',  ( -6.139770520408368348, 215.5359834540460042, 18.95113791807856884 ) ) ;
#32943 = CARTESIAN_POINT ( 'NONE',  ( -13.75000000000001954, 23.81569860407205752, 0.000000000000000000 ) ) ;
#32944 = CARTESIAN_POINT ( 'NONE',  ( 82.87499999726878741, 138.6155565068815463, -3.929120461958505118E-15 ) ) ;
#32945 = CARTESIAN_POINT ( 'NONE',  ( 9.736236675707914401, 214.0148392665762458, 85.70113791807858661 ) ) ;
#32946 = CARTESIAN_POINT ( 'NONE',  ( 125.0000000000000568, -102.9999999999999716, -20.00000000000000000 ) ) ;
#32947 = ORIENTED_EDGE ( 'NONE', *, *, #21622, .T. ) ;
#32948 = CARTESIAN_POINT ( 'NONE',  ( 12.01549611932659367, 203.1486557965466773, 70.14886208192142192 ) ) ;
#32949 = CARTESIAN_POINT ( 'NONE',  ( 10.01549611932659367, 203.7984951890124421, 79.14886208192140771 ) ) ;
#32950 = CARTESIAN_POINT ( 'NONE',  ( 12.00000000000000711, 207.0476921513415220, 15.99886208192143400 ) ) ;
#32951 = CARTESIAN_POINT ( 'NONE',  ( 5.000000000000000000, 2.342598717236910488, 4.057499999999995666 ) ) ;
#32952 = CARTESIAN_POINT ( 'NONE',  ( 6.220909254589536808, 215.4770327129947702, 31.55113791807857382 ) ) ;
#32953 = DIRECTION ( 'NONE',  ( -1.000000000000000000, -0.000000000000000000, -0.000000000000000000 ) ) ;
#32954 = CARTESIAN_POINT ( 'NONE',  ( 8.118202686958138514, 201.1607312380088501, 100.2988620819214418 ) ) ;
#32955 = DIRECTION ( 'NONE',  ( 1.000000000000000000, -0.000000000000000000, -0.000000000000000000 ) ) ;
#32956 = EDGE_LOOP ( 'NONE', ( #16281, #10029, #14602, #25156 ) ) ;
#32957 = DIRECTION ( 'NONE',  ( 0.000000000000000000, 0.5000000000000014433, 0.8660254037844379305 ) ) ;
#32958 = CARTESIAN_POINT ( 'NONE',  ( 2.517493886309087436, 199.4062855549015865, 85.59886208192143897 ) ) ;
#32959 = ORIENTED_EDGE ( 'NONE', *, *, #22246, .T. ) ;
#32960 = CARTESIAN_POINT ( 'NONE',  ( 3.499999999999993339, -2.020725942163723143, -2.587392608830344720 ) ) ;
#32961 = ORIENTED_EDGE ( 'NONE', *, *, #4490, .F. ) ;
#32962 = FACE_BOUND ( 'NONE', #26787, .T. ) ;
#32963 = CARTESIAN_POINT ( 'NONE',  ( 76.62499999726880162, 138.6155565068815463, -3.929120461958505118E-15 ) ) ;
#32964 = CARTESIAN_POINT ( 'NONE',  ( -7.500000000000000888, 3.639598441879742907, -0.7155132341745253921 ) ) ;
#32965 = CARTESIAN_POINT ( 'NONE',  ( 4.903702542908601636, 200.1653181626581102, 80.45113791807857240 ) ) ;
#32966 = CARTESIAN_POINT ( 'NONE',  ( 10.40000000000000036, 0.000000000000000000, 0.000000000000000000 ) ) ;
#32967 = CARTESIAN_POINT ( 'NONE',  ( 40.10000000000000142, 141.2096805137202580, -4.480746418436742040 ) ) ;
#32968 = CARTESIAN_POINT ( 'NONE',  ( 6.444103211790928043, 211.7408657792734061, 57.69886208192144039 ) ) ;
#32969 = VECTOR ( 'NONE', #22373, 1000.000000000000227 ) ;
#32970 = DIRECTION ( 'NONE',  ( -1.000000000000000000, 0.000000000000000000, 0.000000000000000000 ) ) ;
#32971 = DIRECTION ( 'NONE',  ( 1.000000000000000000, 0.000000000000000000, 0.000000000000000000 ) ) ;
#32972 = LINE ( 'NONE', #29753, #18071 ) ;
#32973 = CARTESIAN_POINT ( 'NONE',  ( 49.02499999726880731, 149.9369285172503510, -15.58253175000000823 ) ) ;
#32974 = CARTESIAN_POINT ( 'NONE',  ( 64.17499999726879878, 164.1591823560292198, 12.60653300113718167 ) ) ;
#32975 = CARTESIAN_POINT ( 'NONE',  ( 12.00000000000000711, 206.9523078486586485, 59.00113791807856956 ) ) ;
#32976 = FACE_OUTER_BOUND ( 'NONE', #21017, .T. ) ;
#32977 = CARTESIAN_POINT ( 'NONE',  ( 8.118202686958039038, 212.8392687619912635, 100.7011379180785866 ) ) ;
#32978 = EDGE_CURVE ( 'NONE', #23288, #21869, #14972, .T. ) ;
#32979 = CARTESIAN_POINT ( 'NONE',  ( -0.05014649552810635652, 196.4853777576173002, 77.75113791807856956 ) ) ;
#32980 = AXIS2_PLACEMENT_3D ( 'NONE', #27732, #12230, #30465 ) ;
#32981 = CARTESIAN_POINT ( 'NONE',  ( 9.680171189290716072, 214.0920067884432854, 45.69886208192143329 ) ) ;
#32982 = CARTESIAN_POINT ( 'NONE',  ( 0.05014649552828275014, 196.4853777576173002, 43.74886208192143044 ) ) ;
#32983 = CARTESIAN_POINT ( 'NONE',  ( -65.20000000000000284, -0.9203920079924744480, -19.30000000000004690 ) ) ;
#32984 = CARTESIAN_POINT ( 'NONE',  ( -7.456977232089304408, 196.8216656703010301, 90.05113791807858092 ) ) ;
#32985 = CARTESIAN_POINT ( 'NONE',  ( 73.98867513459481415, 146.1832212156128890, 12.13525491562421976 ) ) ;
#32986 = CARTESIAN_POINT ( 'NONE',  ( -6.139770520408369237, 215.5359834540460042, 3.951137918078566180 ) ) ;
#32987 = CARTESIAN_POINT ( 'NONE',  ( 0.05014649552828275708, 196.4853777576173002, 67.74886208192140202 ) ) ;
#32988 = DIRECTION ( 'NONE',  ( 1.000000000000000000, -0.000000000000000000, -0.000000000000000000 ) ) ;
#32989 = ORIENTED_EDGE ( 'NONE', *, *, #3894, .F. ) ;
#32990 = CARTESIAN_POINT ( 'NONE',  ( 0.05014649552828288198, 194.3824533091408000, 67.74886208192143044 ) ) ;
#32991 = VERTEX_POINT ( 'NONE', #12583 ) ;
#32992 = CARTESIAN_POINT ( 'NONE',  ( 75.97499999726881015, 169.8198683612136222, 4.815267126137181997 ) ) ;
#32993 = CARTESIAN_POINT ( 'NONE',  ( -8.000000000000008882, 206.9523078486584780, 53.49886208192144466 ) ) ;
#32994 = ORIENTED_EDGE ( 'NONE', *, *, #1015, .F. ) ;
#32995 = VECTOR ( 'NONE', #8522, 1000.000000000000000 ) ;
#32996 = CARTESIAN_POINT ( 'NONE',  ( 81.67499999726884141, 168.2552932293087906, -9.630534252274387086 ) ) ;
#32997 = FACE_OUTER_BOUND ( 'NONE', #16864, .T. ) ;
#32998 = DIRECTION ( 'NONE',  ( 0.000000000000000000, 0.000000000000000000, -1.000000000000000000 ) ) ;
#32999 = CARTESIAN_POINT ( 'NONE',  ( 56.82499999726880446, 141.7447067706911810, -9.630534252274385310 ) ) ;
#33000 = CARTESIAN_POINT ( 'NONE',  ( 100.3007760113082156, 155.0000000000000000, -12.10452846326762177 ) ) ;
#33001 = CARTESIAN_POINT ( 'NONE',  ( 9.984503880673420539, 210.2968891136705167, 42.84886208192143897 ) ) ;
#33002 = ORIENTED_EDGE ( 'NONE', *, *, #13220, .T. ) ;
#33003 = CIRCLE ( 'NONE', #15598, 70.00000000000000000 ) ;
#33004 = CARTESIAN_POINT ( 'NONE',  ( 102.4138169258850581, 155.0000000000000000, -32.10452846326769816 ) ) ;
#33005 = DIRECTION ( 'NONE',  ( 1.000000000000000000, 0.000000000000000000, 0.000000000000000000 ) ) ;
#33006 = CARTESIAN_POINT ( 'NONE',  ( 117.5000000000000000, 65.35130719884917028, -52.99999999999947420 ) ) ;
#33007 = CARTESIAN_POINT ( 'NONE',  ( -7.984503880673422316, 204.3529502787951628, 26.34886208192143897 ) ) ;
#33008 = CARTESIAN_POINT ( 'NONE',  ( -9.984503880673473830, 210.2968891136704315, 57.65113791807858235 ) ) ;
#33009 = CARTESIAN_POINT ( 'NONE',  ( 6.139770520408368348, 198.4640165459539674, 47.45113791807857950 ) ) ;
#33010 = CARTESIAN_POINT ( 'NONE',  ( -8.118202686958039038, 201.1607312380087080, 21.20113791807856529 ) ) ;
#33011 = CARTESIAN_POINT ( 'NONE',  ( 0.05014649552807626948, 215.4116977939061144, 1.251137918078566225 ) ) ;
#33012 = CARTESIAN_POINT ( 'NONE',  ( 52.52499999726881441, 140.1801316387863778, 4.815267126137185549 ) ) ;
#33013 = CARTESIAN_POINT ( 'NONE',  ( -54.75000000000000711, -7.347880794884118356E-15, 35.00000000000000000 ) ) ;
#33014 = CARTESIAN_POINT ( 'NONE',  ( 87.50000000000002842, 145.7452232778646817, -11.80462230752951136 ) ) ;
#33015 = CARTESIAN_POINT ( 'NONE',  ( -7.456977232089304408, 196.8216656703010301, 33.05113791807856671 ) ) ;
#33016 = CARTESIAN_POINT ( 'NONE',  ( 6.746887896522740569, -3.895317543249826819, -6.526184258131365823 ) ) ;
#33017 = AXIS2_PLACEMENT_3D ( 'NONE', #10996, #31607, #8436 ) ;
#33018 = CARTESIAN_POINT ( 'NONE',  ( 10.01549611932653860, 210.2015048109876716, 76.85113791807857808 ) ) ;
#33019 = EDGE_CURVE ( 'NONE', #21434, #25041, #33629, .T. ) ;
#33020 = CARTESIAN_POINT ( 'NONE',  ( 0.05014649552810506589, 217.5146222423826714, 52.25113791807856956 ) ) ;
#33021 = MECHANICAL_DESIGN_GEOMETRIC_PRESENTATION_REPRESENTATION (  '', ( #12336 ), #20512 ) ;
#33022 = DIRECTION ( 'NONE',  ( 1.000000000000000000, -0.000000000000000000, -0.000000000000000000 ) ) ;
#33023 = VECTOR ( 'NONE', #18392, 1000.000000000000000 ) ;
#33024 = CARTESIAN_POINT ( 'NONE',  ( 12.00000000000000711, 207.0476921513415220, 9.998862081921435774 ) ) ;
#33025 = CARTESIAN_POINT ( 'NONE',  ( -10.01549611932659545, 210.2015048109875011, 20.64886208192143613 ) ) ;
#33026 = CARTESIAN_POINT ( 'NONE',  ( 74.49999999453764588, 170.2462022514548323, -7.872454543227099337E-15 ) ) ;
#33027 = VERTEX_POINT ( 'NONE', #4690 ) ;
#33028 = CARTESIAN_POINT ( 'NONE',  ( 12.00000000000000711, 206.9523078486586485, 59.00113791807856956 ) ) ;
#33029 = EDGE_CURVE ( 'NONE', #33215, #2474, #32801, .T. ) ;
#33030 = CARTESIAN_POINT ( 'NONE',  ( -4.984841277089726574, 200.2242689037092305, 75.05113791807858092 ) ) ;
#33031 = CARTESIAN_POINT ( 'NONE',  ( 3.044812012439969795, 216.5253028482143520, 45.39886208192143613 ) ) ;
#33032 = FACE_OUTER_BOUND ( 'NONE', #29197, .T. ) ;
#33033 = CIRCLE ( 'NONE', #2583, 10.39117206796836079 ) ;
#33034 = ORIENTED_EDGE ( 'NONE', *, *, #30367, .F. ) ;
#33035 = ADVANCED_FACE ( 'NONE', ( #12358 ), #31741, .T. ) ;
#33036 = VERTEX_POINT ( 'NONE', #4352 ) ;
#33037 = VERTEX_POINT ( 'NONE', #6909 ) ;
#33038 = CARTESIAN_POINT ( 'NONE',  ( 58.68867513459483121, 150.1262045565064227, -15.00000000000002665 ) ) ;
#33039 = DIRECTION ( 'NONE',  ( 0.000000000000000000, 0.000000000000000000, 1.000000000000000000 ) ) ;
#33040 = ORIENTED_EDGE ( 'NONE', *, *, #15990, .T. ) ;
#33041 = CARTESIAN_POINT ( 'NONE',  ( 0.05014649552807626948, 215.4116977939061144, 34.25113791807857666 ) ) ;
#33042 = EDGE_CURVE ( 'NONE', #6483, #16822, #6725, .T. ) ;
#33043 = CARTESIAN_POINT ( 'NONE',  ( 55.41132485994280898, 142.2402378747194405, -9.270509831248439525 ) ) ;
#33044 = CIRCLE ( 'NONE', #8566, 3.047499999999999876 ) ;
#33045 = CARTESIAN_POINT ( 'NONE',  ( -8.062137200540822946, 201.0835637161416400, 14.19886208192143684 ) ) ;
#33046 = CARTESIAN_POINT ( 'NONE',  ( 58.07499999726880446, 168.2552932293087906, 9.630534252274372875 ) ) ;
#33047 = EDGE_LOOP ( 'NONE', ( #29710, #10230, #7906, #7593 ) ) ;
#33048 = CARTESIAN_POINT ( 'NONE',  ( 8.015496119326531499, 209.5516654185219636, 49.85113791807857808 ) ) ;
#33049 = DIRECTION ( 'NONE',  ( 0.7071067811865461294, 8.659560562354951347E-17, 0.7071067811865489050 ) ) ;
#33050 =( NAMED_UNIT ( * ) SI_UNIT ( $, .STERADIAN. ) SOLID_ANGLE_UNIT ( ) );
#33051 = DIRECTION ( 'NONE',  ( 0.000000000000000000, 0.000000000000000000, -1.000000000000000000 ) ) ;
#33052 = CARTESIAN_POINT ( 'NONE',  ( -0.05014649552828403384, 217.5146222423826714, 99.24886208192143044 ) ) ;
#33053 = EDGE_CURVE ( 'NONE', #1780, #4795, #11085, .T. ) ;
#33054 = CARTESIAN_POINT ( 'NONE',  ( 66.57499999726881867, 145.8408176439707802, 12.60653300113718345 ) ) ;
#33055 = CARTESIAN_POINT ( 'NONE',  ( 3.044812012440130555, 197.4746971517856764, 32.60113791807857098 ) ) ;
#33056 = CARTESIAN_POINT ( 'NONE',  ( -6.818272094961329799, -1.321852500971156363, -6.208027553811807486 ) ) ;
#33057 = CARTESIAN_POINT ( 'NONE',  ( -10.01549611932653860, 203.7984951890123284, 21.35113791807855677 ) ) ;
#33058 = DIRECTION ( 'NONE',  ( 0.000000000000000000, 0.000000000000000000, -1.000000000000000000 ) ) ;
#33059 = CARTESIAN_POINT ( 'NONE',  ( 80.80000000000001137, 167.3344367211045096, -8.961492836873482304 ) ) ;
#33060 = CARTESIAN_POINT ( 'NONE',  ( -58.50000000000002132, 194.9217985566782829, -2.500000000000000000 ) ) ;
#33061 = FACE_OUTER_BOUND ( 'NONE', #18084, .T. ) ;
#33062 = CARTESIAN_POINT ( 'NONE',  ( -9.984503880673473830, 210.2968891136704315, 99.65113791807853261 ) ) ;
#33063 = DIRECTION ( 'NONE',  ( -0.000000000000000000, -0.000000000000000000, 1.000000000000000000 ) ) ;
#33064 = CARTESIAN_POINT ( 'NONE',  ( 50.07499999726881157, 168.2552932293087906, 9.630534252274372875 ) ) ;
#33065 = CARTESIAN_POINT ( 'NONE',  ( -10.01549611932653860, 203.7984951890123284, 51.35113791807858519 ) ) ;
#33066 = ADVANCED_FACE ( 'NONE', ( #19852 ), #25127, .F. ) ;
#33067 = CARTESIAN_POINT ( 'NONE',  ( 82.72499999726881015, 140.1801316387863778, -4.815267126137194431 ) ) ;
#33068 = DIRECTION ( 'NONE',  ( -0.000000000000000000, -0.000000000000000000, -1.000000000000000000 ) ) ;
#33069 = CARTESIAN_POINT ( 'NONE',  ( 64.81132485994280046, 150.1262045565066785, 15.00000000000020250 ) ) ;
#33070 = CARTESIAN_POINT ( 'NONE',  ( 52.69999999453762740, 167.3344367211045096, 8.961492836873468093 ) ) ;
#33071 = VERTEX_POINT ( 'NONE', #30249 ) ;
#33072 = CARTESIAN_POINT ( 'NONE',  ( -12.01549611932652972, 203.1486557965464499, 30.35113791807856742 ) ) ;
#33073 = CIRCLE ( 'NONE', #26543, 98.00000000000002842 ) ;
#33074 = DIRECTION ( 'NONE',  ( 0.000000000000000000, 0.000000000000000000, 1.000000000000000000 ) ) ;
#33075 = CARTESIAN_POINT ( 'NONE',  ( -6.220909254589682469, 215.4770327129946850, 5.948862081921435063 ) ) ;
#33076 = AXIS2_PLACEMENT_3D ( 'NONE', #16354, #18596, #29652 ) ;
#33077 = CARTESIAN_POINT ( 'NONE',  ( 92.60208470531341618, 155.0000000000000000, 0.000000000000000000 ) ) ;
#33078 = VERTEX_POINT ( 'NONE', #1790 ) ;
#33079 = AXIS2_PLACEMENT_3D ( 'NONE', #29741, #30251, #27691 ) ;
#33080 = CARTESIAN_POINT ( 'NONE',  ( 9.984503880673470277, 203.7031108863295401, -0.8488620819214341973 ) ) ;
#33081 = CARTESIAN_POINT ( 'NONE',  ( -9.984503880673473830, 210.2968891136704315, 63.65113791807857524 ) ) ;
#33082 =( BOUNDED_CURVE ( )  B_SPLINE_CURVE ( 2, ( #30152, #11424, #9200, #27580, #32693, #9361, #29984, #11925, #6983, #14644, #27253 ),
 .UNSPECIFIED., .F., .T. ) 
 B_SPLINE_CURVE_WITH_KNOTS ( ( 3, 2, 2, 2, 2, 3 ),
 ( 0.7500000000000000000, 0.7535714285714285587, 0.7571428571428571175, 0.7607142857142855652, 0.7642857142857141239, 0.7678571428571427937 ),
 .UNSPECIFIED. ) 
 CURVE ( )  GEOMETRIC_REPRESENTATION_ITEM ( )  RATIONAL_B_SPLINE_CURVE ( ( 1.000000000000000000, 0.9510565162951534202, 1.000000000000000000, 0.9510565162951534202, 1.000000000000000000, 0.9510565162951534202, 1.000000000000000000, 0.9510565162951534202, 1.000000000000000000, 0.9510565162951549745, 0.9999999999999984457 ) ) 
 REPRESENTATION_ITEM ( '' )  );
#33083 = VERTEX_POINT ( 'NONE', #16953 ) ;
#33084 = CARTESIAN_POINT ( 'NONE',  ( -8.015496119326597224, 209.5516654185217362, 23.64886208192143968 ) ) ;
#33085 = EDGE_CURVE ( 'NONE', #3502, #8327, #3996, .T. ) ;
#33086 = AXIS2_PLACEMENT_3D ( 'NONE', #189, #5290, #10587 ) ;
#33087 = CARTESIAN_POINT ( 'NONE',  ( 49.98867513459481415, 146.1832212156128890, 12.13525491562421976 ) ) ;
#33088 = ORIENTED_EDGE ( 'NONE', *, *, #7298, .T. ) ;
#33089 = CARTESIAN_POINT ( 'NONE',  ( 2.426778023690261410, 199.3768101843759837, 2.601137918078566535 ) ) ;
#33090 = EDGE_CURVE ( 'NONE', #17333, #8582, #1945, .T. ) ;
#33091 = CARTESIAN_POINT ( 'NONE',  ( 108.0049454219347354, 155.0000000000000000, 12.10452846326765020 ) ) ;
#33092 = CARTESIAN_POINT ( 'NONE',  ( -9.680171189290716072, 199.9079932115567146, 86.19886208192144750 ) ) ;
#33093 = CARTESIAN_POINT ( 'NONE',  ( 38.47499999726881015, 149.9369285172503510, 15.58253174999999580 ) ) ;
#33094 = ORIENTED_EDGE ( 'NONE', *, *, #25720, .F. ) ;
#33095 = CARTESIAN_POINT ( 'NONE',  ( 44.32499999726881157, 145.8408176439707802, 12.60653300113718345 ) ) ;
#33096 = DIRECTION ( 'NONE',  ( 0.000000000000000000, 0.000000000000000000, -1.000000000000000000 ) ) ;
#33097 = CARTESIAN_POINT ( 'NONE',  ( 3.135527875058820690, 216.4958274776887492, 1.401137918078565914 ) ) ;
#33098 = CARTESIAN_POINT ( 'NONE',  ( -6.139770520408224463, 198.4640165459539389, 68.04886208192142760 ) ) ;
#33099 = EDGE_CURVE ( 'NONE', #30928, #8859, #12704, .T. ) ;
#33100 = CARTESIAN_POINT ( 'NONE',  ( 46.27499999726881441, 160.0630714827496206, 15.58253174999999402 ) ) ;
#33101 = LINE ( 'NONE', #25092, #32593 ) ;
#33102 = CARTESIAN_POINT ( 'NONE',  ( -6.220909254589537696, 198.5229672870051161, 6.051137918078566713 ) ) ;
#33103 = PRODUCT ( 'High-Force Belleville Spring Washer Pack', 'High-Force Belleville Spring Washer Pack', '', ( #16165 ) ) ;
#33104 = CARTESIAN_POINT ( 'NONE',  ( -14.91983402814537740, -23.14029461301516832, -0.01440555954224943640 ) ) ;
#33105 = AXIS2_PLACEMENT_3D ( 'NONE', #11388, #29614, #26709 ) ;
#33106 = CARTESIAN_POINT ( 'NONE',  ( 63.29999999999999716, 163.5228861582408797, 11.73074641843673049 ) ) ;
#33107 = CARTESIAN_POINT ( 'NONE',  ( -8.062137200540920645, 212.9164362838581894, 90.80113791807858092 ) ) ;
#33108 = CARTESIAN_POINT ( 'NONE',  ( 0.000000000000000000, -2.342598717236912265, -4.057499999999995666 ) ) ;
#33109 = CARTESIAN_POINT ( 'NONE',  ( -10.00000000000000711, 207.0476921513413515, 78.50113791807856956 ) ) ;
#33110 = CARTESIAN_POINT ( 'NONE',  ( -5.112021521198522933, 5.708827036477257977, -7.069802615102034338 ) ) ;
#33111 = CARTESIAN_POINT ( 'NONE',  ( 34.47499999726881015, 149.9369285172503510, 15.58253174999999580 ) ) ;
#33112 = CARTESIAN_POINT ( 'NONE',  ( 11.98450388067341876, 210.9467285061363953, 90.84886208192142476 ) ) ;
#33113 = TOROIDAL_SURFACE ( 'NONE', #30939, 9.624472924841564136, 1.000000000000000444 ) ;
#33114 = CARTESIAN_POINT ( 'NONE',  ( 61.12499999726880873, 155.0000000000000000, -15.58253175000000823 ) ) ;
#33116 = EDGE_LOOP ( 'NONE', ( #11799, #1231 ) ) ;
#33115 = CARTESIAN_POINT ( 'NONE',  ( 8.118202686958039038, 212.8392687619912635, 25.70113791807856529 ) ) ;
#33117 = CARTESIAN_POINT ( 'NONE',  ( 86.78867513459481131, 155.0000000000000000, -15.00000000000002487 ) ) ;
#33118 = CARTESIAN_POINT ( 'NONE',  ( 86.87499999726880162, 138.6155565068815463, -3.929120461958505118E-15 ) ) ;
#33119 = CARTESIAN_POINT ( 'NONE',  ( -7.375838497908182134, 217.2372850707499765, 90.95113791807855819 ) ) ;
#33120 = DIRECTION ( 'NONE',  ( 1.000000000000000000, 0.000000000000000000, 0.000000000000000000 ) ) ;
#33121 = ORIENTED_EDGE ( 'NONE', *, *, #13501, .F. ) ;
#33122 = CARTESIAN_POINT ( 'NONE',  ( 12.01549611932659367, 203.1486557965466773, 73.14886208192142192 ) ) ;
#33123 = CARTESIAN_POINT ( 'NONE',  ( -10.01549611932659545, 210.2015048109875011, 89.64886208192143613 ) ) ;
#33124 = CARTESIAN_POINT ( 'NONE',  ( -3.753561863808878130, 218.3979405102790281, 9.098862081921435419 ) ) ;
#33125 = LINE ( 'NONE', #22566, #155 ) ;
#33126 = TOROIDAL_SURFACE ( 'NONE', #11385, 2.200000000000001066, 0.2000000000000000111 ) ;
#33127 = CARTESIAN_POINT ( 'NONE',  ( -3.044812012440131443, 216.5253028482142952, 28.10113791807857098 ) ) ;
#33128 = CARTESIAN_POINT ( 'NONE',  ( -3.750000000000004885, 6.495190528383289141, 0.000000000000000000 ) ) ;
#33129 = CARTESIAN_POINT ( 'NONE',  ( 3.044812012439969795, 216.5253028482143520, 96.39886208192145034 ) ) ;
#33130 = EDGE_CURVE ( 'NONE', #12310, #2726, #1276, .T. ) ;
#33131 = ADVANCED_FACE ( 'NONE', ( #17465, #9124 ), #27850, .F. ) ;
#33132 = CIRCLE ( 'NONE', #32032, 24.99999999999999289 ) ;
#33133 = DIRECTION ( 'NONE',  ( 1.000000000000000000, 0.000000000000000000, 0.000000000000000000 ) ) ;
#33134 = DIRECTION ( 'NONE',  ( 1.000000000000000000, 0.000000000000000000, 0.000000000000000000 ) ) ;
#33135 = ORIENTED_EDGE ( 'NONE', *, *, #179, .F. ) ;
#33136 = DIRECTION ( 'NONE',  ( 1.000000000000000000, 0.000000000000000000, 0.000000000000000000 ) ) ;
#33137 = CARTESIAN_POINT ( 'NONE',  ( -7.984503880673422316, 204.3529502787951628, 77.34886208192143897 ) ) ;
#33138 = ORIENTED_EDGE ( 'NONE', *, *, #32645, .T. ) ;
#33139 = PRODUCT_DEFINITION ( 'UNKNOWN', '', #12094, #22022 ) ;
#33140 = EDGE_CURVE ( 'NONE', #30882, #8055, #14333, .T. ) ;
#33141 = AXIS2_PLACEMENT_3D ( 'NONE', #7520, #2403, #33234 ) ;
#33142 = FACE_OUTER_BOUND ( 'NONE', #6986, .T. ) ;
#33143 = VERTEX_POINT ( 'NONE', #7255 ) ;
#33144 = DIRECTION ( 'NONE',  ( 0.000000000000000000, 1.000000000000000000, -1.100686371591861952E-15 ) ) ;
#33145 = CARTESIAN_POINT ( 'NONE',  ( 73.47499999726879594, 160.0630714827496206, -15.58253175000000823 ) ) ;
#33146 = CARTESIAN_POINT ( 'NONE',  ( 81.92499999726882720, 164.1591823560292198, 12.60653300113718167 ) ) ;
#33147 = CARTESIAN_POINT ( 'NONE',  ( 0.000000000000000000, 0.000000000000000000, -25.03750572909317285 ) ) ;
#33148 = CARTESIAN_POINT ( 'NONE',  ( 6.444103211791042618, 202.2591342207267644, 83.30113791807858092 ) ) ;
#33149 = LINE ( 'NONE', #20192, #5382 ) ;
#33150 = SURFACE_SIDE_STYLE ('',( #15253 ) ) ;
#33151 = CARTESIAN_POINT ( 'NONE',  ( 44.10000000000000142, 141.2096805137202580, -4.480746418436742040 ) ) ;
#33152 = CARTESIAN_POINT ( 'NONE',  ( -7.984503880673422316, 204.3529502787951628, 50.34886208192144608 ) ) ;
#33153 = VECTOR ( 'NONE', #21007, 1000.000000000000000 ) ;
#33154 = FACE_OUTER_BOUND ( 'NONE', #19261, .T. ) ;
#33155 = CARTESIAN_POINT ( 'NONE',  ( -150.0000000000000000, 0.000000000000000000, -35.00000000000000000 ) ) ;
#33156 = CARTESIAN_POINT ( 'NONE',  ( -123.6258236071138015, 5.113356552508662389, 35.00001200000000523 ) ) ;
#33157 = CARTESIAN_POINT ( 'NONE',  ( 60.02499999726881441, 160.0630714827496206, 15.58253174999999224 ) ) ;
#33158 = CARTESIAN_POINT ( 'NONE',  ( 63.17499999726880588, 145.8408176439707802, -12.60653300113719588 ) ) ;
#33159 = CARTESIAN_POINT ( 'NONE',  ( -7.456977232089304408, 196.8216656703010301, 54.05113791807856671 ) ) ;
#33160 = DIRECTION ( 'NONE',  ( 0.000000000000000000, 0.9988620819214347746, -0.04769215134146093105 ) ) ;
#33161 = CARTESIAN_POINT ( 'NONE',  ( 9.680171189290831535, 199.9079932115568852, -0.6988620819214345081 ) ) ;
#33163 = CARTESIAN_POINT ( 'NONE',  ( -10.01549611932653860, 203.7984951890123000, 75.35113791807854966 ) ) ;
#33162 =( REPRESENTATION_RELATIONSHIP ('NONE','NONE', #25663, #22175 ) REPRESENTATION_RELATIONSHIP_WITH_TRANSFORMATION ( #9007 )SHAPE_REPRESENTATION_RELATIONSHIP( ) );
#33164 = CARTESIAN_POINT ( 'NONE',  ( 12.00000000000000711, 207.0476921513415220, 39.99886208192143755 ) ) ;
#33165 = CARTESIAN_POINT ( 'NONE',  ( -0.05014649552828402690, 217.5146222423826714, 51.24886208192143755 ) ) ;
#33166 = CARTESIAN_POINT ( 'NONE',  ( -6.500000000000000888, 0.000000000000000000, 0.000000000000000000 ) ) ;
#33167 = CARTESIAN_POINT ( 'NONE',  ( -7.375838497908182134, 217.2372850707499765, 84.95113791807858661 ) ) ;
#33168 = CARTESIAN_POINT ( 'NONE',  ( 68.11132485994281183, 169.2658477444273331, -4.635254915624224203 ) ) ;
#33169 = CARTESIAN_POINT ( 'NONE',  ( -3.044812012440131443, 216.5253028482142952, 7.101137918078566535 ) ) ;
#33170 = CARTESIAN_POINT ( 'NONE',  ( 8.062137200540822946, 212.9164362838583315, 72.69886208192143329 ) ) ;
#33172 = ORIENTED_EDGE ( 'NONE', *, *, #5953, .T. ) ;
#33171 = B_SPLINE_CURVE_WITH_KNOTS ( 'NONE', 3,
 ( #26758, #3422, #3591, #13984, #16124, #1131 ),
 .UNSPECIFIED., .F., .F.,
 ( 4, 2, 4 ),
 ( 0.000000000000000000, 0.0004189869898914143787, 0.0008379739797828287574 ),
 .UNSPECIFIED. ) ;
#33173 = CARTESIAN_POINT ( 'NONE',  ( 3.662846001189864698, 218.4274158808046593, 69.39886208192143613 ) ) ;
#33174 = ORIENTED_EDGE ( 'NONE', *, *, #3963, .T. ) ;
#33175 = CARTESIAN_POINT ( 'NONE',  ( 75.07499999726879025, 141.7447067706911810, -9.630534252274385310 ) ) ;
#33176 = CARTESIAN_POINT ( 'NONE',  ( -6.500168698208244500, 211.6636982574061676, 47.79886208192144181 ) ) ;
#33177 = AXIS2_PLACEMENT_3D ( 'NONE', #6286, #14635, #29809 ) ;
#33178 = VERTEX_POINT ( 'NONE', #29917 ) ;
#33179 = ADVANCED_FACE ( 'NONE', ( #14409 ), #24802, .T. ) ;
#33180 = CARTESIAN_POINT ( 'NONE',  ( 68.72499999726881015, 140.1801316387863778, -4.815267126137194431 ) ) ;
#33181 = CARTESIAN_POINT ( 'NONE',  ( 6.500000000000000000, 0.6659426636835951152, -5.719325464431898709 ) ) ;
#33182 = CARTESIAN_POINT ( 'NONE',  ( 0.000000000000000000, 0.000000000000000000, -17.97459999999999525 ) ) ;
#33183 = CARTESIAN_POINT ( 'NONE',  ( 62.82499999726881867, 141.7447067706911810, -9.630534252274385310 ) ) ;
#33184 = DIRECTION ( 'NONE',  ( 0.000000000000000000, 1.000000000000000000, -1.224646799147353207E-16 ) ) ;
#33185 = CARTESIAN_POINT ( 'NONE',  ( 10.00000000000000711, 207.0476921513415220, 39.99886208192143755 ) ) ;
#33186 = ORIENTED_EDGE ( 'NONE', *, *, #6402, .F. ) ;
#33187 = DIRECTION ( 'NONE',  ( 1.000000000000000000, -0.000000000000000000, -0.000000000000000000 ) ) ;
#33188 = PLANE ( 'NONE',  #19388 ) ;
#33189 = CARTESIAN_POINT ( 'NONE',  ( 86.41132485994282320, 167.7597621252805880, 9.270509831248428867 ) ) ;
#33190 = CARTESIAN_POINT ( 'NONE',  ( -8.000000000000008882, 206.9523078486584780, 29.49886208192143400 ) ) ;
#33191 = CARTESIAN_POINT ( 'NONE',  ( -8.118202686958039038, 201.1607312380087080, 72.20113791807857240 ) ) ;
#33192 = DIRECTION ( 'NONE',  ( -1.000000000000000000, 0.000000000000000000, -0.000000000000000000 ) ) ;
#33193 = CARTESIAN_POINT ( 'NONE',  ( -9.984503880673473830, 210.2968891136704315, 48.65113791807858235 ) ) ;
#33194 = CARTESIAN_POINT ( 'NONE',  ( 6.139770520408368348, 198.4640165459539674, 14.45113791807856352 ) ) ;
#33195 = CARTESIAN_POINT ( 'NONE',  ( -6.500168698208129925, 202.3363017425936050, 6.201137918078567068 ) ) ;
#33196 = DIRECTION ( 'NONE',  ( 1.000000000000000000, 0.000000000000000000, 0.000000000000000000 ) ) ;
#33197 = CARTESIAN_POINT ( 'NONE',  ( 37.52499999726881441, 169.8198683612136222, -4.815267126137197984 ) ) ;
#33198 = ADVANCED_BREP_SHAPE_REPRESENTATION ( '', ( #23704, #2404 ), #20321 ) ;
#33199 = CARTESIAN_POINT ( 'NONE',  ( -12.00000000000000711, 207.0476921513413515, 27.50113791807856956 ) ) ;
#33200 = CARTESIAN_POINT ( 'NONE',  ( 4.000000000000000000, -1.759474945355381958, 3.047500000000001208 ) ) ;
#33201 = CARTESIAN_POINT ( 'NONE',  ( -10.01549611932653860, 203.7984951890123284, 75.35113791807853545 ) ) ;
#33202 = CARTESIAN_POINT ( 'NONE',  ( 10.01549611932653860, 210.2015048109876716, 49.85113791807857808 ) ) ;
#33203 = FACE_OUTER_BOUND ( 'NONE', #47, .T. ) ;
#33204 = CARTESIAN_POINT ( 'NONE',  ( 54.48867513459482836, 142.2402378747194405, -9.270509831248439525 ) ) ;
#33205 = CARTESIAN_POINT ( 'NONE',  ( 7.456977232089471386, 196.8216656703012006, 13.44886208192143684 ) ) ;
#33206 = CARTESIAN_POINT ( 'NONE',  ( -8.062137200540822946, 201.0835637161416400, 23.19886208192143684 ) ) ;
#33207 = CARTESIAN_POINT ( 'NONE',  ( 72.79999999453762882, 163.5228861582408797, 11.73074641843673049 ) ) ;
#33208 = VERTEX_POINT ( 'NONE', #12530 ) ;
#33209 = CARTESIAN_POINT ( 'NONE',  ( 3.753561863808689836, 218.3979405102790565, 61.40113791807856103 ) ) ;
#33210 = CARTESIAN_POINT ( 'NONE',  ( -6.444103211791042618, 211.7408657792732356, 81.80113791807858092 ) ) ;
#33211 = CARTESIAN_POINT ( 'NONE',  ( 8.062137200540822946, 212.9164362838583315, 39.69886208192143329 ) ) ;
#33212 = AXIS2_PLACEMENT_3D ( 'NONE', #1012, #11407, #8352 ) ;
#33213 = CARTESIAN_POINT ( 'NONE',  ( 115.4999999999999858, 155.0000000000000000, 49.99999999999999289 ) ) ;
#33214 = ORIENTED_EDGE ( 'NONE', *, *, #8681, .F. ) ;
#33215 = VERTEX_POINT ( 'NONE', #20369 ) ;
#33216 = ORIENTED_EDGE ( 'NONE', *, *, #14492, .T. ) ;
#33217 = CARTESIAN_POINT ( 'NONE',  ( -60.00000000000000000, -7.347880794884118356E-15, 20.00000000000001776 ) ) ;
#33218 = CARTESIAN_POINT ( 'NONE',  ( 10.00000000000000711, 207.0476921513415220, 0.9988620819214341084 ) ) ;
#33219 = ORIENTED_EDGE ( 'NONE', *, *, #21235, .F. ) ;
#33220 = CARTESIAN_POINT ( 'NONE',  ( -4.903702542908602524, 213.8346818373418898, 27.95113791807857240 ) ) ;
#33221 = CARTESIAN_POINT ( 'NONE',  ( 55.11132485994280472, 140.7341522555726669, 4.635254915624211769 ) ) ;
#33222 = ADVANCED_FACE ( 'NONE', ( #12695 ), #2814, .T. ) ;
#33223 = CARTESIAN_POINT ( 'NONE',  ( -3.135527875058982783, 216.4958274776886924, 15.09886208192143542 ) ) ;
#33224 = CARTESIAN_POINT ( 'NONE',  ( 59.47499999726880304, 160.0630714827496206, -15.58253175000000823 ) ) ;
#33225 = VERTEX_POINT ( 'NONE', #21030 ) ;
#33226 = CARTESIAN_POINT ( 'NONE',  ( -6.500168698208129925, 202.3363017425936050, 63.20113791807857240 ) ) ;
#33227 = DIRECTION ( 'NONE',  ( 1.000000000000000000, 0.000000000000000000, 0.000000000000000000 ) ) ;
#33228 = CARTESIAN_POINT ( 'NONE',  ( 57.01132485994281041, 142.2402378747194405, 9.270509831248432420 ) ) ;
#33229 = CARTESIAN_POINT ( 'NONE',  ( -10.00000000000000711, 206.9523078486584495, 104.4988620819214447 ) ) ;
#33230 = CARTESIAN_POINT ( 'NONE',  ( 67.67499999726881299, 168.2552932293087906, -9.630534252274385310 ) ) ;
#33231 = CARTESIAN_POINT ( 'NONE',  ( 6.220909254589536808, 215.4770327129947702, 46.55113791807856671 ) ) ;
#33232 = FACE_OUTER_BOUND ( 'NONE', #18678, .T. ) ;
#33233 = CARTESIAN_POINT ( 'NONE',  ( -6.220909254589537696, 198.5229672870051161, 15.05113791807856671 ) ) ;
#33234 = DIRECTION ( 'NONE',  ( 0.000000000000000000, 0.000000000000000000, -1.000000000000000000 ) ) ;
#33235 = AXIS2_PLACEMENT_3D ( 'NONE', #187, #13126, #23682 ) ;
#33236 = APPLICATION_PROTOCOL_DEFINITION ( 'draft international standard', 'automotive_design', 1998, #20725 ) ;
#33237 = CARTESIAN_POINT ( 'NONE',  ( 86.79999999999998295, 167.3344367211045096, -8.961492836873482304 ) ) ;
#33238 = SURFACE_STYLE_USAGE ( .BOTH. , #17055 ) ;
#33239 = DIRECTION ( 'NONE',  ( 0.000000000000000000, 0.000000000000000000, -1.000000000000000000 ) ) ;
#33240 = CARTESIAN_POINT ( 'NONE',  ( 7.375838497908181246, 196.7627149292499666, -0.5488620819214343749 ) ) ;
#33241 = CARTESIAN_POINT ( 'NONE',  ( 4.000000000000000000, 3.518949890710768802, -4.770489558936219510E-15 ) ) ;
#33242 = CARTESIAN_POINT ( 'NONE',  ( 53.87499999726881583, 171.3844434931184253, -7.942151717890132712E-15 ) ) ;
#33243 = CARTESIAN_POINT ( 'NONE',  ( -9.984503880673473830, 210.2968891136704315, 51.65113791807855392 ) ) ;
#33244 = CARTESIAN_POINT ( 'NONE',  ( 87.32499999726880446, 164.1591823560292198, -12.60653300113719766 ) ) ;
#33245 = CARTESIAN_POINT ( 'NONE',  ( 52.11132485994280472, 169.2658477444273331, -4.635254915624224203 ) ) ;
#33246 = CARTESIAN_POINT ( 'NONE',  ( -5.007715329123872641E-16, -8.660254037844399733, -7.422398894150038728 ) ) ;
#33247 = CARTESIAN_POINT ( 'NONE',  ( 55.09999999453761887, 150.2886644046228639, 14.49999999999999645 ) ) ;
#33248 = EDGE_LOOP ( 'NONE', ( #16069, #32694, #5884, #18222 ) ) ;
#33249 = CARTESIAN_POINT ( 'NONE',  ( 7.456977232089302632, 217.1783343296989131, 28.55113791807857027 ) ) ;
#33250 = CARTESIAN_POINT ( 'NONE',  ( 60.00000000000000000, 7.347880794884118356E-15, -35.00000000000000000 ) ) ;
#33251 = CARTESIAN_POINT ( 'NONE',  ( 3.135527875058981895, 197.5041725223112792, 10.59886208192143542 ) ) ;
#33252 = FACE_OUTER_BOUND ( 'NONE', #27145, .T. ) ;
#33253 = ORIENTED_EDGE ( 'NONE', *, *, #24584, .F. ) ;
#33254 = CARTESIAN_POINT ( 'NONE',  ( -6.139770520408369237, 215.5359834540460042, 6.951137918078566180 ) ) ;
#33255 = CARTESIAN_POINT ( 'NONE',  ( 8.118202686958039038, 212.8392687619912635, 58.70113791807857240 ) ) ;
#33256 = EDGE_CURVE ( 'NONE', #32112, #16822, #28548, .T. ) ;
#33257 = ORIENTED_EDGE ( 'NONE', *, *, #1176, .T. ) ;
#33258 = CARTESIAN_POINT ( 'NONE',  ( 0.05014649552828262524, 198.5883022060938572, 22.74886208192143755 ) ) ;
#33259 = DIRECTION ( 'NONE',  ( 0.000000000000000000, 0.000000000000000000, 1.000000000000000000 ) ) ;
#33260 = VECTOR ( 'NONE', #29885, 1000.000000000000000 ) ;
#33261 = ORIENTED_EDGE ( 'NONE', *, *, #28534, .T. ) ;
#33262 = CARTESIAN_POINT ( 'NONE',  ( -8.000000000000008882, 207.0476921513413515, 0.5011379180785658916 ) ) ;
#33263 = ADVANCED_FACE ( 'NONE', ( #261, #22919 ), #2309, .F. ) ;
#33264 = CARTESIAN_POINT ( 'NONE',  ( -3.753561863808878130, 218.3979405102790281, 93.09886208192145318 ) ) ;
#33265 = CARTESIAN_POINT ( 'NONE',  ( 38.37499999726880873, 155.0000000000000000, 15.58253174999999402 ) ) ;
#33266 = VERTEX_POINT ( 'NONE', #25818 ) ;
#33267 = CARTESIAN_POINT ( 'NONE',  ( 41.32499999726881157, 164.1591823560292198, -12.60653300113719766 ) ) ;
#33268 = DIRECTION ( 'NONE',  ( 0.000000000000000000, 0.000000000000000000, 1.000000000000000000 ) ) ;
#33269 = DIRECTION ( 'NONE',  ( -1.000000000000000000, 0.000000000000000000, 0.000000000000000000 ) ) ;
#33270 = CARTESIAN_POINT ( 'NONE',  ( 8.062137200540822946, 212.9164362838583315, 69.69886208192144750 ) ) ;
#33271 = CARTESIAN_POINT ( 'NONE',  ( 45.47499999726881015, 160.0630714827496206, -15.58253175000000823 ) ) ;
#33272 = CARTESIAN_POINT ( 'NONE',  ( -67.50001199999998391, 150.5921963353448803, 16.45628302766014173 ) ) ;
#33273 = CARTESIAN_POINT ( 'NONE',  ( -7.898309971686851227, 224.1054302408387287, 103.4854814124441447 ) ) ;
#33274 = DIRECTION ( 'NONE',  ( -0.000000000000000000, -0.000000000000000000, 1.000000000000000000 ) ) ;
#33275 = ADVANCED_FACE ( 'NONE', ( #30936 ), #5522, .T. ) ;
#33276 = CARTESIAN_POINT ( 'NONE',  ( 66.29999999999999716, 146.4771138417591203, -11.73074641843674470 ) ) ;
#33277 = CARTESIAN_POINT ( 'NONE',  ( 6.139770520408368348, 198.4640165459539674, 89.45113791807857240 ) ) ;
#33278 = CARTESIAN_POINT ( 'NONE',  ( 63.91132485994280188, 163.8167787843871110, -12.13525491562423397 ) ) ;
#33279 = CARTESIAN_POINT ( 'NONE',  ( 3.135527875058820690, 216.4958274776887492, 79.40113791807857524 ) ) ;
#33280 = DIRECTION ( 'NONE',  ( 1.000000000000000000, 0.000000000000000000, 0.000000000000000000 ) ) ;
#33281 = LINE ( 'NONE', #27819, #24882 ) ;
#33282 = CARTESIAN_POINT ( 'NONE',  ( 0.05014649552828288198, 194.3824533091408000, 88.74886208192143044 ) ) ;
#33283 = CARTESIAN_POINT ( 'NONE',  ( 63.82499999726881867, 168.2552932293087906, 9.630534252274372875 ) ) ;
#33285 = EDGE_LOOP ( 'NONE', ( #12666, #19630, #12351, #13545 ) ) ;
#33284 = CARTESIAN_POINT ( 'NONE',  ( 9.984503880673473830, 203.7031108863295401, 32.15113791807857524 ) ) ;
#33286 = CARTESIAN_POINT ( 'NONE',  ( 99.30625411593993590, 155.0000000000000000, 0.000000000000000000 ) ) ;
#33287 = VECTOR ( 'NONE', #5495, 1000.000000000000000 ) ;
#33288 = CARTESIAN_POINT ( 'NONE',  ( 34.69999999453763451, 167.3344367211045096, 8.961492836873468093 ) ) ;
#33289 = CARTESIAN_POINT ( 'NONE',  ( -7.456977232089304408, 196.8216656703010301, 96.05113791807858092 ) ) ;
#33290 = EDGE_CURVE ( 'NONE', #2299, #13676, #23255, .T. ) ;
#33291 =( BOUNDED_CURVE ( )  B_SPLINE_CURVE ( 2, ( #1408, #29690, #13675, #29363, #6347, #16398, #26792, #3455, #33087, #14516, #12638 ),
 .UNSPECIFIED., .F., .F. ) 
 B_SPLINE_CURVE_WITH_KNOTS ( ( 3, 2, 2, 2, 2, 3 ),
 ( 0.6607142857142855874, 0.6642857142857142572, 0.6678571428571427049, 0.6714285714285712636, 0.6749999999999997113, 0.6785714285714283811 ),
 .UNSPECIFIED. ) 
 CURVE ( )  GEOMETRIC_REPRESENTATION_ITEM ( )  RATIONAL_B_SPLINE_CURVE ( ( 1.000000000000000000, 0.9510565162951534202, 1.000000000000000000, 0.9510565162951534202, 1.000000000000000000, 0.9510565162951534202, 1.000000000000000000, 0.9510565162951534202, 1.000000000000000000, 0.9510565162951564178, 0.9999999999999970024 ) ) 
 REPRESENTATION_ITEM ( '' )  );
#33292 = DIRECTION ( 'NONE',  ( -0.000000000000000000, -0.000000000000000000, 1.000000000000000000 ) ) ;
#33293 = ORIENTED_EDGE ( 'NONE', *, *, #26600, .F. ) ;
#33294 = CARTESIAN_POINT ( 'NONE',  ( 8.118202686958138514, 201.1607312380088501, 82.29886208192144181 ) ) ;
#33295 = AXIS2_PLACEMENT_3D ( 'NONE', #4134, #1585, #17091 ) ;
#33296 = CARTESIAN_POINT ( 'NONE',  ( 12.01549611932659367, 203.1486557965466773, 28.14886208192143968 ) ) ;
#33297 = CYLINDRICAL_SURFACE ( 'NONE', #32236, 4.200000000000001954 ) ;
#33298 = CARTESIAN_POINT ( 'NONE',  ( -3.044812012440131443, 216.5253028482142952, 31.10113791807856742 ) ) ;
#33299 = EDGE_CURVE ( 'NONE', #12934, #13672, #4862, .T. ) ;
#33300 = DIRECTION ( 'NONE',  ( -1.000000000000000000, 0.000000000000000000, 0.000000000000000000 ) ) ;
#33301 = CARTESIAN_POINT ( 'NONE',  ( 6.220909254589681581, 198.5229672870052582, 94.44886208192140487 ) ) ;
#33302 = CARTESIAN_POINT ( 'NONE',  ( 0.8808064505786590281, 6.997019658119588925, -5.875704392892181716 ) ) ;
#33303 = ORIENTED_EDGE ( 'NONE', *, *, #33053, .F. ) ;
#33304 = CARTESIAN_POINT ( 'NONE',  ( 70.51132485994280330, 163.8167787843871110, 12.13525491562421621 ) ) ;
#33305 = CARTESIAN_POINT ( 'NONE',  ( -7.984503880673422316, 204.3529502787951628, 83.34886208192143897 ) ) ;
#33306 = ORIENTED_EDGE ( 'NONE', *, *, #27006, .F. ) ;
#33307 = CARTESIAN_POINT ( 'NONE',  ( 34.01132485994281041, 167.7597621252805880, -9.270509831248443078 ) ) ;
#33308 = VERTEX_POINT ( 'NONE', #33311 ) ;
#33309 = LINE ( 'NONE', #28200, #9635 ) ;
#33310 = CARTESIAN_POINT ( 'NONE',  ( 84.02499999726882152, 160.0630714827496206, 15.58253174999999402 ) ) ;
#33311 = CARTESIAN_POINT ( 'NONE',  ( -52.50000000000002132, 155.0000000000000000, -16.99999999999999645 ) ) ;
#33312 = CARTESIAN_POINT ( 'NONE',  ( -4.984841277089726574, 200.2242689037092305, 75.05113791807858092 ) ) ;
#33313 = DIRECTION ( 'NONE',  ( 0.000000000000000000, 1.000000000000000000, -1.224646799147353207E-16 ) ) ;
#33315 = VECTOR ( 'NONE', #24381, 1000.000000000000227 ) ;
#33314 =( NAMED_UNIT ( * ) SI_UNIT ( $, .STERADIAN. ) SOLID_ANGLE_UNIT ( ) );
#33316 = CARTESIAN_POINT ( 'NONE',  ( 42.89999999999999858, 168.7903194862797420, -4.480746418436745593 ) ) ;
#33317 = CARTESIAN_POINT ( 'NONE',  ( -4.984841277089891776, 213.7757310962905990, 62.94886208192144039 ) ) ;
#33318 = ADVANCED_FACE ( 'NONE', ( #15421 ), #2481, .F. ) ;
#33319 = EDGE_CURVE ( 'NONE', #1999, #27806, #20871, .T. ) ;
#33320 = CARTESIAN_POINT ( 'NONE',  ( 6.139770520408367460, 198.4640165459539389, 2.451137918078566180 ) ) ;
#33321 = DIRECTION ( 'NONE',  ( 1.000000000000000000, -0.000000000000000000, -0.000000000000000000 ) ) ;
#33322 = CARTESIAN_POINT ( 'NONE',  ( 16.00000000000000000, 0.000000000000000000, 1.610000000000000098 ) ) ;
#33323 = CARTESIAN_POINT ( 'NONE',  ( 55.32499999726881157, 164.1591823560292198, -12.60653300113719766 ) ) ;
#33324 = CARTESIAN_POINT ( 'NONE',  ( 69.97499999726881015, 169.8198683612136222, 4.815267126137181997 ) ) ;
#33325 = CARTESIAN_POINT ( 'NONE',  ( -3.753561863808691168, 195.6020594897209435, 68.90113791807856103 ) ) ;
#33326 = LINE ( 'NONE', #20383, #12987 ) ;
#33327 = CARTESIAN_POINT ( 'NONE',  ( 12.00000000000000711, 206.9523078486586485, 11.00113791807856600 ) ) ;
#33328 = EDGE_CURVE ( 'NONE', #3168, #29153, #7761, .T. ) ;
#33329 = CARTESIAN_POINT ( 'NONE',  ( 3.135527875058820690, 216.4958274776887492, 76.40113791807857524 ) ) ;
#33330 = CARTESIAN_POINT ( 'NONE',  ( 11.98450388067341876, 210.9467285061363953, 39.84886208192143187 ) ) ;
#33331 = AXIS2_PLACEMENT_3D ( 'NONE', #9385, #22162, #19781 ) ;
#33332 = CARTESIAN_POINT ( 'NONE',  ( 6.220909254589680693, 198.5229672870052582, 58.44886208192144039 ) ) ;
#33333 = DIRECTION ( 'NONE',  ( -1.000000000000000000, 0.000000000000000000, 0.000000000000000000 ) ) ;
#33334 = CARTESIAN_POINT ( 'NONE',  ( -3.753561863808691168, 195.6020594897209435, 92.90113791807857524 ) ) ;
#33335 = CARTESIAN_POINT ( 'NONE',  ( 73.88867513459481984, 150.1262045565060248, 14.99999999999975842 ) ) ;
#33336 = CARTESIAN_POINT ( 'NONE',  ( -6.220909254589537696, 198.5229672870051161, 3.051137918078564937 ) ) ;
#33337 = ADVANCED_FACE ( 'NONE', ( #28703 ), #10656, .F. ) ;
#33338 = CARTESIAN_POINT ( 'NONE',  ( 8.118202686958138514, 201.1607312380088501, 73.29886208192142760 ) ) ;
#33339 = FACE_OUTER_BOUND ( 'NONE', #4939, .T. ) ;
#33340 = ORIENTED_EDGE ( 'NONE', *, *, #24518, .F. ) ;
#33341 = CARTESIAN_POINT ( 'NONE',  ( 3.753561863808876797, 195.6020594897209719, 70.59886208192142476 ) ) ;
#33342 = CARTESIAN_POINT ( 'NONE',  ( 8.062137200540920645, 201.0835637161417822, 89.30113791807858092 ) ) ;
#33343 = CIRCLE ( 'NONE', #14283, 2.149999999999985256 ) ;
#33344 = EDGE_LOOP ( 'NONE', ( #10962, #23738, #26838, #30531 ) ) ;
#33345 = CARTESIAN_POINT ( 'NONE',  ( 80.47499999726881015, 149.9369285172503510, 15.58253174999999580 ) ) ;
#33346 = CARTESIAN_POINT ( 'NONE',  ( -2.517493886309087880, 214.5937144450984135, 54.09886208192143897 ) ) ;
#33347 = VECTOR ( 'NONE', #3828, 1000.000000000000000 ) ;
#33348 = ORIENTED_EDGE ( 'NONE', *, *, #6390, .F. ) ;
#33349 = CARTESIAN_POINT ( 'NONE',  ( 70.22499999726879594, 149.9369285172503510, 15.58253174999999580 ) ) ;
#33350 = CARTESIAN_POINT ( 'NONE',  ( 6.838238910409970117, -3.993980678889271552, -6.572970348078615466 ) ) ;
#33351 = DIRECTION ( 'NONE',  ( 1.000000000000000000, 0.000000000000000000, 0.000000000000000000 ) ) ;
#33352 = CARTESIAN_POINT ( 'NONE',  ( 65.82499999726881867, 168.2552932293087906, 9.630534252274372875 ) ) ;
#33353 = DIRECTION ( 'NONE',  ( -1.000000000000000000, 0.000000000000000000, 0.000000000000000000 ) ) ;
#33354 = CARTESIAN_POINT ( 'NONE',  ( 8.118202686958138514, 201.1607312380088501, 49.29886208192143471 ) ) ;
#33355 = EDGE_LOOP ( 'NONE', ( #12089, #23947, #6518, #19167 ) ) ;
#33356 = FACE_OUTER_BOUND ( 'NONE', #18097, .T. ) ;
#33357 = AXIS2_PLACEMENT_3D ( 'NONE', #29638, #10751, #23850 ) ;
#33358 = SURFACE_SIDE_STYLE ('',( #7466 ) ) ;
#33359 = CARTESIAN_POINT ( 'NONE',  ( -52.50000000000002132, 155.0000000000000000, 6.938893903907228378E-15 ) ) ;
#33360 = LINE ( 'NONE', #22962, #13122 ) ;
#33361 = CARTESIAN_POINT ( 'NONE',  ( 4.903702542908435547, 213.8346818373419751, 27.54886208192144181 ) ) ;
#33362 = CARTESIAN_POINT ( 'NONE',  ( 8.118202686958039038, 212.8392687619912635, 73.70113791807857240 ) ) ;
#33363 = DIRECTION ( 'NONE',  ( 0.000000000000000000, 0.000000000000000000, -1.000000000000000000 ) ) ;
#33364 = CARTESIAN_POINT ( 'NONE',  ( 8.118202686958039038, 212.8392687619912635, 52.70113791807857240 ) ) ;
#33365 = CONTEXT_DEPENDENT_SHAPE_REPRESENTATION ( #20327, #26670 ) ;
#33366 = CARTESIAN_POINT ( 'NONE',  ( -10.00000000000000711, 207.0476921513413515, 30.50113791807856600 ) ) ;
#33367 = CARTESIAN_POINT ( 'NONE',  ( 8.015496119326531499, 209.5516654185219636, 1.851137918078566091 ) ) ;
#33368 = CONICAL_SURFACE ( 'NONE', #3977, 12.00000000000001066, 0.1047197551196188681 ) ;
#33369 = DIRECTION ( 'NONE',  ( -1.000000000000000000, 0.000000000000000000, -0.000000000000000000 ) ) ;
#33370 = CARTESIAN_POINT ( 'NONE',  ( 38.12499999726880873, 155.0000000000000000, 15.58253174999999402 ) ) ;
#33371 = CARTESIAN_POINT ( 'NONE',  ( -9.680171189290831535, 214.0920067884431148, 33.80113791807856671 ) ) ;
#33372 = PLANE ( 'NONE',  #9150 ) ;
#33373 = VECTOR ( 'NONE', #11678, 1000.000000000000000 ) ;
#33374 = CARTESIAN_POINT ( 'NONE',  ( -3.044812012440131443, 216.5253028482142952, 88.10113791807857808 ) ) ;
#33375 = CARTESIAN_POINT ( 'NONE',  ( -8.062137200540920645, 212.9164362838581894, 45.80113791807856671 ) ) ;
#33376 = FACE_OUTER_BOUND ( 'NONE', #25378, .T. ) ;
#33377 = CARTESIAN_POINT ( 'NONE',  ( 3.753561863808876797, 195.6020594897209719, 10.59886208192143542 ) ) ;
#33378 = CARTESIAN_POINT ( 'NONE',  ( -6.139770520408224463, 198.4640165459539105, 26.04886208192143826 ) ) ;
#33379 = CARTESIAN_POINT ( 'NONE',  ( 76.19999999453763451, 163.5228861582408797, -11.73074641843674470 ) ) ;
#33380 = VERTEX_POINT ( 'NONE', #13196 ) ;
#33381 = CARTESIAN_POINT ( 'NONE',  ( -3.662846001190052991, 218.4274158808045740, 58.10113791807857808 ) ) ;
#33382 = CARTESIAN_POINT ( 'NONE',  ( 2.426778023690261410, 199.3768101843759837, 77.60113791807854966 ) ) ;
#33383 = CARTESIAN_POINT ( 'NONE',  ( -10.01549611932659722, 210.2015048109875011, 41.64886208192144323 ) ) ;
#33384 = CARTESIAN_POINT ( 'NONE',  ( 125.0000000000000000, 25.00000000000004619, -35.00000000000000000 ) ) ;
#33385 = ORIENTED_EDGE ( 'NONE', *, *, #7035, .F. ) ;
#33386 = CARTESIAN_POINT ( 'NONE',  ( -12.01549611932659722, 210.8513442034533227, 38.64886208192143613 ) ) ;
#33387 = ORIENTED_EDGE ( 'NONE', *, *, #10237, .F. ) ;
#33388 = PRESENTATION_LAYER_ASSIGNMENT (  '', '', ( #14337 ) ) ;
#33389 = VERTEX_POINT ( 'NONE', #7420 ) ;
#33390 = CARTESIAN_POINT ( 'NONE',  ( 51.18867513459482410, 169.2658477444273331, -4.635254915624224203 ) ) ;
#33391 = CARTESIAN_POINT ( 'NONE',  ( -63.50000000000001421, 210.0000000000000000, -3.061616997868383141E-16 ) ) ;
#33392 = ORIENTED_EDGE ( 'NONE', *, *, #9725, .T. ) ;
#33393 =( GEOMETRIC_REPRESENTATION_CONTEXT ( 3 ) GLOBAL_UNCERTAINTY_ASSIGNED_CONTEXT ( ( #13720 ) ) GLOBAL_UNIT_ASSIGNED_CONTEXT ( ( #17903, #334, #10078 ) ) REPRESENTATION_CONTEXT ( 'NONE', 'WORKASPACE' ) );
#33394 = CARTESIAN_POINT ( 'NONE',  ( 8.000000000000008882, 206.9523078486586485, 29.00113791807856956 ) ) ;
#33395 = AXIS2_PLACEMENT_3D ( 'NONE', #17415, #4466, #1918 ) ;
#33396 = DIRECTION ( 'NONE',  ( 1.000000000000000000, 0.000000000000000000, 0.000000000000000000 ) ) ;
#33397 = CARTESIAN_POINT ( 'NONE',  ( 8.062137200540822946, 212.9164362838583315, 12.69886208192143506 ) ) ;
#33398 = CONICAL_SURFACE ( 'NONE', #4550, 31.00000000000000000, 1.466076571675255957 ) ;
#33399 = CARTESIAN_POINT ( 'NONE',  ( 58.67499999726880588, 141.7447067706911810, 9.630534252274376428 ) ) ;
#33400 = ORIENTED_EDGE ( 'NONE', *, *, #26600, .T. ) ;
#33401 = CARTESIAN_POINT ( 'NONE',  ( -7.984503880673488041, 209.6470497212046098, 57.65113791807858945 ) ) ;
#33402 = FACE_OUTER_BOUND ( 'NONE', #18621, .T. ) ;
#33403 = CARTESIAN_POINT ( 'NONE',  ( -10.00000000000000711, 206.9523078486584495, 101.4988620819214304 ) ) ;
#33404 = CARTESIAN_POINT ( 'NONE',  ( 63.77499999726880731, 169.8198683612136222, -4.815267126137197984 ) ) ;
#33405 = CARTESIAN_POINT ( 'NONE',  ( 9.984503880673470277, 203.7031108863295401, 41.15113791807855392 ) ) ;
#33406 = CARTESIAN_POINT ( 'NONE',  ( -6.220909254589537696, 198.5229672870051161, 21.05113791807855961 ) ) ;
#33407 = DIRECTION ( 'NONE',  ( 1.000000000000000000, 0.000000000000000000, 0.000000000000000000 ) ) ;
#33408 =( GEOMETRIC_REPRESENTATION_CONTEXT ( 3 ) GLOBAL_UNCERTAINTY_ASSIGNED_CONTEXT ( ( #21231 ) ) GLOBAL_UNIT_ASSIGNED_CONTEXT ( ( #6018, #24883, #25220 ) ) REPRESENTATION_CONTEXT ( 'NONE', 'WORKASPACE' ) );
#33409 = CARTESIAN_POINT ( 'NONE',  ( 34.52499999726880731, 140.1801316387863778, 4.815267126137185549 ) ) ;
#33410 = CARTESIAN_POINT ( 'NONE',  ( -6.901579824520442941, 4.675625068323816080, -0.7022220667781327030 ) ) ;
#33411 = CARTESIAN_POINT ( 'NONE',  ( 125.5000000000000000, 228.4330392262239116, 76.47359838532422316 ) ) ;
#33412 = CARTESIAN_POINT ( 'NONE',  ( -12.01549611932652972, 203.1486557965464499, 0.3511379180785654808 ) ) ;
#33413 = CARTESIAN_POINT ( 'NONE',  ( -0.3470952277635217520, -8.860649561028104415, -7.493596212620245112 ) ) ;
#33414 = CARTESIAN_POINT ( 'NONE',  ( 49.07499999726880446, 141.7447067706911810, -9.630534252274385310 ) ) ;
#33415 = CARTESIAN_POINT ( 'NONE',  ( 8.118202686958039038, 212.8392687619912635, 43.70113791807857240 ) ) ;
#33416 = DIRECTION ( 'NONE',  ( -1.000000000000000000, 0.000000000000000000, 0.000000000000000000 ) ) ;
#33417 = CARTESIAN_POINT ( 'NONE',  ( -62.70000000000000284, -88.00000000000000000, -20.00000000000000000 ) ) ;
#33418 = CARTESIAN_POINT ( 'NONE',  ( -31.74999999999995737, 0.000000000000000000, 0.000000000000000000 ) ) ;
#33419 = CARTESIAN_POINT ( 'NONE',  ( 55.99999999453762456, 155.0000000000000000, -14.50000000000000711 ) ) ;
#33420 = ORIENTED_EDGE ( 'NONE', *, *, #33140, .T. ) ;
#33421 = CARTESIAN_POINT ( 'NONE',  ( -3.753561863808691168, 195.6020594897209435, 26.90113791807856813 ) ) ;
#33422 = CIRCLE ( 'NONE', #18176, 1.650000000000000133 ) ;
#33423 = DIRECTION ( 'NONE',  ( 1.000000000000000000, 0.000000000000000000, 0.000000000000000000 ) ) ;
#33424 = ADVANCED_FACE ( 'NONE', ( #18483 ), #21934, .T. ) ;
#33425 = CARTESIAN_POINT ( 'NONE',  ( 8.118202686958138514, 201.1607312380088501, 7.298862081921435596 ) ) ;
#33426 = ORIENTED_EDGE ( 'NONE', *, *, #16237, .T. ) ;
#33427 = CARTESIAN_POINT ( 'NONE',  ( 8.062137200540920645, 201.0835637161417822, 11.30113791807856671 ) ) ;
#33428 = CARTESIAN_POINT ( 'NONE',  ( 0.05014649552810505201, 217.5146222423826714, 67.25113791807856956 ) ) ;
#33429 = ORIENTED_EDGE ( 'NONE', *, *, #12430, .F. ) ;
#33430 = CARTESIAN_POINT ( 'NONE',  ( -6.500168698208244500, 211.6636982574061676, 20.79886208192143826 ) ) ;
#33431 =( GEOMETRIC_REPRESENTATION_CONTEXT ( 3 ) GLOBAL_UNCERTAINTY_ASSIGNED_CONTEXT ( ( #22633 ) ) GLOBAL_UNIT_ASSIGNED_CONTEXT ( ( #506, #21277, #10573 ) ) REPRESENTATION_CONTEXT ( 'NONE', 'WORKASPACE' ) );
#33432 = CARTESIAN_POINT ( 'NONE',  ( 4.358513833876415333, 4.989164364209877967, -0.07763482564820642362 ) ) ;
#33433 = ORIENTED_EDGE ( 'NONE', *, *, #30736, .T. ) ;
#33434 = CARTESIAN_POINT ( 'NONE',  ( 8.015496119326531499, 209.5516654185219636, 7.851137918078565647 ) ) ;
#33435 = CARTESIAN_POINT ( 'NONE',  ( -12.00000000000000711, 206.9523078486584780, 89.49886208192144466 ) ) ;
#33436 = CARTESIAN_POINT ( 'NONE',  ( 37.77499999726881441, 169.8198683612136222, -4.815267126137197984 ) ) ;
#33437 = ORIENTED_EDGE ( 'NONE', *, *, #9924, .T. ) ;
#33438 = CARTESIAN_POINT ( 'NONE',  ( 47.02499999726881441, 149.9369285172503510, -15.58253175000000823 ) ) ;
#33439 = CARTESIAN_POINT ( 'NONE',  ( 7.500000000000000888, 2.932633423934449812, -0.4709827563909316783 ) ) ;
#33440 = CARTESIAN_POINT ( 'NONE',  ( -0.05014649552810635652, 196.4853777576173002, 11.75113791807856778 ) ) ;
#33441 = AXIS2_PLACEMENT_3D ( 'NONE', #15635, #28260, #22970 ) ;
#33442 = CARTESIAN_POINT ( 'NONE',  ( 9.984503880673420539, 210.2968891136705167, 72.84886208192143897 ) ) ;
#33443 = CARTESIAN_POINT ( 'NONE',  ( 44.77499999726881441, 140.1801316387863778, 4.815267126137185549 ) ) ;
#33444 = CARTESIAN_POINT ( 'NONE',  ( -67.50001199999999812, 150.5921963353448803, -16.45628302766012752 ) ) ;
#33445 = CARTESIAN_POINT ( 'NONE',  ( -3.135527875058821579, 197.5041725223112223, 17.90113791807856458 ) ) ;
#33446 = CARTESIAN_POINT ( 'NONE',  ( 58.71132485994280614, 155.0000000000000000, 15.00000000000001243 ) ) ;
#33447 = CARTESIAN_POINT ( 'NONE',  ( 69.60000000000000853, 150.2886644046228639, 14.49999999999999645 ) ) ;
#33448 = CARTESIAN_POINT ( 'NONE',  ( -10.01549611932653860, 203.7984951890123284, 102.3511379180785781 ) ) ;
#33449 = CARTESIAN_POINT ( 'NONE',  ( 115.4999999999999858, 127.5651812191323557, -102.3881375866411645 ) ) ;
#33450 = EDGE_CURVE ( 'NONE', #25547, #19912, #5364, .T. ) ;
#33451 = CARTESIAN_POINT ( 'NONE',  ( -0.05014649552810635652, 196.4853777576173002, 77.75113791807856956 ) ) ;
#33452 = LINE ( 'NONE', #20333, #28156 ) ;
#33453 = CARTESIAN_POINT ( 'NONE',  ( -3.753561863808878130, 218.3979405102790281, 87.09886208192143897 ) ) ;
#33454 = CARTESIAN_POINT ( 'NONE',  ( 67.62499999726881583, 171.3844434931184253, -7.942151717890132712E-15 ) ) ;
#33455 = ORIENTED_EDGE ( 'NONE', *, *, #12220, .T. ) ;
#33456 = CARTESIAN_POINT ( 'NONE',  ( -60.15281075484971041, 194.9558321103198466, 1.882765505879504309 ) ) ;
#33457 = CARTESIAN_POINT ( 'NONE',  ( 36.99999999453763166, 155.0000000000000000, 14.49999999999999467 ) ) ;
#33458 = CARTESIAN_POINT ( 'NONE',  ( -3.662846001190052991, 218.4274158808045740, 94.10113791807857808 ) ) ;
#33459 = CARTESIAN_POINT ( 'NONE',  ( 125.0000000000000568, -102.9999999999999716, -30.00000000000000000 ) ) ;
#33460 = EDGE_CURVE ( 'NONE', #23779, #2760, #2652, .T. ) ;
#33461 = ORIENTED_EDGE ( 'NONE', *, *, #24492, .F. ) ;
#33462 = CARTESIAN_POINT ( 'NONE',  ( -0.05014649552828402690, 217.5146222423826714, 84.24886208192143044 ) ) ;
#33463 = CARTESIAN_POINT ( 'NONE',  ( -9.736236675708031640, 214.0148392665760753, 23.79886208192143826 ) ) ;
#33464 = CARTESIAN_POINT ( 'NONE',  ( -65.20000000000000284, -0.9203920079924774456, 19.30000000000001847 ) ) ;
#33465 = EDGE_CURVE ( 'NONE', #30017, #30624, #24695, .T. ) ;
#33466 = CARTESIAN_POINT ( 'NONE',  ( -0.05014649552810635652, 196.4853777576173002, 38.75113791807856956 ) ) ;
#33467 = ORIENTED_EDGE ( 'NONE', *, *, #13261, .T. ) ;
#33468 = CARTESIAN_POINT ( 'NONE',  ( 9.984503880673420539, 210.2968891136705167, 99.84886208192141055 ) ) ;
#33469 = EDGE_CURVE ( 'NONE', #22659, #17495, #8905, .T. ) ;
#33470 = CARTESIAN_POINT ( 'NONE',  ( 93.60208470531338776, 155.0000000000000000, -12.00000000000001066 ) ) ;
#33471 = EDGE_LOOP ( 'NONE', ( #23660, #8535, #26756, #15890 ) ) ;
#33472 = LINE ( 'NONE', #7412, #32507 ) ;
#33473 = CARTESIAN_POINT ( 'NONE',  ( -6.500168698208244500, 211.6636982574061676, 80.79886208192144181 ) ) ;
#33474 = ORIENTED_EDGE ( 'NONE', *, *, #27431, .F. ) ;
#33475 = DIRECTION ( 'NONE',  ( 1.000000000000000000, 0.000000000000000000, 0.000000000000000000 ) ) ;
#33476 = ORIENTED_EDGE ( 'NONE', *, *, #11256, .T. ) ;
#33477 = CARTESIAN_POINT ( 'NONE',  ( 81.61132485994282604, 150.1262045565065364, -15.00000000000012434 ) ) ;
#33478 = CARTESIAN_POINT ( 'NONE',  ( -4.984841277089726574, 200.2242689037092305, 60.05113791807858092 ) ) ;
#33479 = CARTESIAN_POINT ( 'NONE',  ( 83.52499999726880731, 169.8198683612136222, -4.815267126137197984 ) ) ;
#33480 = ADVANCED_FACE ( 'NONE', ( #16079 ), #6192, .T. ) ;
#33481 = DIRECTION ( 'NONE',  ( -1.000000000000000000, -0.000000000000000000, -0.000000000000000000 ) ) ;
#33482 = CARTESIAN_POINT ( 'NONE',  ( -2.426778023690262742, 214.6231898156240163, 91.10113791807859229 ) ) ;
#33483 = DIRECTION ( 'NONE',  ( 0.000000000000000000, 0.000000000000000000, -1.000000000000000000 ) ) ;
#33484 = CARTESIAN_POINT ( 'NONE',  ( 50.50000000000000000, 155.0000000000000000, -14.50000000000000711 ) ) ;
#33485 = CARTESIAN_POINT ( 'NONE',  ( 0.05014649552828262524, 198.5883022060938572, 61.74886208192144466 ) ) ;
#33486 = CARTESIAN_POINT ( 'NONE',  ( 71.51132485994280330, 146.1832212156128890, -12.13525491562423042 ) ) ;
#33487 = EDGE_CURVE ( 'NONE', #29530, #21262, #17080, .T. ) ;
#33488 = CARTESIAN_POINT ( 'NONE',  ( -10.01549611932653860, 203.7984951890123000, 0.3511379180785656473 ) ) ;
#33489 = CARTESIAN_POINT ( 'NONE',  ( -65.20000000000000284, -7.347880794884118356E-15, -19.30000000000003979 ) ) ;
#33490 = DIRECTION ( 'NONE',  ( 0.000000000000000000, 0.000000000000000000, 1.000000000000000000 ) ) ;
#33491 = CARTESIAN_POINT ( 'NONE',  ( 59.02499999726880731, 149.9369285172503510, -15.58253175000000823 ) ) ;
#33492 = CARTESIAN_POINT ( 'NONE',  ( 72.67499999726881299, 141.7447067706911810, 9.630534252274376428 ) ) ;
#33493 = CARTESIAN_POINT ( 'NONE',  ( -3.753561863808691168, 195.6020594897209435, 65.90113791807856103 ) ) ;
#33494 = CYLINDRICAL_SURFACE ( 'NONE', #28767, 15.00000000000001776 ) ;
#33495 = CARTESIAN_POINT ( 'NONE',  ( 12.00000000000000711, 206.9523078486586485, 14.00113791807856600 ) ) ;
#33496 = CARTESIAN_POINT ( 'NONE',  ( -6.139770520408368348, 215.5359834540460042, 87.95113791807858661 ) ) ;
#33497 = CARTESIAN_POINT ( 'NONE',  ( -7.375838497908014268, 196.7627149292498530, 53.04886208192142760 ) ) ;
#33498 = CARTESIAN_POINT ( 'NONE',  ( -0.05014649552828402690, 217.5146222423826714, 54.24886208192143044 ) ) ;
#33499 = DIRECTION ( 'NONE',  ( -0.000000000000000000, 0.000000000000000000, -1.000000000000000000 ) ) ;
#33500 = CARTESIAN_POINT ( 'NONE',  ( 9.680171189290831535, 199.9079932115568852, 92.30113791807858092 ) ) ;
#33501 = CARTESIAN_POINT ( 'NONE',  ( -67.50001199999999812, 165.3698264620994394, 13.51682963488644162 ) ) ;
#33502 = CARTESIAN_POINT ( 'NONE',  ( -9.984503880673473830, 210.2968891136704315, 6.651137918078564581 ) ) ;
#33503 = CARTESIAN_POINT ( 'NONE',  ( -6.220909254589682469, 215.4770327129946850, 65.94886208192144750 ) ) ;
#33504 = VERTEX_POINT ( 'NONE', #2980 ) ;
#33505 = CARTESIAN_POINT ( 'NONE',  ( 11.98450388067341876, 210.9467285061363953, 81.84886208192142476 ) ) ;
#33506 = CARTESIAN_POINT ( 'NONE',  ( -10.01549611932653860, 203.7984951890123284, 87.35113791807854966 ) ) ;
#33507 = ORIENTED_EDGE ( 'NONE', *, *, #31480, .F. ) ;
#33508 = CARTESIAN_POINT ( 'NONE',  ( 80.97499999726881015, 140.1801316387863778, -4.815267126137194431 ) ) ;
#33509 = CARTESIAN_POINT ( 'NONE',  ( 4.984841277089891776, 200.2242689037093726, 52.44886208192144039 ) ) ;
#33510 = ORIENTED_EDGE ( 'NONE', *, *, #32365, .F. ) ;
#33511 = EDGE_CURVE ( 'NONE', #31655, #17667, #10023, .T. ) ;
#33512 = CARTESIAN_POINT ( 'NONE',  ( 73.02499999726882152, 149.9369285172503510, -15.58253175000000823 ) ) ;
#33513 = DIRECTION ( 'NONE',  ( 1.000000000000000000, -0.000000000000000000, -0.000000000000000000 ) ) ;
#33514 = CARTESIAN_POINT ( 'NONE',  ( -56.01643337169826964, 194.9989636249862599, -0.3293050612182487069 ) ) ;
#33515 = CARTESIAN_POINT ( 'NONE',  ( 66.62499999726881583, 138.6155565068815463, -3.929120461958505118E-15 ) ) ;
#33516 = EDGE_CURVE ( 'NONE', #32153, #20297, #24426, .T. ) ;
#33517 = CARTESIAN_POINT ( 'NONE',  ( -65.20000000000000284, -7.347880794884118356E-15, 19.29999999999998295 ) ) ;
#33518 = CARTESIAN_POINT ( 'NONE',  ( 9.984503880673420539, 210.2968891136705167, 48.84886208192143187 ) ) ;
#33519 = AXIS2_PLACEMENT_3D ( 'NONE', #24993, #17658, #17822 ) ;
#33520 = ORIENTED_EDGE ( 'NONE', *, *, #17444, .T. ) ;
#33521 = CARTESIAN_POINT ( 'NONE',  ( -125.0000000000000000, 0.000000000000000000, 35.00000000000000000 ) ) ;
#33522 =( NAMED_UNIT ( * ) PLANE_ANGLE_UNIT ( ) SI_UNIT ( $, .RADIAN. ) );
#33523 = DIRECTION ( 'NONE',  ( -0.000000000000000000, -0.000000000000000000, 1.000000000000000000 ) ) ;
#33524 =( BOUNDED_CURVE ( )  B_SPLINE_CURVE ( 2, ( #10627, #5001, #2952, #387, #3107, #21002, #10790, #8069, #25946, #10301, #31400 ),
 .UNSPECIFIED., .F., .T. ) 
 B_SPLINE_CURVE_WITH_KNOTS ( ( 3, 2, 2, 2, 2, 3 ),
 ( 0.01785714285714287350, 0.02142857142857142530, 0.02499999999999997710, 0.02857142857142853237, 0.03214285714285719520, 0.03571428571428574700 ),
 .UNSPECIFIED. ) 
 CURVE ( )  GEOMETRIC_REPRESENTATION_ITEM ( )  RATIONAL_B_SPLINE_CURVE ( ( 0.9999999999999988898, 0.9510565162951545304, 1.000000000000000000, 0.9510565162951534202, 1.000000000000000000, 0.9510565162951534202, 1.000000000000000000, 0.9510565162951534202, 1.000000000000000000, 0.9510565162951527540, 1.000000000000000666 ) ) 
 REPRESENTATION_ITEM ( '' )  );
#33525 = CARTESIAN_POINT ( 'NONE',  ( -8.015496119326597224, 209.5516654185217362, 35.64886208192143613 ) ) ;
#33526 = EDGE_CURVE ( 'NONE', #2969, #5005, #1301, .T. ) ;
#33527 = CARTESIAN_POINT ( 'NONE',  ( 8.062137200540920645, 201.0835637161417822, 71.30113791807856671 ) ) ;
#33528 = CARTESIAN_POINT ( 'NONE',  ( 117.5000000000000142, 155.0000000000000000, -70.00000000000002842 ) ) ;
#33529 = CARTESIAN_POINT ( 'NONE',  ( 3.135527875058820690, 216.4958274776887492, 55.40113791807857524 ) ) ;
#33530 = CARTESIAN_POINT ( 'NONE',  ( 8.062137200540920645, 201.0835637161417822, 26.30113791807856671 ) ) ;
#33531 = CARTESIAN_POINT ( 'NONE',  ( -4.903702542908602524, 213.8346818373418898, 9.951137918078567068 ) ) ;
#33532 = CARTESIAN_POINT ( 'NONE',  ( 45.78867513459482552, 155.0000000000000000, 15.00000000000001243 ) ) ;
#33533 = CARTESIAN_POINT ( 'NONE',  ( 32.50000000000000000, 155.0000000000000000, 15.00000000000001243 ) ) ;
#33534 = CARTESIAN_POINT ( 'NONE',  ( 41.12499999726880873, 155.0000000000000000, -15.58253175000000823 ) ) ;
#33535 = CARTESIAN_POINT ( 'NONE',  ( -9.680171189290831535, 214.0920067884431148, 39.80113791807857382 ) ) ;
#33536 = CARTESIAN_POINT ( 'NONE',  ( 62.70000000000001705, -88.00000000000000000, 30.00000000000000000 ) ) ;
#33537 = CARTESIAN_POINT ( 'NONE',  ( -8.062137200540920645, 212.9164362838581894, 87.80113791807856671 ) ) ;
#33538 = CARTESIAN_POINT ( 'NONE',  ( -3.135527875058821579, 197.5041725223112223, 62.90113791807858235 ) ) ;
#33539 = DIRECTION ( 'NONE',  ( 1.000000000000000000, 0.000000000000000000, 0.000000000000000000 ) ) ;
#33540 = CARTESIAN_POINT ( 'NONE',  ( -0.05014649552828442242, 219.6175466908591716, 27.24886208192143755 ) ) ;
#33541 = CARTESIAN_POINT ( 'NONE',  ( 8.118202686958138514, 201.1607312380088501, 28.29886208192143471 ) ) ;
#33542 = CARTESIAN_POINT ( 'NONE',  ( 71.19999999453763451, 146.4771138417591203, 11.73074641843673227 ) ) ;
#33543 = ORIENTED_EDGE ( 'NONE', *, *, #13907, .F. ) ;
#33544 = CARTESIAN_POINT ( 'NONE',  ( 9.680171189290831535, 199.9079932115568852, 68.30113791807856671 ) ) ;
#33545 = CARTESIAN_POINT ( 'NONE',  ( 8.015496119326531499, 209.5516654185219636, 82.85113791807857808 ) ) ;
#33546 = CARTESIAN_POINT ( 'NONE',  ( -10.00000000000000711, 206.9523078486584495, 41.49886208192143044 ) ) ;
#33547 = AXIS2_PLACEMENT_3D ( 'NONE', #33077, #24746, #19629 ) ;
#33548 = FACE_OUTER_BOUND ( 'NONE', #20601, .T. ) ;
#33549 = ORIENTED_EDGE ( 'NONE', *, *, #30419, .F. ) ;
#33550 = CARTESIAN_POINT ( 'NONE',  ( -12.00000000000000711, 206.9523078486584780, 44.49886208192143755 ) ) ;
#33551 = AXIS2_PLACEMENT_3D ( 'NONE', #30064, #6894, #17121 ) ;
#33552 = ORIENTED_EDGE ( 'NONE', *, *, #24122, .T. ) ;
#33553 = ORIENTED_EDGE ( 'NONE', *, *, #8366, .F. ) ;
#33554 = EDGE_CURVE ( 'NONE', #19012, #30720, #7295, .T. ) ;
#33555 = VECTOR ( 'NONE', #27228, 1000.000000000000000 ) ;
#33556 = CARTESIAN_POINT ( 'NONE',  ( 51.28867513459482552, 170.7719333635740497, -7.904646289410545231E-15 ) ) ;
#33557 = CARTESIAN_POINT ( 'NONE',  ( 56.38867513459481984, 140.7341522555726669, -4.635254915624220651 ) ) ;
#33558 = ORIENTED_EDGE ( 'NONE', *, *, #23461, .F. ) ;
#33559 = CARTESIAN_POINT ( 'NONE',  ( 6.444103211791042618, 202.2591342207267644, 44.30113791807857382 ) ) ;
#33560 = ADVANCED_FACE ( 'NONE', ( #3299 ), #11481, .T. ) ;
#33561 = PLANE ( 'NONE',  #5808 ) ;
#33562 = CARTESIAN_POINT ( 'NONE',  ( 3.044812012439969795, 216.5253028482143520, 24.39886208192143613 ) ) ;
#33563 = CARTESIAN_POINT ( 'NONE',  ( 59.97499999726881015, 169.8198683612136222, 4.815267126137181997 ) ) ;
#33564 = VERTEX_POINT ( 'NONE', #29700 ) ;
#33565 = DIRECTION ( 'NONE',  ( 0.000000000000000000, 0.4999999999999994449, -0.8660254037844389297 ) ) ;
#33566 = DIRECTION ( 'NONE',  ( -1.000000000000000000, 0.000000000000000000, -0.000000000000000000 ) ) ;
#33567 = CARTESIAN_POINT ( 'NONE',  ( -6.500168698208244500, 211.6636982574061676, 5.798862081921435596 ) ) ;
#33568 = CARTESIAN_POINT ( 'NONE',  ( 10.01549611932653860, 210.2015048109876716, 40.85113791807857098 ) ) ;
#33569 = FILL_AREA_STYLE ('',( #16004 ) ) ;
#33570 = CARTESIAN_POINT ( 'NONE',  ( -6.139770520408369237, 215.5359834540460042, 24.95113791807855819 ) ) ;
#33571 = CARTESIAN_POINT ( 'NONE',  ( -10.00000000000000178, 206.9999999999998863, 103.5000000000000426 ) ) ;
#33572 = VECTOR ( 'NONE', #25200, 1000.000000000000000 ) ;
#33573 = SHAPE_DEFINITION_REPRESENTATION ( #12151, #1289 ) ;
#33574 = AXIS2_PLACEMENT_3D ( 'NONE', #9211, #9538, #27764 ) ;
#33575 = CARTESIAN_POINT ( 'NONE',  ( 6.500168698208244500, 202.3363017425938324, 82.29886208192144181 ) ) ;
#33576 = CARTESIAN_POINT ( 'NONE',  ( 34.62499999726880873, 138.6155565068815463, -3.929120461958505118E-15 ) ) ;
#33577 = CARTESIAN_POINT ( 'NONE',  ( -66.50402289005056389, 121.5305141831588003, -17.99597710994943967 ) ) ;
#33578 = CARTESIAN_POINT ( 'NONE',  ( -27.50000000000000000, 15.87713240271474824, -15.54379906938135214 ) ) ;
#33579 = CARTESIAN_POINT ( 'NONE',  ( -9.736236675707914401, 199.9851607334237542, 6.201137918078565292 ) ) ;
#33580 = DIRECTION ( 'NONE',  ( 0.000000000000000000, 0.000000000000000000, -1.000000000000000000 ) ) ;
#33581 = CARTESIAN_POINT ( 'NONE',  ( 52.67499999726880588, 141.7447067706911810, 9.630534252274376428 ) ) ;
#33582 = CARTESIAN_POINT ( 'NONE',  ( 6.220909254589536808, 215.4770327129947702, 55.55113791807855961 ) ) ;
#33583 = VECTOR ( 'NONE', #589, 1000.000000000000000 ) ;
#33584 = FACE_OUTER_BOUND ( 'NONE', #13626, .T. ) ;
#33585 = CARTESIAN_POINT ( 'NONE',  ( 52.21132485994282035, 170.7719333635740497, -7.904646289410545231E-15 ) ) ;
#33586 = CARTESIAN_POINT ( 'NONE',  ( 8.118202686958138514, 201.1607312380088501, 4.298862081921434708 ) ) ;
#33587 = CARTESIAN_POINT ( 'NONE',  ( 56.69999999453763451, 167.3344367211045096, 8.961492836873468093 ) ) ;
#33588 = VERTEX_POINT ( 'NONE', #23754 ) ;
#33589 = CARTESIAN_POINT ( 'NONE',  ( 9.736236675707914401, 214.0148392665762458, 40.70113791807857240 ) ) ;
#33590 = CARTESIAN_POINT ( 'NONE',  ( -64.50000000000000000, 120.3589838486224437, 20.00000000000000000 ) ) ;
#33591 = CARTESIAN_POINT ( 'NONE',  ( -8.062137200540822946, 201.0835637161416400, 14.19886208192143684 ) ) ;
#33592 = CARTESIAN_POINT ( 'NONE',  ( 0.1999999999999987899, 0.000000000000000000, 0.000000000000000000 ) ) ;
#33593 = VERTEX_POINT ( 'NONE', #31914 ) ;
#33594 = CARTESIAN_POINT ( 'NONE',  ( -0.05014649552810635652, 196.4853777576173002, 8.751137918078562450 ) ) ;
#33595 = CARTESIAN_POINT ( 'NONE',  ( -0.05014649552810635652, 196.4853777576173002, 68.75113791807855534 ) ) ;
#33596 = VECTOR ( 'NONE', #329, 1000.000000000000000 ) ;
#33597 = ORIENTED_EDGE ( 'NONE', *, *, #4163, .T. ) ;
#33598 = CARTESIAN_POINT ( 'NONE',  ( -0.05014649552828365914, 215.4116977939061144, 33.24886208192144466 ) ) ;
#33599 = MECHANICAL_DESIGN_GEOMETRIC_PRESENTATION_REPRESENTATION (  '', ( #28149 ), #19457 ) ;
#33600 = AXIS2_PLACEMENT_3D ( 'NONE', #13235, #28064, #10192 ) ;
#33601 = VECTOR ( 'NONE', #32424, 1000.000000000000000 ) ;
#33602 = CARTESIAN_POINT ( 'NONE',  ( 79.67499999726881299, 168.2552932293087906, -9.630534252274387086 ) ) ;
#33603 = ORIENTED_EDGE ( 'NONE', *, *, #11020, .F. ) ;
#33604 = CARTESIAN_POINT ( 'NONE',  ( -8.000000000000008882, 207.0476921513413515, 15.50113791807856600 ) ) ;
#33605 = CARTESIAN_POINT ( 'NONE',  ( -3.753561863808878130, 218.3979405102790281, 96.09886208192143897 ) ) ;
#33606 = CARTESIAN_POINT ( 'NONE',  ( 34.57499999726881157, 145.8408176439707802, 12.60653300113718345 ) ) ;
#33607 = ORIENTED_EDGE ( 'NONE', *, *, #22607, .T. ) ;
#33608 = CARTESIAN_POINT ( 'NONE',  ( 41.52499999726881441, 169.8198683612136222, -4.815267126137197984 ) ) ;
#33609 = CARTESIAN_POINT ( 'NONE',  ( 0.000000000000000000, 4.685197434473814759, -5.637851296924623057E-15 ) ) ;
#33610 = CARTESIAN_POINT ( 'NONE',  ( 10.00000000000000711, 206.9523078486586201, 11.00113791807856600 ) ) ;
#33611 = CARTESIAN_POINT ( 'NONE',  ( 8.062137200540822946, 212.9164362838583315, 75.69886208192143329 ) ) ;
#33612 = CARTESIAN_POINT ( 'NONE',  ( 45.57499999726881157, 164.1591823560292198, -12.60653300113719766 ) ) ;
#33613 = CARTESIAN_POINT ( 'NONE',  ( -67.50001199999998391, 144.6301735379005322, -13.51682963488642564 ) ) ;
#33614 = CARTESIAN_POINT ( 'NONE',  ( -10.01549611932653860, 203.7984951890123284, 15.35113791807856565 ) ) ;
#33615 = LINE ( 'NONE', #28340, #32254 ) ;
#33616 = CARTESIAN_POINT ( 'NONE',  ( 70.29999999999999716, 146.4771138417591203, -11.73074641843674470 ) ) ;
#33617 = CARTESIAN_POINT ( 'NONE',  ( -8.118202686958039038, 201.1607312380087080, 102.2011379180785866 ) ) ;
#33618 = CARTESIAN_POINT ( 'NONE',  ( -27.50000000000000355, 0.000000000000000000, 0.000000000000000000 ) ) ;
#33619 = CARTESIAN_POINT ( 'NONE',  ( 9.984503880673470277, 203.7031108863295401, 80.15113791807858945 ) ) ;
#33620 = VECTOR ( 'NONE', #33187, 1000.000000000000000 ) ;
#33621 = CARTESIAN_POINT ( 'NONE',  ( -27.50000000000000000, 5.390523180938844305, -0.2837416352459747881 ) ) ;
#33622 = CARTESIAN_POINT ( 'NONE',  ( 103.3032345859876102, 155.0000000000000000, -31.00000000000000000 ) ) ;
#33623 = CARTESIAN_POINT ( 'NONE',  ( 12.00000000000000711, 207.0476921513415220, 99.99886208192143044 ) ) ;
#33624 = VECTOR ( 'NONE', #24201, 1000.000000000000000 ) ;
#33625 = CARTESIAN_POINT ( 'NONE',  ( 72.32499999726880446, 145.8408176439707802, 12.60653300113718345 ) ) ;
#33626 = ORIENTED_EDGE ( 'NONE', *, *, #20817, .T. ) ;
#33627 = LINE ( 'NONE', #25448, #10314 ) ;
#33628 = CARTESIAN_POINT ( 'NONE',  ( 36.39999999453763024, 168.7903194862797420, -4.480746418436745593 ) ) ;
#33629 = B_SPLINE_CURVE_WITH_KNOTS ( 'NONE', 3,
 ( #14571, #22402, #30589, #24972, #1626, #12016, #32629, #32964, #32794, #28025 ),
 .UNSPECIFIED., .F., .F.,
 ( 4, 2, 2, 2, 4 ),
 ( 0.01051144076094934904, 0.01162027323572610918, 0.01272910571050286932, 0.01383793818527962946, 0.01494677066005638960 ),
 .UNSPECIFIED. ) ;
#33630 = CARTESIAN_POINT ( 'NONE',  ( 3.662846001190051659, 195.5725841191953691, 92.60113791807857808 ) ) ;
#33631 = CARTESIAN_POINT ( 'NONE',  ( -10.84125907834625480, 206.4200127656791039, 104.0062660280915026 ) ) ;
#33632 = ORIENTED_EDGE ( 'NONE', *, *, #16386, .T. ) ;
#33633 = CARTESIAN_POINT ( 'NONE',  ( -3.135527875058982783, 216.4958274776886924, 87.09886208192143897 ) ) ;
#33634 = CARTESIAN_POINT ( 'NONE',  ( -12.01549611932659722, 210.8513442034533227, 20.64886208192143613 ) ) ;
#33635 = CARTESIAN_POINT ( 'NONE',  ( 13.16654248868335664, -24.15255795529147065, -1.397731417911683705E-14 ) ) ;
#33636 = CARTESIAN_POINT ( 'NONE',  ( 3.044812012440130555, 197.4746971517856764, 38.60113791807857098 ) ) ;
#33637 = ORIENTED_EDGE ( 'NONE', *, *, #9983, .T. ) ;
#33638 = CARTESIAN_POINT ( 'NONE',  ( -4.984841277089891776, 213.7757310962905990, 2.948862081921435063 ) ) ;
#33639 = DIRECTION ( 'NONE',  ( 1.000000000000000000, 0.000000000000000000, -0.000000000000000000 ) ) ;
#33640 = ORIENTED_EDGE ( 'NONE', *, *, #24556, .T. ) ;
#33641 = CARTESIAN_POINT ( 'NONE',  ( 6.500168698208244500, 202.3363017425938324, 79.29886208192144181 ) ) ;
#33642 = CIRCLE ( 'NONE', #22198, 1.499999999999999556 ) ;
#33643 = ORIENTED_EDGE ( 'NONE', *, *, #9297, .T. ) ;
#33644 = DIRECTION ( 'NONE',  ( 5.620504062164857944E-16, -0.9988620819214347746, 0.04769215134146256169 ) ) ;
#33645 = VERTEX_POINT ( 'NONE', #24082 ) ;
#33646 = LINE ( 'NONE', #12354, #10195 ) ;
#33647 = CARTESIAN_POINT ( 'NONE',  ( -7.984503880673488041, 209.6470497212046098, 57.65113791807858945 ) ) ;
#33648 = CARTESIAN_POINT ( 'NONE',  ( 84.42499999726881299, 141.7447067706911810, 9.630534252274376428 ) ) ;
#33649 = CARTESIAN_POINT ( 'NONE',  ( 115.4999999999999858, 63.20130719884917170, -52.99999999999946709 ) ) ;
#33650 = CARTESIAN_POINT ( 'NONE',  ( -6.500168698208129925, 202.3363017425936050, 90.20113791807857240 ) ) ;
#33651 = LINE ( 'NONE', #25645, #27147 ) ;
#33652 = ADVANCED_FACE ( 'NONE', ( #29200 ), #418, .T. ) ;
#33653 = VECTOR ( 'NONE', #12030, 1000.000000000000000 ) ;
#33654 =( NAMED_UNIT ( * ) SI_UNIT ( $, .STERADIAN. ) SOLID_ANGLE_UNIT ( ) );
#33655 = CARTESIAN_POINT ( 'NONE',  ( 49.89999999999999858, 141.2096805137202580, 4.480746418436733158 ) ) ;
#33656 = CARTESIAN_POINT ( 'NONE',  ( -6.444103211790928043, 202.2591342207265939, 68.19886208192143329 ) ) ;
#33657 = CARTESIAN_POINT ( 'NONE',  ( 84.01132485994281751, 167.7597621252805880, -9.270509831248443078 ) ) ;
#33658 = B_SPLINE_CURVE_WITH_KNOTS ( 'NONE', 3,
 ( #11120, #13829, #29844, #3267, #24391, #22002 ),
 .UNSPECIFIED., .F., .F.,
 ( 4, 2, 4 ),
 ( -5.145455527293010977E-06, 0.0004153350442917342006, 0.0008358155441107593302 ),
 .UNSPECIFIED. ) ;
#33659 = EDGE_CURVE ( 'NONE', #14984, #2476, #30142, .T. ) ;
#33660 = CARTESIAN_POINT ( 'NONE',  ( 54.02499999726880020, 160.0630714827496206, 15.58253174999999402 ) ) ;
#33661 = CARTESIAN_POINT ( 'NONE',  ( -0.05014649552810635652, 196.4853777576173002, 2.751137918078565558 ) ) ;
#33662 = DIRECTION ( 'NONE',  ( -0.000000000000000000, -0.000000000000000000, -1.000000000000000000 ) ) ;
#33663 = CARTESIAN_POINT ( 'NONE',  ( 56.22499999726882436, 149.9369285172503510, 15.58253174999999580 ) ) ;
#33664 = CARTESIAN_POINT ( 'NONE',  ( 72.87499999726881583, 138.6155565068815463, -3.929120461958505118E-15 ) ) ;
#33665 = CARTESIAN_POINT ( 'NONE',  ( 3.662846001190051659, 195.5725841191953691, 65.60113791807857808 ) ) ;
#33666 = CARTESIAN_POINT ( 'NONE',  ( -64.50000000000000000, 0.000000000000000000, -20.00000000000000000 ) ) ;
#33667 = CIRCLE ( 'NONE', #5896, 2.500000000000000000 ) ;
#33668 = PRODUCT_DEFINITION_SHAPE ( 'NONE', 'NONE',  #28336 ) ;
#33669 = CARTESIAN_POINT ( 'NONE',  ( -7.375838497908182134, 217.2372850707499765, 9.951137918078567068 ) ) ;
#33670 = CARTESIAN_POINT ( 'NONE',  ( 0.05014649552810506589, 217.5146222423826714, 85.25113791807855534 ) ) ;
#33671 = CARTESIAN_POINT ( 'NONE',  ( -11.98450388067341876, 203.0532714938636047, 47.34886208192143897 ) ) ;
#33672 = CARTESIAN_POINT ( 'NONE',  ( -3.044812012439970683, 197.4746971517856196, 52.89886208192143613 ) ) ;
#33673 = DIRECTION ( 'NONE',  ( -0.000000000000000000, -0.000000000000000000, 1.000000000000000000 ) ) ;
#33674 = CARTESIAN_POINT ( 'NONE',  ( -7.375838497908182134, 217.2372850707499765, 93.95113791807857240 ) ) ;
#33675 = CARTESIAN_POINT ( 'NONE',  ( -67.50001200000001234, 157.2252672838932597, 16.89041650604972133 ) ) ;
#33676 = CARTESIAN_POINT ( 'NONE',  ( 0.05014649552810505201, 217.5146222423826714, 10.25113791807856778 ) ) ;
#33677 = CARTESIAN_POINT ( 'NONE',  ( -6.220909254589682469, 215.4770327129946850, 68.94886208192140487 ) ) ;
#33678 = ORIENTED_EDGE ( 'NONE', *, *, #25603, .T. ) ;
#33679 = CARTESIAN_POINT ( 'NONE',  ( 0.05014649552828288198, 194.3824533091408000, 76.74886208192144466 ) ) ;
#33680 = CARTESIAN_POINT ( 'NONE',  ( -3.044812012440131443, 216.5253028482142952, 94.10113791807857808 ) ) ;
#33681 = EDGE_LOOP ( 'NONE', ( #23930, #19472, #25453, #21979 ) ) ;
#33682 = CARTESIAN_POINT ( 'NONE',  ( 79.37499999726881583, 155.0000000000000000, -15.58253175000000823 ) ) ;
#33683 = CARTESIAN_POINT ( 'NONE',  ( -8.000000000000008882, 206.9523078486584780, 50.49886208192144466 ) ) ;
#33684 = ADVANCED_FACE ( 'NONE', ( #26471 ), #22531, .T. ) ;
#33685 = EDGE_LOOP ( 'NONE', ( #3246, #17629, #23371, #18253 ) ) ;
#33686 = CARTESIAN_POINT ( 'NONE',  ( 71.22499999726879594, 160.0630714827496206, -15.58253175000000823 ) ) ;
#33687 = ORIENTED_EDGE ( 'NONE', *, *, #32425, .F. ) ;
#33688 = NEXT_ASSEMBLY_USAGE_OCCURRENCE ( 'NAUO1', ' ', ' ', #14589, #3132, $ ) ;
#33689 = NEXT_ASSEMBLY_USAGE_OCCURRENCE ( 'NAUO2', ' ', ' ', #14589, #28336, $ ) ;
#33690 = NEXT_ASSEMBLY_USAGE_OCCURRENCE ( 'NAUO3', ' ', ' ', #14589, #29780, $ ) ;
#33691 = NEXT_ASSEMBLY_USAGE_OCCURRENCE ( 'NAUO4', ' ', ' ', #14589, #13732, $ ) ;
#33692 = NEXT_ASSEMBLY_USAGE_OCCURRENCE ( 'NAUO5', ' ', ' ', #14589, #27284, $ ) ;
#33693 = NEXT_ASSEMBLY_USAGE_OCCURRENCE ( 'NAUO6', ' ', ' ', #14589, #32279, $ ) ;
#33694 = NEXT_ASSEMBLY_USAGE_OCCURRENCE ( 'NAUO7', ' ', ' ', #14589, #1660, $ ) ;
#33695 = NEXT_ASSEMBLY_USAGE_OCCURRENCE ( 'NAUO8', ' ', ' ', #14589, #17286, $ ) ;
#33696 = NEXT_ASSEMBLY_USAGE_OCCURRENCE ( 'NAUO9', ' ', ' ', #14589, #6235, $ ) ;
#33697 = NEXT_ASSEMBLY_USAGE_OCCURRENCE ( 'NAUO10', ' ', ' ', #14589, #17286, $ ) ;
#33698 = NEXT_ASSEMBLY_USAGE_OCCURRENCE ( 'NAUO11', ' ', ' ', #14589, #31263, $ ) ;
#33699 = NEXT_ASSEMBLY_USAGE_OCCURRENCE ( 'NAUO12', ' ', ' ', #14589, #31263, $ ) ;
#33700 = NEXT_ASSEMBLY_USAGE_OCCURRENCE ( 'NAUO13', ' ', ' ', #14589, #21056, $ ) ;
#33701 = NEXT_ASSEMBLY_USAGE_OCCURRENCE ( 'NAUO14', ' ', ' ', #14589, #21056, $ ) ;
#33702 = NEXT_ASSEMBLY_USAGE_OCCURRENCE ( 'NAUO15', ' ', ' ', #14589, #21056, $ ) ;
#33703 = NEXT_ASSEMBLY_USAGE_OCCURRENCE ( 'NAUO16', ' ', ' ', #14589, #21056, $ ) ;
#33704 = NEXT_ASSEMBLY_USAGE_OCCURRENCE ( 'NAUO17', ' ', ' ', #14589, #21056, $ ) ;
#33705 = NEXT_ASSEMBLY_USAGE_OCCURRENCE ( 'NAUO18', ' ', ' ', #14589, #21056, $ ) ;
#33706 = NEXT_ASSEMBLY_USAGE_OCCURRENCE ( 'NAUO19', ' ', ' ', #14589, #21056, $ ) ;
#33707 = NEXT_ASSEMBLY_USAGE_OCCURRENCE ( 'NAUO20', ' ', ' ', #14589, #21056, $ ) ;
#33708 = NEXT_ASSEMBLY_USAGE_OCCURRENCE ( 'NAUO21', ' ', ' ', #14589, #33139, $ ) ;
#33709 = NEXT_ASSEMBLY_USAGE_OCCURRENCE ( 'NAUO22', ' ', ' ', #14589, #33139, $ ) ;
#33710 = NEXT_ASSEMBLY_USAGE_OCCURRENCE ( 'NAUO23', ' ', ' ', #14589, #33139, $ ) ;
#33711 = NEXT_ASSEMBLY_USAGE_OCCURRENCE ( 'NAUO24', ' ', ' ', #14589, #33139, $ ) ;
#33712 = NEXT_ASSEMBLY_USAGE_OCCURRENCE ( 'NAUO25', ' ', ' ', #14589, #33139, $ ) ;
#33713 = NEXT_ASSEMBLY_USAGE_OCCURRENCE ( 'NAUO26', ' ', ' ', #14589, #33139, $ ) ;
#33714 = NEXT_ASSEMBLY_USAGE_OCCURRENCE ( 'NAUO27', ' ', ' ', #14589, #33139, $ ) ;
#33715 = NEXT_ASSEMBLY_USAGE_OCCURRENCE ( 'NAUO28', ' ', ' ', #14589, #33139, $ ) ;
#33716 = NEXT_ASSEMBLY_USAGE_OCCURRENCE ( 'NAUO29', ' ', ' ', #14589, #12945, $ ) ;
#33717 = NEXT_ASSEMBLY_USAGE_OCCURRENCE ( 'NAUO30', ' ', ' ', #14589, #12945, $ ) ;
#33718 = NEXT_ASSEMBLY_USAGE_OCCURRENCE ( 'NAUO31', ' ', ' ', #14589, #18980, $ ) ;
#33719 = NEXT_ASSEMBLY_USAGE_OCCURRENCE ( 'NAUO32', ' ', ' ', #14589, #18980, $ ) ;
#33720 = NEXT_ASSEMBLY_USAGE_OCCURRENCE ( 'NAUO33', ' ', ' ', #14589, #1908, $ ) ;
#33721 = NEXT_ASSEMBLY_USAGE_OCCURRENCE ( 'NAUO34', ' ', ' ', #14589, #1908, $ ) ;
#33722 = NEXT_ASSEMBLY_USAGE_OCCURRENCE ( 'NAUO35', ' ', ' ', #14589, #27705, $ ) ;
#33723 = NEXT_ASSEMBLY_USAGE_OCCURRENCE ( 'NAUO36', ' ', ' ', #14589, #27705, $ ) ;
ENDSEC;
END-ISO-10303-21;
